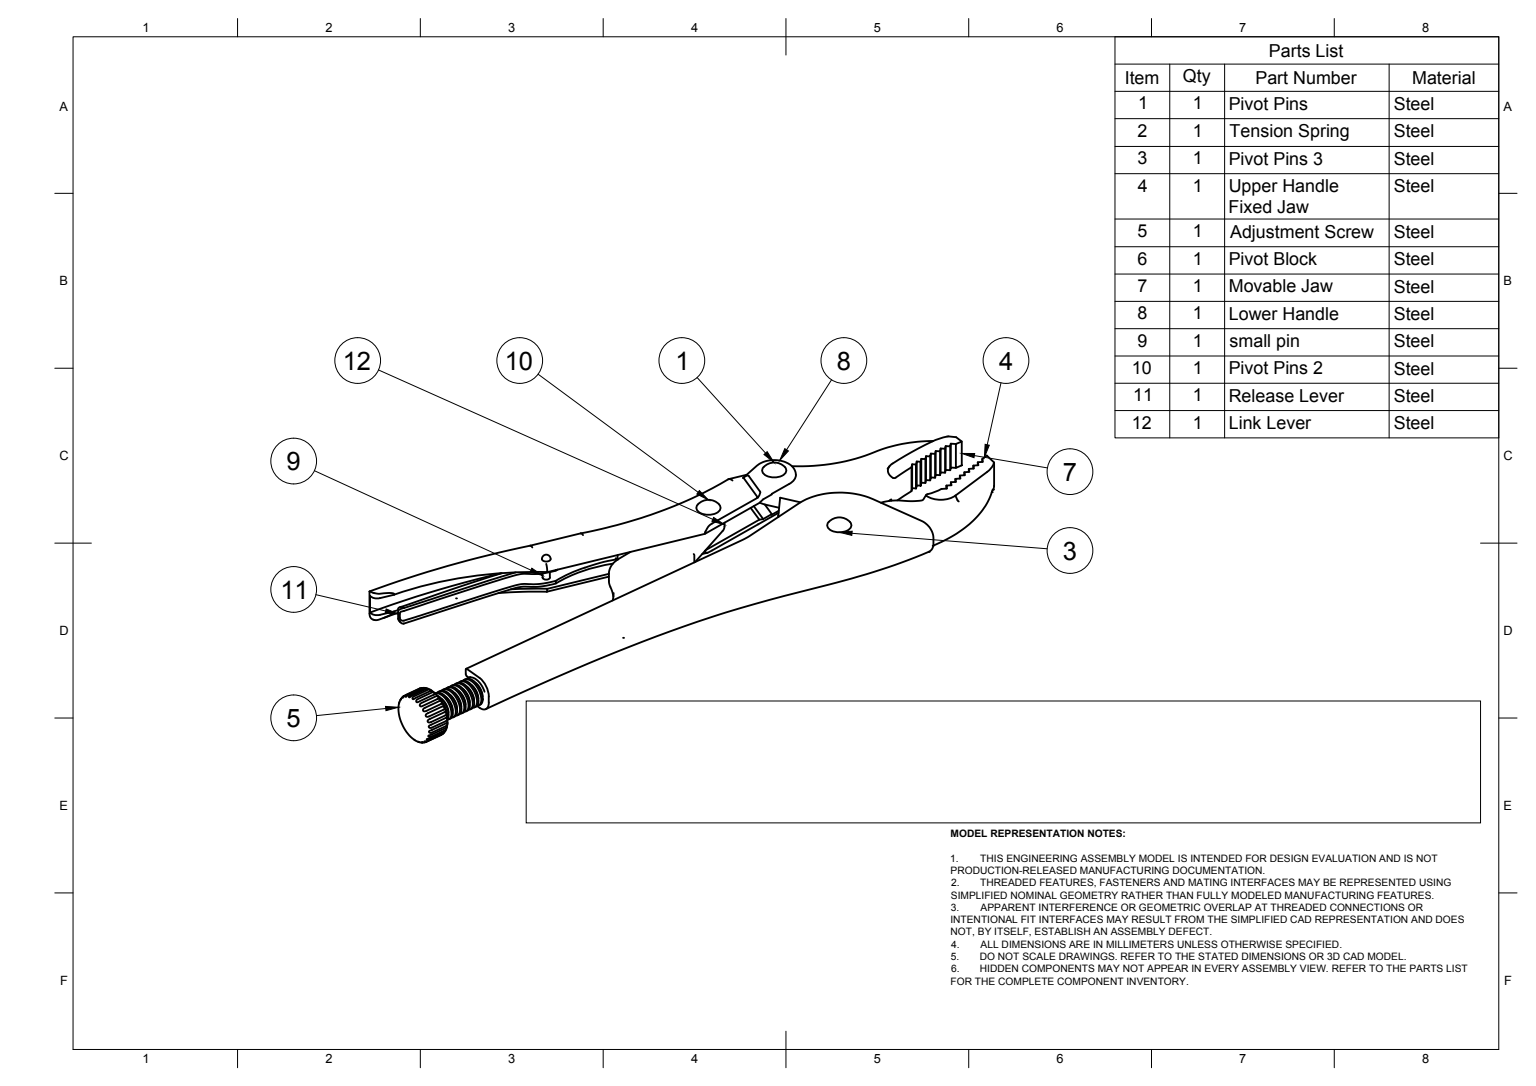
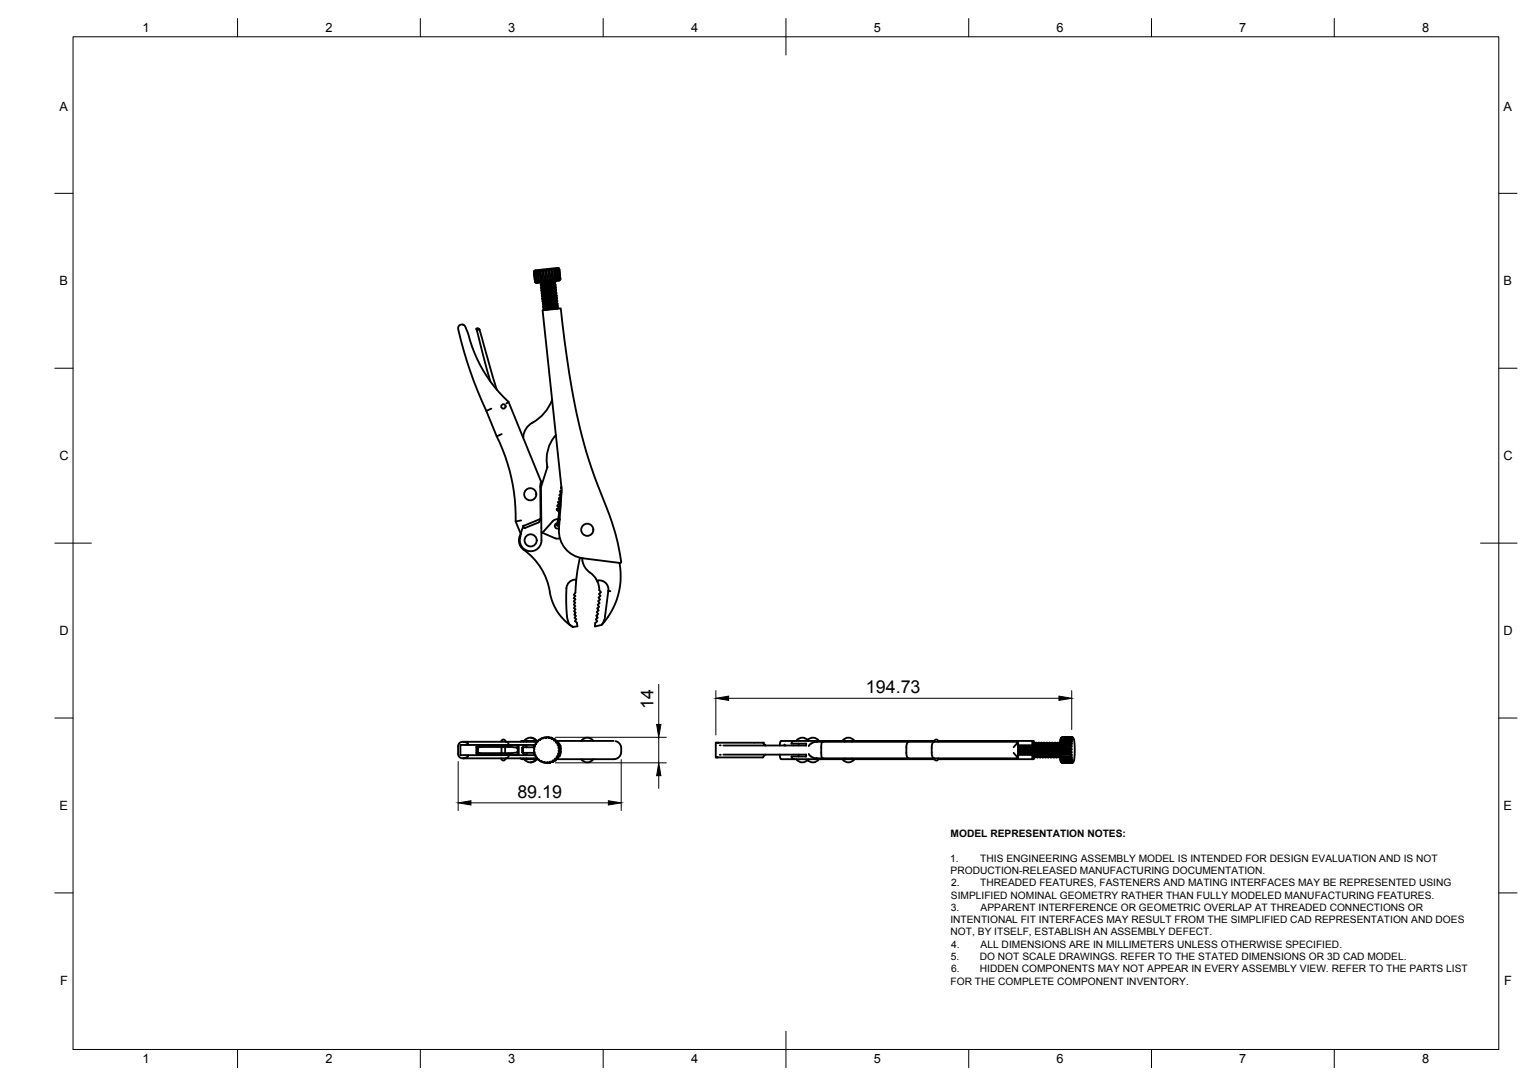
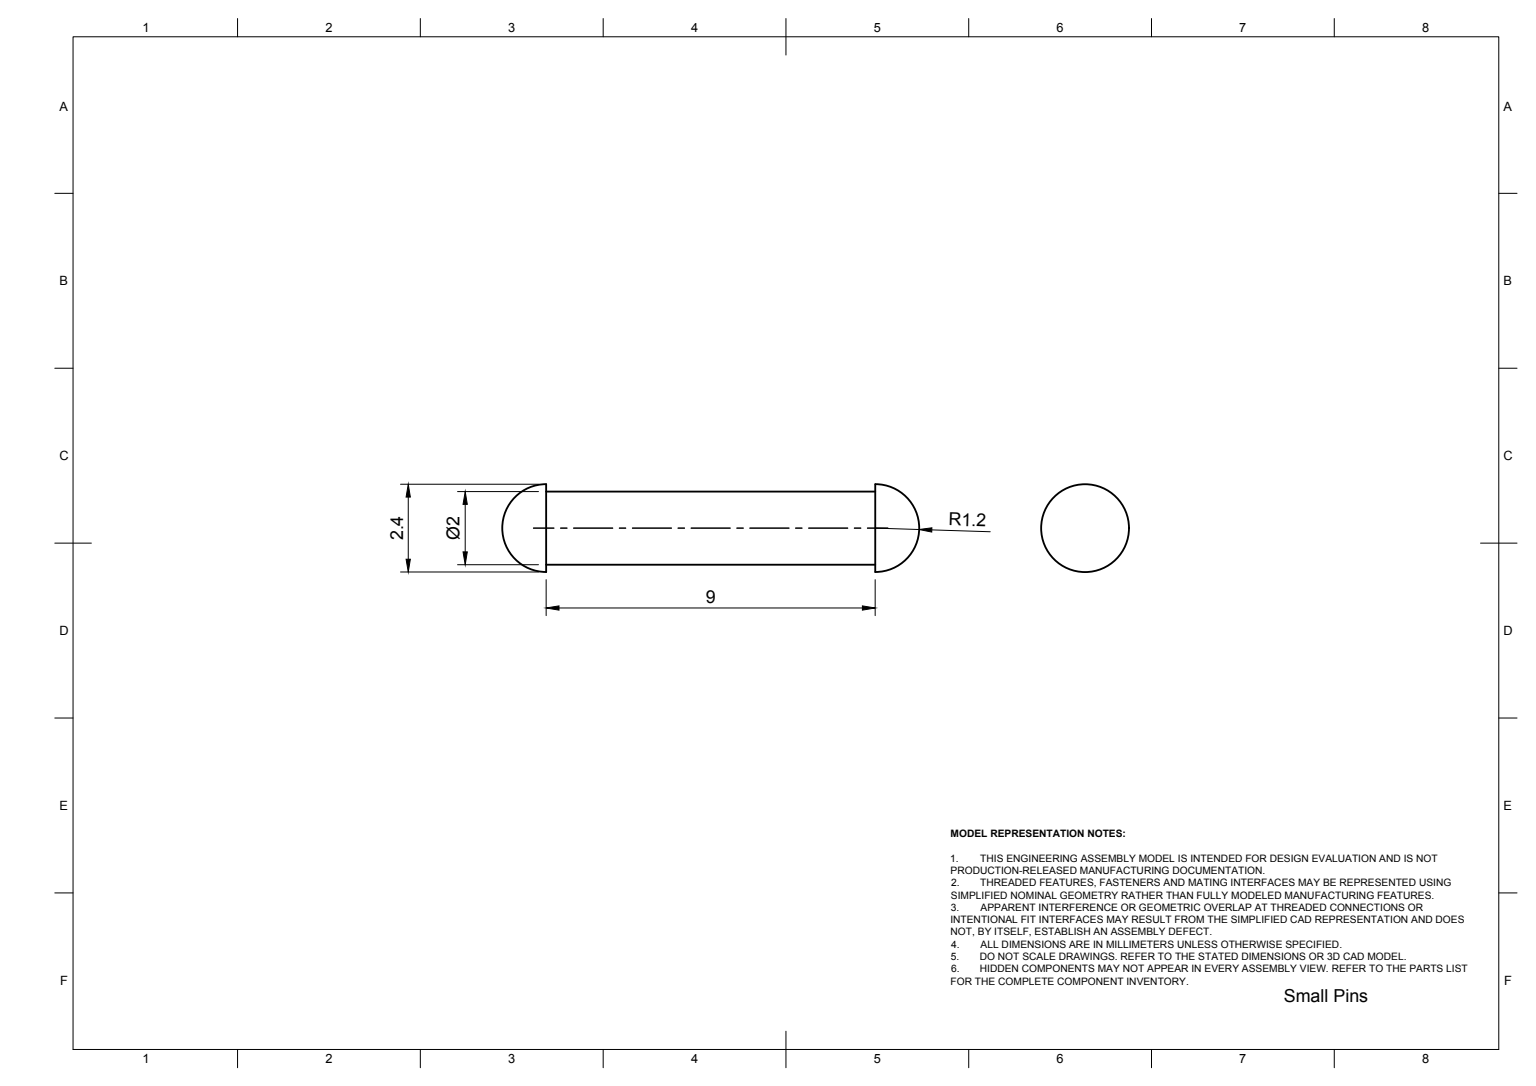
ISO-10303-21;
HEADER;
/* Generated by software containing ST-Developer
 * from STEP Tools, Inc. (www.steptools.com) 
 */

FILE_DESCRIPTION(
/* description */ ('STEP AP214'),
/* implementation_level */ '2;1');

FILE_NAME(
/* name */ 'MAS-610',
/* time_stamp */ '2026-10-06T11:11:25-07:00',
/* author */ (''),
/* organization */ (''),
/* preprocessor_version */ 'ST-DEVELOPER v20.2',
/* originating_system */ 'Autodesk Translation Framework v15.15.0.0',
/* authorisation */ '');

FILE_SCHEMA (('AUTOMOTIVE_DESIGN { 1 0 10303 214 3 1 1 }'));
ENDSEC;

DATA;
#10=MECHANICAL_DESIGN_GEOMETRIC_PRESENTATION_REPRESENTATION('',(#698,#699,
#700,#701,#702,#703,#704,#705,#706,#707,#708,#709),#47717);
#11=ITEM_DEFINED_TRANSFORMATION($,$,#9071,#9944);
#12=ITEM_DEFINED_TRANSFORMATION($,$,#9081,#9945);
#13=ITEM_DEFINED_TRANSFORMATION($,$,#9112,#9946);
#14=ITEM_DEFINED_TRANSFORMATION($,$,#9122,#9947);
#15=ITEM_DEFINED_TRANSFORMATION($,$,#9345,#9948);
#16=ITEM_DEFINED_TRANSFORMATION($,$,#9511,#9949);
#17=ITEM_DEFINED_TRANSFORMATION($,$,#9515,#9950);
#18=ITEM_DEFINED_TRANSFORMATION($,$,#9703,#9951);
#19=ITEM_DEFINED_TRANSFORMATION($,$,#9812,#9952);
#20=ITEM_DEFINED_TRANSFORMATION($,$,#9824,#9953);
#21=ITEM_DEFINED_TRANSFORMATION($,$,#9834,#9954);
#22=ITEM_DEFINED_TRANSFORMATION($,$,#9871,#9955);
#23=(
REPRESENTATION_RELATIONSHIP($,$,#47761,#47760)
REPRESENTATION_RELATIONSHIP_WITH_TRANSFORMATION(#11)
SHAPE_REPRESENTATION_RELATIONSHIP()
);
#24=(
REPRESENTATION_RELATIONSHIP($,$,#47762,#47760)
REPRESENTATION_RELATIONSHIP_WITH_TRANSFORMATION(#12)
SHAPE_REPRESENTATION_RELATIONSHIP()
);
#25=(
REPRESENTATION_RELATIONSHIP($,$,#47763,#47760)
REPRESENTATION_RELATIONSHIP_WITH_TRANSFORMATION(#13)
SHAPE_REPRESENTATION_RELATIONSHIP()
);
#26=(
REPRESENTATION_RELATIONSHIP($,$,#47764,#47760)
REPRESENTATION_RELATIONSHIP_WITH_TRANSFORMATION(#14)
SHAPE_REPRESENTATION_RELATIONSHIP()
);
#27=(
REPRESENTATION_RELATIONSHIP($,$,#47765,#47760)
REPRESENTATION_RELATIONSHIP_WITH_TRANSFORMATION(#15)
SHAPE_REPRESENTATION_RELATIONSHIP()
);
#28=(
REPRESENTATION_RELATIONSHIP($,$,#47766,#47760)
REPRESENTATION_RELATIONSHIP_WITH_TRANSFORMATION(#16)
SHAPE_REPRESENTATION_RELATIONSHIP()
);
#29=(
REPRESENTATION_RELATIONSHIP($,$,#47767,#47760)
REPRESENTATION_RELATIONSHIP_WITH_TRANSFORMATION(#17)
SHAPE_REPRESENTATION_RELATIONSHIP()
);
#30=(
REPRESENTATION_RELATIONSHIP($,$,#47768,#47760)
REPRESENTATION_RELATIONSHIP_WITH_TRANSFORMATION(#18)
SHAPE_REPRESENTATION_RELATIONSHIP()
);
#31=(
REPRESENTATION_RELATIONSHIP($,$,#47769,#47760)
REPRESENTATION_RELATIONSHIP_WITH_TRANSFORMATION(#19)
SHAPE_REPRESENTATION_RELATIONSHIP()
);
#32=(
REPRESENTATION_RELATIONSHIP($,$,#47770,#47760)
REPRESENTATION_RELATIONSHIP_WITH_TRANSFORMATION(#20)
SHAPE_REPRESENTATION_RELATIONSHIP()
);
#33=(
REPRESENTATION_RELATIONSHIP($,$,#47771,#47760)
REPRESENTATION_RELATIONSHIP_WITH_TRANSFORMATION(#21)
SHAPE_REPRESENTATION_RELATIONSHIP()
);
#34=(
REPRESENTATION_RELATIONSHIP($,$,#47772,#47760)
REPRESENTATION_RELATIONSHIP_WITH_TRANSFORMATION(#22)
SHAPE_REPRESENTATION_RELATIONSHIP()
);
#35=CONTEXT_DEPENDENT_SHAPE_REPRESENTATION(#23,#47748);
#36=CONTEXT_DEPENDENT_SHAPE_REPRESENTATION(#24,#47749);
#37=CONTEXT_DEPENDENT_SHAPE_REPRESENTATION(#25,#47750);
#38=CONTEXT_DEPENDENT_SHAPE_REPRESENTATION(#26,#47751);
#39=CONTEXT_DEPENDENT_SHAPE_REPRESENTATION(#27,#47752);
#40=CONTEXT_DEPENDENT_SHAPE_REPRESENTATION(#28,#47753);
#41=CONTEXT_DEPENDENT_SHAPE_REPRESENTATION(#29,#47754);
#42=CONTEXT_DEPENDENT_SHAPE_REPRESENTATION(#30,#47755);
#43=CONTEXT_DEPENDENT_SHAPE_REPRESENTATION(#31,#47756);
#44=CONTEXT_DEPENDENT_SHAPE_REPRESENTATION(#32,#47757);
#45=CONTEXT_DEPENDENT_SHAPE_REPRESENTATION(#33,#47758);
#46=CONTEXT_DEPENDENT_SHAPE_REPRESENTATION(#34,#47759);
#47=NEXT_ASSEMBLY_USAGE_OCCURRENCE('Pivot Pins:1','Pivot Pins:1',
'Pivot Pins:1',#47774,#47775,'Pivot Pins:1');
#48=NEXT_ASSEMBLY_USAGE_OCCURRENCE('Tension Spring:1',
'Tension Spring:1','Tension Spring:1',#47774,#47776,'Tension Spring:1');
#49=NEXT_ASSEMBLY_USAGE_OCCURRENCE('Pivot Pins 3:1','Pivot Pins 3:1',
'Pivot Pins 3:1',#47774,#47777,'Pivot Pins 3:1');
#50=NEXT_ASSEMBLY_USAGE_OCCURRENCE('Upper Handle Fixed Jaw:1',
'Upper Handle Fixed Jaw:1','Upper Handle Fixed Jaw:1',#47774,#47778,
'Upper Handle Fixed Jaw:1');
#51=NEXT_ASSEMBLY_USAGE_OCCURRENCE('Adjustment Screw:1',
'Adjustment Screw:1','Adjustment Screw:1',#47774,#47779,
'Adjustment Screw:1');
#52=NEXT_ASSEMBLY_USAGE_OCCURRENCE('Pivot Block:1','Pivot Block:1',
'Pivot Block:1',#47774,#47780,'Pivot Block:1');
#53=NEXT_ASSEMBLY_USAGE_OCCURRENCE('Movable Jaw:1','Movable Jaw:1',
'Movable Jaw:1',#47774,#47781,'Movable Jaw:1');
#54=NEXT_ASSEMBLY_USAGE_OCCURRENCE('Lower Handle:1','Lower Handle:1',
'Lower Handle:1',#47774,#47782,'Lower Handle:1');
#55=NEXT_ASSEMBLY_USAGE_OCCURRENCE('Small Pin:1','Small Pin:1',
'Small Pin:1',#47774,#47783,'Small Pin:1');
#56=NEXT_ASSEMBLY_USAGE_OCCURRENCE('Pivot Pins 2:1','Pivot Pins 2:1',
'Pivot Pins 2:1',#47774,#47784,'Pivot Pins 2:1');
#57=NEXT_ASSEMBLY_USAGE_OCCURRENCE('Release Lever:1','Release Lever:1',
'Release Lever:1',#47774,#47785,'Release Lever:1');
#58=NEXT_ASSEMBLY_USAGE_OCCURRENCE('Link Lever:1','Link Lever:1',
'Link Lever:1',#47774,#47786,'Link Lever:1');
#59=(
BOUNDED_CURVE()
B_SPLINE_CURVE(2,(#17840,#17841,#17842,#17843,#17844),.UNSPECIFIED.,.F.,
 .F.)
B_SPLINE_CURVE_WITH_KNOTS((3,2,3),(0.0782086527637745,0.0875,0.0968862157575747),
 .UNSPECIFIED.)
CURVE()
GEOMETRIC_REPRESENTATION_ITEM()
RATIONAL_B_SPLINE_CURVE((0.970952227928523,0.943419064382284,1.,0.942841349486679,
0.971523247154132))
REPRESENTATION_ITEM('')
);
#60=(
BOUNDED_CURVE()
B_SPLINE_CURVE(2,(#17845,#17846,#17847,#17848,#17849),.UNSPECIFIED.,.F.,
 .F.)
B_SPLINE_CURVE_WITH_KNOTS((3,2,3),(0.803114463635883,0.8125,0.821791347236166),
 .UNSPECIFIED.)
CURVE()
GEOMETRIC_REPRESENTATION_ITEM()
RATIONAL_B_SPLINE_CURVE((0.971519095495255,0.942845486746487,1.,0.943419064382644,
0.970952227928172))
REPRESENTATION_ITEM('')
);
#61=(
BOUNDED_CURVE()
B_SPLINE_CURVE(2,(#17851,#17852,#17853,#17854,#17855),.UNSPECIFIED.,.F.,
 .F.)
B_SPLINE_CURVE_WITH_KNOTS((3,2,3),(0.178208652763774,0.1875,0.196882250682148),
 .UNSPECIFIED.)
CURVE()
GEOMETRIC_REPRESENTATION_ITEM()
RATIONAL_B_SPLINE_CURVE((0.970952227928523,0.943419064382284,1.,0.942865495358289,
0.971499029940397))
REPRESENTATION_ITEM('')
);
#62=(
BOUNDED_CURVE()
B_SPLINE_CURVE(2,(#17856,#17857,#17858,#17859,#17860),.UNSPECIFIED.,.F.,
 .F.)
B_SPLINE_CURVE_WITH_KNOTS((3,2,3),(0.703119206263016,0.7125,0.721791347236166),
 .UNSPECIFIED.)
CURVE()
GEOMETRIC_REPRESENTATION_ITEM()
RATIONAL_B_SPLINE_CURVE((0.971490139155267,0.942874367626047,1.,0.943419064382644,
0.970952227928173))
REPRESENTATION_ITEM('')
);
#63=(
BOUNDED_CURVE()
B_SPLINE_CURVE(2,(#17862,#17863,#17864,#17865,#17866),.UNSPECIFIED.,.F.,
 .F.)
B_SPLINE_CURVE_WITH_KNOTS((3,2,3),(0.278208652763774,0.2875,0.296875230169318),
 .UNSPECIFIED.)
CURVE()
GEOMETRIC_REPRESENTATION_ITEM()
RATIONAL_B_SPLINE_CURVE((0.970952227928523,0.943419064382284,1.,0.94290824773578,
0.971456226391036))
REPRESENTATION_ITEM('')
);
#64=(
BOUNDED_CURVE()
B_SPLINE_CURVE(2,(#17867,#17868,#17869,#17870,#17871),.UNSPECIFIED.,.F.,
 .F.)
B_SPLINE_CURVE_WITH_KNOTS((3,2,3),(0.603126927215252,0.6125,0.621791347236166),
 .UNSPECIFIED.)
CURVE()
GEOMETRIC_REPRESENTATION_ITEM()
RATIONAL_B_SPLINE_CURVE((0.971443092268521,0.942921385425537,1.,0.943419064382644,
0.970952227928173))
REPRESENTATION_ITEM('')
);
#65=(
BOUNDED_CURVE()
B_SPLINE_CURVE(2,(#17873,#17874,#17875,#17876,#17877),.UNSPECIFIED.,.F.,
 .F.)
B_SPLINE_CURVE_WITH_KNOTS((3,2,3),(0.378208652763774,0.3875,0.396865543999395),
 .UNSPECIFIED.)
CURVE()
GEOMETRIC_REPRESENTATION_ITEM()
RATIONAL_B_SPLINE_CURVE((0.970952227928524,0.943419064382284,1.,0.942967232998394,
0.971397328198516))
REPRESENTATION_ITEM('')
);
#66=(
BOUNDED_CURVE()
B_SPLINE_CURVE(2,(#17878,#17879,#17880,#17881,#17882),.UNSPECIFIED.,.F.,
 .F.)
B_SPLINE_CURVE_WITH_KNOTS((3,2,3),(0.50313718714112,0.5125,0.521791347236167),
 .UNSPECIFIED.)
CURVE()
GEOMETRIC_REPRESENTATION_ITEM()
RATIONAL_B_SPLINE_CURVE((0.971380754136894,0.94298386465382,1.,0.943419064382643,
0.970952227928174))
REPRESENTATION_ITEM('')
);
#67=(
BOUNDED_CURVE()
B_SPLINE_CURVE(2,(#17884,#17885,#17886,#17887,#17888),.UNSPECIFIED.,.F.,
 .F.)
B_SPLINE_CURVE_WITH_KNOTS((3,2,3),(0.478208652763774,0.4875,0.496853778396117),
 .UNSPECIFIED.)
CURVE()
GEOMETRIC_REPRESENTATION_ITEM()
RATIONAL_B_SPLINE_CURVE((0.970952227928524,0.943419064382283,1.,0.94303888125614,
0.971326031620276))
REPRESENTATION_ITEM('')
);
#68=(
BOUNDED_CURVE()
B_SPLINE_CURVE(2,(#17889,#17890,#17891,#17892,#17893),.UNSPECIFIED.,.F.,
 .F.)
B_SPLINE_CURVE_WITH_KNOTS((3,2,3),(0.403149353858237,0.4125,0.421791347236167),
 .UNSPECIFIED.)
CURVE()
GEOMETRIC_REPRESENTATION_ITEM()
RATIONAL_B_SPLINE_CURVE((0.971307096418175,0.943057955549397,1.,0.943419064382643,
0.970952227928173))
REPRESENTATION_ITEM('')
);
#69=(
BOUNDED_CURVE()
B_SPLINE_CURVE(2,(#17895,#17896,#17897,#17898,#17899),.UNSPECIFIED.,.F.,
 .F.)
B_SPLINE_CURVE_WITH_KNOTS((3,2,3),(0.578208652763774,0.5875,0.596840698287781),
 .UNSPECIFIED.)
CURVE()
GEOMETRIC_REPRESENTATION_ITEM()
RATIONAL_B_SPLINE_CURVE((0.970952227928523,0.943419064382284,1.,0.943118534373046,
0.971247086120199))
REPRESENTATION_ITEM('')
);
#70=(
BOUNDED_CURVE()
B_SPLINE_CURVE(2,(#17900,#17901,#17902,#17903,#17904),.UNSPECIFIED.,.F.,
 .F.)
B_SPLINE_CURVE_WITH_KNOTS((3,2,3),(0.303162621990297,0.3125,0.321791347236167),
 .UNSPECIFIED.)
CURVE()
GEOMETRIC_REPRESENTATION_ITEM()
RATIONAL_B_SPLINE_CURVE((0.971227099510026,0.943138753662606,1.,0.943419064382643,
0.970952227928174))
REPRESENTATION_ITEM('')
);
#71=(
BOUNDED_CURVE()
B_SPLINE_CURVE(2,(#17907,#17908,#17909,#17910,#17911),.UNSPECIFIED.,.F.,
 .F.)
B_SPLINE_CURVE_WITH_KNOTS((3,2,3),(0.678208652763775,0.6875,0.691555825853902),
 .UNSPECIFIED.)
CURVE()
GEOMETRIC_REPRESENTATION_ITEM()
RATIONAL_B_SPLINE_CURVE((0.970952227928523,0.943419064382284,1.,0.975301491195852,
0.966630638481416))
REPRESENTATION_ITEM('')
);
#72=(
BOUNDED_CURVE()
B_SPLINE_CURVE(2,(#19973,#19974,#19975,#19976,#19977),.UNSPECIFIED.,.F.,
 .F.)
B_SPLINE_CURVE_WITH_KNOTS((3,2,3),(0.745762259902575,0.75,0.751783130051315),
 .UNSPECIFIED.)
CURVE()
GEOMETRIC_REPRESENTATION_ITEM()
RATIONAL_B_SPLINE_CURVE((0.965885061990929,0.974193699415065,1.,0.989141384552057,
0.981380740867458))
REPRESENTATION_ITEM('')
);
#73=(
BOUNDED_CURVE()
B_SPLINE_CURVE(2,(#20440,#20441,#20442,#20443,#20444,#20445,#20446,#20447,
#20448,#20449,#20450,#20451,#20452,#20453,#20454),.UNSPECIFIED.,.F.,.F.)
B_SPLINE_CURVE_WITH_KNOTS((3,2,2,2,2,2,2,3),(0.673216868607369,0.675,0.6875,
0.7,0.7125,0.725,0.7375,0.745762259902575),.UNSPECIFIED.)
CURVE()
GEOMETRIC_REPRESENTATION_ITEM()
RATIONAL_B_SPLINE_CURVE((0.981380729191956,0.989141376383933,1.,0.923879532511287,
1.,0.923879532511287,1.,0.923879532511287,1.,0.923879532511287,1.,0.923879532511287,
1.,0.949685833096222,0.965885061990929))
REPRESENTATION_ITEM('')
);
#74=(
BOUNDED_CURVE()
B_SPLINE_CURVE(2,(#20777,#20778,#20779,#20780,#20781,#20782,#20783,#20784,
#20785),.UNSPECIFIED.,.F.,.F.)
B_SPLINE_CURVE_WITH_KNOTS((3,2,2,2,3),(0.673216868607369,0.675,0.6875,0.7,
0.712499999279178),.UNSPECIFIED.)
CURVE()
GEOMETRIC_REPRESENTATION_ITEM()
RATIONAL_B_SPLINE_CURVE((0.981380729191956,0.989141376383933,1.,0.923879532511287,
1.,0.923879532511287,1.,0.923879536900831,0.999999991220912))
REPRESENTATION_ITEM('')
);
#75=(
BOUNDED_CURVE()
B_SPLINE_CURVE(2,(#23686,#23687,#23688,#23689,#23690,#23691,#23692,#23693,
#23694,#23695,#23696,#23697,#23698,#23699,#23700,#23701,#23702),
 .UNSPECIFIED.,.F.,.F.)
B_SPLINE_CURVE_WITH_KNOTS((3,2,2,2,2,2,2,2,3),(0.0732168686073693,0.075,
0.0875,0.1,0.1125,0.125,0.1375,0.15,0.151783130051315),.UNSPECIFIED.)
CURVE()
GEOMETRIC_REPRESENTATION_ITEM()
RATIONAL_B_SPLINE_CURVE((0.981380729191956,0.989141376383932,1.,0.923879532511287,
1.,0.923879532511287,1.,0.923879532511287,1.,0.923879532511287,1.,0.923879532511287,
1.,0.923879532511287,1.,0.989141384552058,0.981380740867459))
REPRESENTATION_ITEM('')
);
#76=(
BOUNDED_CURVE()
B_SPLINE_CURVE(2,(#24025,#24026,#24027,#24028,#24029,#24030,#24031,#24032,
#24033,#24034,#24035,#24036,#24037,#24038,#24039),.UNSPECIFIED.,.F.,.F.)
B_SPLINE_CURVE_WITH_KNOTS((3,2,2,2,2,2,2,3),(0.0792377388003687,0.0875,
0.1,0.1125,0.125,0.1375,0.15,0.151783130051315),.UNSPECIFIED.)
CURVE()
GEOMETRIC_REPRESENTATION_ITEM()
RATIONAL_B_SPLINE_CURVE((0.965885067077025,0.949685825197617,1.,0.923879532511287,
1.,0.923879532511287,1.,0.923879532511287,1.,0.923879532511287,1.,0.923879532511287,
1.,0.989141384552057,0.981380740867458))
REPRESENTATION_ITEM('')
);
#77=(
BOUNDED_CURVE()
B_SPLINE_CURVE(2,(#25006,#25007,#25008,#25009,#25010,#25011,#25012,#25013,
#25014,#25015,#25016,#25017,#25018,#25019,#25020,#25021,#25022),
 .UNSPECIFIED.,.F.,.F.)
B_SPLINE_CURVE_WITH_KNOTS((3,2,2,2,2,2,2,2,3),(0.173216868607369,0.175,
0.1875,0.2,0.2125,0.225,0.2375,0.25,0.251783130051315),.UNSPECIFIED.)
CURVE()
GEOMETRIC_REPRESENTATION_ITEM()
RATIONAL_B_SPLINE_CURVE((0.981380729191956,0.989141376383932,1.,0.923879532511287,
1.,0.923879532511287,1.,0.923879532511287,1.,0.923879532511287,1.,0.923879532511287,
1.,0.923879532511287,1.,0.989141384552057,0.981380740867459))
REPRESENTATION_ITEM('')
);
#78=(
BOUNDED_CURVE()
B_SPLINE_CURVE(2,(#25345,#25346,#25347,#25348,#25349,#25350,#25351,#25352,
#25353,#25354,#25355,#25356,#25357,#25358,#25359,#25360,#25361),
 .UNSPECIFIED.,.F.,.F.)
B_SPLINE_CURVE_WITH_KNOTS((3,2,2,2,2,2,2,2,3),(0.173216868607369,0.175,
0.1875,0.2,0.2125,0.225,0.2375,0.25,0.251783130051315),.UNSPECIFIED.)
CURVE()
GEOMETRIC_REPRESENTATION_ITEM()
RATIONAL_B_SPLINE_CURVE((0.981380729191957,0.989141376383933,1.,0.923879532511287,
1.,0.923879532511287,1.,0.923879532511287,1.,0.923879532511287,1.,0.923879532511287,
1.,0.923879532511287,1.,0.989141384552057,0.981380740867459))
REPRESENTATION_ITEM('')
);
#79=(
BOUNDED_CURVE()
B_SPLINE_CURVE(2,(#26328,#26329,#26330,#26331,#26332,#26333,#26334,#26335,
#26336,#26337,#26338,#26339,#26340,#26341,#26342,#26343,#26344),
 .UNSPECIFIED.,.F.,.F.)
B_SPLINE_CURVE_WITH_KNOTS((3,2,2,2,2,2,2,2,3),(0.273216868607369,0.275,
0.2875,0.3,0.3125,0.325,0.3375,0.35,0.351783130051315),.UNSPECIFIED.)
CURVE()
GEOMETRIC_REPRESENTATION_ITEM()
RATIONAL_B_SPLINE_CURVE((0.981380729191956,0.989141376383932,1.,0.923879532511287,
1.,0.923879532511287,1.,0.923879532511287,1.,0.923879532511287,1.,0.923879532511287,
1.,0.923879532511287,1.,0.989141384552056,0.981380740867458))
REPRESENTATION_ITEM('')
);
#80=(
BOUNDED_CURVE()
B_SPLINE_CURVE(2,(#26667,#26668,#26669,#26670,#26671,#26672,#26673,#26674,
#26675,#26676,#26677,#26678,#26679,#26680,#26681,#26682,#26683),
 .UNSPECIFIED.,.F.,.F.)
B_SPLINE_CURVE_WITH_KNOTS((3,2,2,2,2,2,2,2,3),(0.273216868607369,0.275,
0.2875,0.3,0.3125,0.325,0.3375,0.35,0.351783130051315),.UNSPECIFIED.)
CURVE()
GEOMETRIC_REPRESENTATION_ITEM()
RATIONAL_B_SPLINE_CURVE((0.981380729191955,0.989141376383932,1.,0.923879532511287,
1.,0.923879532511287,1.,0.923879532511287,1.,0.923879532511287,1.,0.923879532511287,
1.,0.923879532511287,1.,0.989141384552056,0.981380740867458))
REPRESENTATION_ITEM('')
);
#81=(
BOUNDED_CURVE()
B_SPLINE_CURVE(2,(#27650,#27651,#27652,#27653,#27654,#27655,#27656,#27657,
#27658,#27659,#27660,#27661,#27662,#27663,#27664,#27665,#27666),
 .UNSPECIFIED.,.F.,.F.)
B_SPLINE_CURVE_WITH_KNOTS((3,2,2,2,2,2,2,2,3),(0.373216868607369,0.375,
0.3875,0.4,0.4125,0.425,0.4375,0.45,0.451783130051315),.UNSPECIFIED.)
CURVE()
GEOMETRIC_REPRESENTATION_ITEM()
RATIONAL_B_SPLINE_CURVE((0.981380729191956,0.989141376383932,1.,0.923879532511287,
1.,0.923879532511287,1.,0.923879532511287,1.,0.923879532511287,1.,0.923879532511287,
1.,0.923879532511287,1.,0.989141384552057,0.981380740867459))
REPRESENTATION_ITEM('')
);
#82=(
BOUNDED_CURVE()
B_SPLINE_CURVE(2,(#27989,#27990,#27991,#27992,#27993,#27994,#27995,#27996,
#27997,#27998,#27999,#28000,#28001,#28002,#28003,#28004,#28005),
 .UNSPECIFIED.,.F.,.F.)
B_SPLINE_CURVE_WITH_KNOTS((3,2,2,2,2,2,2,2,3),(0.373216868607369,0.375,
0.3875,0.4,0.4125,0.425,0.4375,0.45,0.451783130051315),.UNSPECIFIED.)
CURVE()
GEOMETRIC_REPRESENTATION_ITEM()
RATIONAL_B_SPLINE_CURVE((0.981380729191956,0.989141376383932,1.,0.923879532511287,
1.,0.923879532511287,1.,0.923879532511287,1.,0.923879532511287,1.,0.923879532511287,
1.,0.923879532511287,1.,0.989141384552056,0.981380740867458))
REPRESENTATION_ITEM('')
);
#83=(
BOUNDED_CURVE()
B_SPLINE_CURVE(2,(#28972,#28973,#28974,#28975,#28976,#28977,#28978,#28979,
#28980,#28981,#28982,#28983,#28984,#28985,#28986,#28987,#28988),
 .UNSPECIFIED.,.F.,.F.)
B_SPLINE_CURVE_WITH_KNOTS((3,2,2,2,2,2,2,2,3),(0.473216868607369,0.475,
0.4875,0.5,0.5125,0.525,0.5375,0.55,0.551783130051315),.UNSPECIFIED.)
CURVE()
GEOMETRIC_REPRESENTATION_ITEM()
RATIONAL_B_SPLINE_CURVE((0.981380729191957,0.989141376383933,1.,0.923879532511287,
1.,0.923879532511287,1.,0.923879532511287,1.,0.923879532511287,1.,0.923879532511287,
1.,0.923879532511287,1.,0.989141384552057,0.981380740867459))
REPRESENTATION_ITEM('')
);
#84=(
BOUNDED_CURVE()
B_SPLINE_CURVE(2,(#29311,#29312,#29313,#29314,#29315,#29316,#29317,#29318,
#29319,#29320,#29321,#29322,#29323,#29324,#29325,#29326,#29327),
 .UNSPECIFIED.,.F.,.F.)
B_SPLINE_CURVE_WITH_KNOTS((3,2,2,2,2,2,2,2,3),(0.473216868607369,0.475,
0.4875,0.5,0.5125,0.525,0.5375,0.55,0.551783130051315),.UNSPECIFIED.)
CURVE()
GEOMETRIC_REPRESENTATION_ITEM()
RATIONAL_B_SPLINE_CURVE((0.981380729191956,0.989141376383932,1.,0.923879532511287,
1.,0.923879532511287,1.,0.923879532511287,1.,0.923879532511287,1.,0.923879532511287,
1.,0.923879532511287,1.,0.989141384552057,0.981380740867459))
REPRESENTATION_ITEM('')
);
#85=(
BOUNDED_CURVE()
B_SPLINE_CURVE(2,(#30294,#30295,#30296,#30297,#30298,#30299,#30300,#30301,
#30302,#30303,#30304,#30305,#30306,#30307,#30308,#30309,#30310),
 .UNSPECIFIED.,.F.,.F.)
B_SPLINE_CURVE_WITH_KNOTS((3,2,2,2,2,2,2,2,3),(0.573216868607369,0.575,
0.5875,0.6,0.6125,0.625,0.6375,0.65,0.651783130051315),.UNSPECIFIED.)
CURVE()
GEOMETRIC_REPRESENTATION_ITEM()
RATIONAL_B_SPLINE_CURVE((0.981380729191957,0.989141376383933,1.,0.923879532511287,
1.,0.923879532511287,1.,0.923879532511287,1.,0.923879532511287,1.,0.923879532511287,
1.,0.923879532511287,1.,0.989141384552057,0.981380740867459))
REPRESENTATION_ITEM('')
);
#86=(
BOUNDED_CURVE()
B_SPLINE_CURVE(2,(#30633,#30634,#30635,#30636,#30637,#30638,#30639,#30640,
#30641,#30642,#30643,#30644,#30645,#30646,#30647,#30648,#30649),
 .UNSPECIFIED.,.F.,.F.)
B_SPLINE_CURVE_WITH_KNOTS((3,2,2,2,2,2,2,2,3),(0.573216868607369,0.575,
0.5875,0.6,0.6125,0.625,0.6375,0.65,0.651783130051315),.UNSPECIFIED.)
CURVE()
GEOMETRIC_REPRESENTATION_ITEM()
RATIONAL_B_SPLINE_CURVE((0.981380729191956,0.989141376383932,1.,0.923879532511287,
1.,0.923879532511287,1.,0.923879532511287,1.,0.923879532511287,1.,0.923879532511287,
1.,0.923879532511287,1.,0.989141384552057,0.981380740867458))
REPRESENTATION_ITEM('')
);
#87=(
BOUNDED_CURVE()
B_SPLINE_CURVE(2,(#31616,#31617,#31618,#31619,#31620),.UNSPECIFIED.,.F.,
 .F.)
B_SPLINE_CURVE_WITH_KNOTS((3,2,3),(0.0457622599025745,0.05,0.0517831300513152),
 .UNSPECIFIED.)
CURVE()
GEOMETRIC_REPRESENTATION_ITEM()
RATIONAL_B_SPLINE_CURVE((0.965885061990928,0.974193699415064,1.,0.989141384552057,
0.981380740867459))
REPRESENTATION_ITEM('')
);
#88=(
BOUNDED_CURVE()
B_SPLINE_CURVE(2,(#38802,#38803,#38804,#38805,#38806,#38807,#38808,#38809,
#38810,#38811,#38812,#38813,#38814,#38815,#38816,#38817,#38818,#38819,#38820,
#38821,#38822,#38823,#38824,#38825,#38826,#38827,#38828,#38829,#38830,#38831,
#38832,#38833,#38834,#38835,#38836,#38837,#38838,#38839,#38840,#38841,#38842,
#38843,#38844,#38845,#38846,#38847,#38848,#38849,#38850,#38851,#38852,#38853,
#38854,#38855,#38856,#38857,#38858,#38859,#38860,#38861,#38862,#38863,#38864,
#38865,#38866,#38867,#38868,#38869,#38870,#38871,#38872,#38873,#38874,#38875,
#38876,#38877,#38878,#38879,#38880,#38881,#38882,#38883,#38884,#38885,#38886,
#38887,#38888,#38889,#38890,#38891,#38892,#38893,#38894,#38895,#38896,#38897,
#38898,#38899,#38900,#38901,#38902,#38903,#38904,#38905,#38906,#38907,#38908,
#38909,#38910,#38911,#38912,#38913,#38914,#38915,#38916,#38917,#38918,#38919,
#38920,#38921,#38922,#38923,#38924,#38925,#38926,#38927,#38928,#38929,#38930,
#38931,#38932,#38933,#38934,#38935,#38936,#38937,#38938,#38939,#38940,#38941,
#38942,#38943,#38944,#38945,#38946,#38947,#38948,#38949,#38950,#38951,#38952,
#38953,#38954,#38955,#38956,#38957,#38958,#38959,#38960,#38961,#38962,#38963,
#38964,#38965,#38966,#38967,#38968,#38969,#38970,#38971,#38972,#38973,#38974,
#38975,#38976,#38977,#38978,#38979,#38980,#38981,#38982,#38983,#38984,#38985,
#38986,#38987,#38988,#38989,#38990,#38991,#38992,#38993,#38994,#38995,#38996,
#38997,#38998,#38999,#39000,#39001,#39002,#39003,#39004,#39005,#39006,#39007,
#39008,#39009,#39010,#39011,#39012,#39013,#39014,#39015,#39016,#39017,#39018,
#39019,#39020,#39021,#39022,#39023,#39024,#39025,#39026,#39027,#39028,#39029,
#39030,#39031,#39032,#39033,#39034,#39035,#39036,#39037,#39038,#39039,#39040,
#39041,#39042,#39043,#39044,#39045,#39046,#39047,#39048,#39049,#39050,#39051,
#39052,#39053,#39054,#39055,#39056,#39057,#39058,#39059,#39060,#39061,#39062,
#39063,#39064,#39065,#39066,#39067,#39068,#39069,#39070,#39071,#39072,#39073,
#39074,#39075,#39076,#39077,#39078,#39079,#39080,#39081,#39082,#39083,#39084,
#39085,#39086,#39087,#39088,#39089,#39090,#39091,#39092,#39093,#39094,#39095,
#39096,#39097,#39098,#39099,#39100,#39101,#39102,#39103,#39104,#39105,#39106,
#39107,#39108,#39109,#39110,#39111,#39112,#39113,#39114,#39115,#39116,#39117,
#39118,#39119,#39120,#39121,#39122,#39123,#39124,#39125,#39126,#39127,#39128,
#39129,#39130,#39131,#39132,#39133,#39134,#39135,#39136,#39137,#39138,#39139,
#39140,#39141,#39142,#39143,#39144,#39145,#39146,#39147,#39148,#39149,#39150,
#39151,#39152,#39153,#39154,#39155,#39156,#39157,#39158,#39159,#39160,#39161,
#39162,#39163,#39164,#39165,#39166,#39167,#39168,#39169,#39170,#39171,#39172,
#39173,#39174,#39175,#39176,#39177,#39178,#39179,#39180,#39181,#39182,#39183,
#39184,#39185,#39186,#39187,#39188,#39189,#39190,#39191,#39192,#39193,#39194,
#39195,#39196,#39197,#39198,#39199,#39200,#39201,#39202,#39203,#39204,#39205,
#39206,#39207,#39208,#39209,#39210,#39211,#39212,#39213,#39214,#39215,#39216,
#39217,#39218,#39219,#39220,#39221,#39222,#39223,#39224,#39225,#39226,#39227,
#39228,#39229,#39230,#39231,#39232,#39233,#39234,#39235,#39236,#39237,#39238,
#39239,#39240,#39241,#39242,#39243,#39244,#39245,#39246,#39247,#39248,#39249,
#39250,#39251,#39252,#39253,#39254,#39255,#39256,#39257,#39258,#39259,#39260,
#39261,#39262,#39263,#39264,#39265,#39266,#39267,#39268,#39269,#39270,#39271,
#39272,#39273,#39274,#39275,#39276,#39277,#39278,#39279,#39280,#39281,#39282,
#39283,#39284,#39285,#39286,#39287,#39288,#39289,#39290,#39291,#39292,#39293,
#39294,#39295,#39296,#39297,#39298,#39299,#39300,#39301,#39302,#39303,#39304,
#39305,#39306,#39307,#39308,#39309,#39310,#39311,#39312,#39313,#39314,#39315,
#39316,#39317,#39318,#39319,#39320,#39321,#39322,#39323,#39324,#39325,#39326,
#39327,#39328,#39329,#39330,#39331,#39332,#39333,#39334,#39335,#39336,#39337,
#39338,#39339,#39340,#39341,#39342,#39343,#39344,#39345,#39346,#39347,#39348,
#39349,#39350,#39351,#39352,#39353,#39354,#39355,#39356,#39357,#39358,#39359,
#39360,#39361,#39362,#39363,#39364,#39365,#39366,#39367,#39368,#39369,#39370,
#39371,#39372,#39373,#39374,#39375,#39376,#39377,#39378,#39379,#39380,#39381,
#39382,#39383,#39384,#39385,#39386,#39387,#39388,#39389,#39390,#39391,#39392,
#39393,#39394,#39395,#39396,#39397,#39398,#39399,#39400,#39401,#39402,#39403,
#39404,#39405,#39406,#39407,#39408,#39409,#39410,#39411,#39412,#39413,#39414,
#39415,#39416,#39417,#39418,#39419,#39420,#39421,#39422,#39423,#39424,#39425,
#39426,#39427,#39428,#39429,#39430,#39431,#39432,#39433,#39434,#39435,#39436,
#39437,#39438,#39439,#39440,#39441,#39442,#39443,#39444),.UNSPECIFIED.,
 .F.,.F.)
B_SPLINE_CURVE_WITH_KNOTS((3,2,2,2,2,2,2,2,2,2,2,2,2,2,2,2,2,2,2,2,2,2,
2,2,2,2,2,2,2,2,2,2,2,2,2,2,2,2,2,2,2,2,2,2,2,2,2,2,2,2,2,2,2,2,2,2,2,2,
2,2,2,2,2,2,2,2,2,2,2,2,2,2,2,2,2,2,2,2,2,2,2,2,2,2,2,2,2,2,2,2,2,2,2,2,
2,2,2,2,2,2,2,2,2,2,2,2,2,2,2,2,2,2,2,2,2,2,2,2,2,2,2,2,2,2,2,2,2,2,2,2,
2,2,2,2,2,2,2,2,2,2,2,2,2,2,2,2,2,2,2,2,2,2,2,2,2,2,2,2,2,2,2,2,2,2,2,2,
2,2,2,2,2,2,2,2,2,2,2,2,2,2,2,2,2,2,2,2,2,2,2,2,2,2,2,2,2,2,2,2,2,2,2,2,
2,2,2,2,2,2,2,2,2,2,2,2,2,2,2,2,2,2,2,2,2,2,2,2,2,2,2,2,2,2,2,2,2,2,2,2,
2,2,2,2,2,2,2,2,2,2,2,2,2,2,2,2,2,2,2,2,2,2,2,2,2,2,2,2,2,2,2,2,2,2,2,2,
2,2,2,2,2,2,2,2,2,2,2,2,2,2,2,2,2,2,2,2,2,2,2,2,2,2,2,2,2,2,2,2,2,2,2,2,
2,2,2,2,2,2,2,2,2,2,2,3),(0.0125164708018431,0.0144231574970549,0.0173077889964661,
0.0201924204958774,0.0230770519952887,0.0259616834947,0.0288463149941112,
0.0317309464935225,0.0346155779929338,0.037500209492345,0.0403848409917563,
0.0432694724911676,0.0461541039905789,0.0490387354899901,0.0519233669894014,
0.0548079984888127,0.057692629988224,0.0605772614876352,0.0634618929870465,
0.0663465244864578,0.069231155985869,0.0721157874852803,0.0750004189846916,
0.0778850504841029,0.0807696819835141,0.0836543134829254,0.0865389449823367,
0.089423576481748,0.0923082079811592,0.0951928394805705,0.0980774709799818,
0.100962102479393,0.103846733978804,0.106731365478216,0.109615996977627,
0.112500628477038,0.115385259976449,0.118269891475861,0.121154522975272,
0.124039154474683,0.126923785974095,0.129808417473506,0.132693048972917,
0.135577680472328,0.13846231197174,0.141346943471151,0.144231574970562,
0.147116206469973,0.150000837969385,0.152885469468796,0.155770100968207,
0.158654732467619,0.16153936396703,0.164423995466441,0.167308626965852,
0.170193258465264,0.173077889964675,0.175962521464086,0.178847152963497,
0.181731784462909,0.18461641596232,0.187501047461731,0.190385678961143,
0.193270310460554,0.196154941959965,0.199039573459376,0.201924204958788,
0.204808836458199,0.20769346795761,0.210578099457021,0.213462730956433,
0.216347362455844,0.219231993955255,0.222116625454667,0.225001256954078,
0.227885888453489,0.2307705199529,0.233655151452312,0.236539782951723,0.239424414451134,
0.242309045950545,0.245193677449957,0.248078308949368,0.250962940448779,
0.253847571948191,0.256732203447602,0.259616834947013,0.262501466446424,
0.265386097945836,0.268270729445247,0.271155360944658,0.274039992444069,
0.276924623943481,0.279809255442892,0.282693886942303,0.285578518441715,
0.288463149941126,0.291347781440537,0.294232412939948,0.29711704443936,
0.300001675938771,0.302886307438182,0.305770938937593,0.308655570437005,
0.311540201936416,0.314424833435827,0.317309464935239,0.32019409643465,
0.323078727934061,0.325963359433472,0.328847990932884,0.331732622432295,
0.334617253931706,0.337501885431117,0.340386516930529,0.34327114842994,
0.346155779929351,0.349040411428763,0.351925042928174,0.354809674427585,
0.357694305926996,0.360578937426408,0.363463568925819,0.36634820042523,
0.369232831924641,0.372117463424053,0.375002094923464,0.377886726422875,
0.380771357922287,0.383655989421698,0.386540620921109,0.38942525242052,
0.392309883919932,0.395194515419343,0.398079146918754,0.400963778418165,
0.403848409917577,0.406733041416988,0.409617672916399,0.412502304415811,
0.415386935915222,0.418271567414633,0.421156198914044,0.424040830413456,
0.426925461912867,0.429810093412278,0.432694724911689,0.435579356411101,
0.438463987910512,0.441348619409923,0.444233250909335,0.447117882408746,
0.450002513908157,0.452887145407568,0.45577177690698,0.458656408406391,
0.461541039905802,0.464425671405213,0.467310302904625,0.470194934404036,
0.473079565903447,0.475964197402859,0.47884882890227,0.481733460401681,
0.484618091901092,0.487502723400504,0.490387354899915,0.493271986399326,
0.496156617898737,0.499041249398149,0.50192588089756,0.504810512396971,
0.507695143896382,0.510579775395794,0.513464406895205,0.516349038394616,
0.519233669894028,0.522118301393439,0.52500293289285,0.527887564392261,
0.530772195891673,0.533656827391084,0.536541458890495,0.539426090389907,
0.542310721889318,0.545195353388729,0.54807998488814,0.550964616387552,
0.553849247886963,0.556733879386374,0.559618510885786,0.562503142385197,
0.565387773884608,0.568272405384019,0.571157036883431,0.574041668382842,
0.576926299882253,0.579810931381664,0.582695562881076,0.585580194380487,
0.588464825879898,0.591349457379309,0.594234088878721,0.597118720378132,
0.600003351877543,0.602887983376955,0.605772614876366,0.608657246375777,
0.611541877875188,0.6144265093746,0.617311140874011,0.620195772373422,0.623080403872833,
0.625965035372245,0.628849666871656,0.631734298371067,0.634618929870479,
0.63750356136989,0.640388192869301,0.643272824368712,0.646157455868124,
0.649042087367535,0.651926718866946,0.654811350366358,0.657695981865769,
0.66058061336518,0.663465244864591,0.666349876364003,0.669234507863414,
0.672119139362825,0.675003770862236,0.677888402361648,0.680773033861059,
0.68365766536047,0.686542296859882,0.689426928359293,0.692311559858704,
0.695196191358115,0.698080822857527,0.700965454356938,0.703850085856349,
0.70673471735576,0.709619348855172,0.712503980354583,0.715388611853994,
0.718273243353405,0.721157874852817,0.724042506352228,0.726927137851639,
0.729811769351051,0.732696400850462,0.735581032349873,0.738465663849284,
0.741350295348696,0.744234926848107,0.747119558347518,0.75000418984693,
0.752888821346341,0.755773452845752,0.758658084345163,0.761542715844575,
0.764427347343986,0.767311978843397,0.770196610342808,0.77308124184222,
0.775965873341631,0.778850504841042,0.781735136340453,0.784619767839865,
0.787504399339276,0.790389030838687,0.793273662338098,0.79615829383751,
0.799042925336921,0.801927556836332,0.804812188335744,0.807696819835155,
0.810581451334566,0.813466082833978,0.816350714333389,0.8192353458328,0.822119977332211,
0.825004608831623,0.827889240331034,0.830773871830445,0.833658503329856,
0.836543134829268,0.839427766328679,0.84231239782809,0.845197029327502,
0.848081660826913,0.850966292326324,0.853850923825735,0.856735555325147,
0.859620186824558,0.862504818323969,0.86538944982338,0.868274081322792,
0.871158712822203,0.874043344321614,0.876927975821026,0.879812607320437,
0.882697238819848,0.885581870319259,0.888466501818671,0.891351133318082,
0.894235764817493,0.897120396316904,0.900005027816316,0.902889659315727,
0.905774290815138,0.908658922314549,0.911543553813961,0.914428185313372,
0.917312816812783,0.920197448312195,0.923082079811606,0.925966711311017,
0.928851342810428,0.93173597430984,0.934620605809251,0.935598550613399),
 .UNSPECIFIED.)
CURVE()
GEOMETRIC_REPRESENTATION_ITEM()
RATIONAL_B_SPLINE_CURVE((0.965885073571149,0.949685815112381,1.,0.923879532511287,
1.,0.923879532511287,1.,0.923879532511287,1.,0.923879532511287,1.,0.923879532511287,
1.,0.923879532511287,1.,0.923879532511287,1.,0.923879532511287,1.,0.923879532511287,
1.,0.923879532511287,1.,0.923879532511287,1.,0.923879532511287,1.,0.923879532511287,
1.,0.923879532511287,1.,0.923879532511287,1.,0.923879532511287,1.,0.923879532511287,
1.,0.923879532511287,1.,0.923879532511287,1.,0.923879532511287,1.,0.923879532511287,
1.,0.923879532511287,1.,0.923879532511287,1.,0.923879532511287,1.,0.923879532511287,
1.,0.923879532511287,1.,0.923879532511287,1.,0.923879532511287,1.,0.923879532511287,
1.,0.923879532511287,1.,0.923879532511287,1.,0.923879532511287,1.,0.923879532511287,
1.,0.923879532511287,1.,0.923879532511287,1.,0.923879532511287,1.,0.923879532511287,
1.,0.923879532511287,1.,0.923879532511287,1.,0.923879532511287,1.,0.923879532511287,
1.,0.923879532511287,1.,0.923879532511287,1.,0.923879532511287,1.,0.923879532511287,
1.,0.923879532511287,1.,0.923879532511287,1.,0.923879532511287,1.,0.923879532511287,
1.,0.923879532511287,1.,0.923879532511287,1.,0.923879532511287,1.,0.923879532511287,
1.,0.923879532511287,1.,0.923879532511287,1.,0.923879532511287,1.,0.923879532511287,
1.,0.923879532511287,1.,0.923879532511287,1.,0.923879532511287,1.,0.923879532511287,
1.,0.923879532511287,1.,0.923879532511287,1.,0.923879532511287,1.,0.923879532511287,
1.,0.923879532511287,1.,0.923879532511287,1.,0.923879532511287,1.,0.923879532511287,
1.,0.923879532511287,1.,0.923879532511287,1.,0.923879532511287,1.,0.923879532511287,
1.,0.923879532511287,1.,0.923879532511287,1.,0.923879532511287,1.,0.923879532511287,
1.,0.923879532511287,1.,0.923879532511287,1.,0.923879532511287,1.,0.923879532511287,
1.,0.923879532511287,1.,0.923879532511287,1.,0.923879532511287,1.,0.923879532511287,
1.,0.923879532511287,1.,0.923879532511287,1.,0.923879532511287,1.,0.923879532511287,
1.,0.923879532511287,1.,0.923879532511287,1.,0.923879532511287,1.,0.923879532511287,
1.,0.923879532511287,1.,0.923879532511287,1.,0.923879532511287,1.,0.923879532511287,
1.,0.923879532511287,1.,0.923879532511287,1.,0.923879532511287,1.,0.923879532511287,
1.,0.923879532511287,1.,0.923879532511287,1.,0.923879532511287,1.,0.923879532511287,
1.,0.923879532511287,1.,0.923879532511287,1.,0.923879532511287,1.,0.923879532511287,
1.,0.923879532511287,1.,0.923879532511287,1.,0.923879532511287,1.,0.923879532511287,
1.,0.923879532511287,1.,0.923879532511287,1.,0.923879532511287,1.,0.923879532511287,
1.,0.923879532511287,1.,0.923879532511287,1.,0.923879532511287,1.,0.923879532511287,
1.,0.923879532511287,1.,0.923879532511287,1.,0.923879532511287,1.,0.923879532511287,
1.,0.923879532511287,1.,0.923879532511287,1.,0.923879532511287,1.,0.923879532511287,
1.,0.923879532511287,1.,0.923879532511287,1.,0.923879532511287,1.,0.923879532511287,
1.,0.923879532511287,1.,0.923879532511287,1.,0.923879532511287,1.,0.923879532511287,
1.,0.923879532511287,1.,0.923879532511287,1.,0.923879532511287,1.,0.923879532511287,
1.,0.923879532511287,1.,0.923879532511287,1.,0.923879532511287,1.,0.923879532511287,
1.,0.923879532511287,1.,0.923879532511287,1.,0.923879532511287,1.,0.923879532511287,
1.,0.923879532511287,1.,0.923879532511287,1.,0.923879532511287,1.,0.923879532511287,
1.,0.923879532511287,1.,0.923879532511287,1.,0.923879532511287,1.,0.923879532511287,
1.,0.923879532511287,1.,0.923879532511287,1.,0.923879532511287,1.,0.923879532511287,
1.,0.923879532511287,1.,0.923879532511287,1.,0.923879532511287,1.,0.923879532511287,
1.,0.923879532511287,1.,0.923879532511287,1.,0.923879532511287,1.,0.923879532511287,
1.,0.923879532511287,1.,0.923879532511287,1.,0.923879532511287,1.,0.923879532511287,
1.,0.923879532511287,1.,0.923879532511287,1.,0.923879532511287,1.,0.923879532511287,
1.,0.923879532511287,1.,0.923879532511287,1.,0.923879532511287,1.,0.923879532511287,
1.,0.923879532511287,1.,0.923879532511287,1.,0.923879532511287,1.,0.923879532511287,
1.,0.923879532511287,1.,0.923879532511287,1.,0.923879532511287,1.,0.923879532511287,
1.,0.923879532511287,1.,0.923879532511287,1.,0.923879532511287,1.,0.923879532511287,
1.,0.923879532511287,1.,0.923879532511287,1.,0.923879532511287,1.,0.923879532511287,
1.,0.923879532511287,1.,0.923879532511287,1.,0.923879532511287,1.,0.923879532511287,
1.,0.923879532511287,1.,0.923879532511287,1.,0.923879532511287,1.,0.923879532511287,
1.,0.923879532511287,1.,0.923879532511287,1.,0.923879532511287,1.,0.923879532511287,
1.,0.923879532511287,1.,0.923879532511287,1.,0.923879532511287,1.,0.923879532511287,
1.,0.923879532511287,1.,0.923879532511287,1.,0.923879532511287,1.,0.923879532511287,
1.,0.923879532511287,1.,0.923879532511287,1.,0.923879532511287,1.,0.923879532511287,
1.,0.923879532511287,1.,0.923879532511287,1.,0.923879532511287,1.,0.923879532511287,
1.,0.923879532511287,1.,0.923879532511287,1.,0.923879532511287,1.,0.923879532511287,
1.,0.923879532511287,1.,0.923879532511287,1.,0.923879532511287,1.,0.923879532511287,
1.,0.923879532511287,1.,0.923879532511287,1.,0.923879532511287,1.,0.923879532511287,
1.,0.923879532511287,1.,0.923879532511287,1.,0.923879532511287,1.,0.923879532511287,
1.,0.923879532511287,1.,0.923879532511287,1.,0.923879532511287,1.,0.923879532511287,
1.,0.923879532511287,1.,0.923879532511287,1.,0.923879532511287,1.,0.923879532511287,
1.,0.923879532511287,1.,0.923879532511287,1.,0.923879532511287,1.,0.923879532511287,
1.,0.923879532511287,1.,0.923879532511287,1.,0.923879532511287,1.,0.923879532511287,
1.,0.923879532511287,1.,0.923879532511287,1.,0.923879532511287,1.,0.923879532511287,
1.,0.923879532511287,1.,0.923879532511287,1.,0.923879532511287,1.,0.923879532511287,
1.,0.923879532511287,1.,0.923879532511287,1.,0.923879532511287,1.,0.923879532511287,
1.,0.923879532511287,1.,0.923879532511287,1.,0.923879532511287,1.,0.923879532511287,
1.,0.923879532511287,1.,0.923879532511287,1.,0.923879532511287,1.,0.923879532511287,
1.,0.923879532511287,1.,0.923879532511287,1.,0.923879532511287,1.,0.923879532511287,
1.,0.923879532511287,1.,0.923879532511287,1.,0.923879532511287,1.,0.923879532511287,
1.,0.923879532511287,1.,0.923879532511287,1.,0.923879532511287,1.,0.923879532511287,
1.,0.923879532511287,1.,0.923879532511287,1.,0.923879532511287,1.,0.923879532511287,
1.,0.923879532511287,1.,0.923879532511287,1.,0.923879532511287,1.,0.923879532511287,
1.,0.923879532511287,1.,0.923879532511287,1.,0.923879532511287,1.,0.923879532511287,
1.,0.923879532511287,1.,0.923879532511287,1.,0.923879532511287,1.,0.923879532511287,
1.,0.923879532511287,1.,0.923879532511287,1.,0.923879532511287,1.,0.923879532511287,
1.,0.923879532511287,1.,0.923879532511287,1.,0.923879532511287,1.,0.923879532511287,
1.,0.923879532511287,1.,0.923879532511287,1.,0.923879532511287,1.,0.923879532511287,
1.,0.923879532511287,1.,0.923879532511287,1.,0.974193717400275,0.965885073572031))
REPRESENTATION_ITEM('')
);
#89=(
BOUNDED_CURVE()
B_SPLINE_CURVE(2,(#40835,#40836,#40837,#40838,#40839,#40840,#40841,#40842,
#40843,#40844,#40845,#40846,#40847,#40848,#40849,#40850,#40851,#40852,#40853,
#40854,#40855,#40856,#40857,#40858,#40859,#40860,#40861,#40862,#40863,#40864,
#40865,#40866,#40867,#40868,#40869,#40870,#40871,#40872,#40873,#40874,#40875,
#40876,#40877,#40878,#40879,#40880,#40881,#40882,#40883,#40884,#40885,#40886,
#40887,#40888,#40889,#40890,#40891,#40892,#40893,#40894,#40895,#40896,#40897,
#40898,#40899,#40900,#40901,#40902,#40903,#40904,#40905,#40906,#40907,#40908,
#40909,#40910,#40911,#40912,#40913,#40914,#40915,#40916,#40917,#40918,#40919,
#40920,#40921,#40922,#40923,#40924,#40925,#40926,#40927,#40928,#40929,#40930,
#40931,#40932,#40933,#40934,#40935,#40936,#40937,#40938,#40939,#40940,#40941,
#40942,#40943,#40944,#40945,#40946,#40947,#40948,#40949,#40950,#40951,#40952,
#40953,#40954,#40955,#40956,#40957,#40958,#40959,#40960,#40961,#40962,#40963,
#40964,#40965,#40966,#40967,#40968,#40969,#40970,#40971,#40972,#40973,#40974,
#40975,#40976,#40977,#40978,#40979,#40980,#40981,#40982,#40983,#40984,#40985,
#40986,#40987,#40988,#40989,#40990,#40991,#40992,#40993,#40994,#40995,#40996,
#40997,#40998,#40999,#41000,#41001,#41002,#41003,#41004,#41005,#41006,#41007,
#41008,#41009,#41010,#41011,#41012,#41013,#41014,#41015,#41016,#41017,#41018,
#41019,#41020,#41021,#41022,#41023,#41024,#41025,#41026,#41027,#41028,#41029,
#41030,#41031,#41032,#41033,#41034,#41035,#41036,#41037,#41038,#41039,#41040,
#41041,#41042,#41043,#41044,#41045,#41046,#41047,#41048,#41049,#41050,#41051,
#41052,#41053,#41054,#41055,#41056,#41057,#41058,#41059,#41060,#41061,#41062,
#41063,#41064,#41065,#41066,#41067,#41068,#41069,#41070,#41071,#41072,#41073,
#41074,#41075,#41076,#41077,#41078,#41079,#41080,#41081,#41082,#41083,#41084,
#41085,#41086,#41087,#41088,#41089,#41090,#41091,#41092,#41093,#41094,#41095,
#41096,#41097,#41098,#41099,#41100,#41101,#41102,#41103,#41104,#41105,#41106,
#41107,#41108,#41109,#41110,#41111,#41112,#41113,#41114,#41115,#41116,#41117,
#41118,#41119,#41120,#41121,#41122,#41123,#41124,#41125,#41126,#41127,#41128,
#41129,#41130,#41131,#41132,#41133,#41134,#41135,#41136,#41137,#41138,#41139,
#41140,#41141,#41142,#41143,#41144,#41145,#41146,#41147,#41148,#41149,#41150,
#41151,#41152,#41153,#41154,#41155,#41156,#41157,#41158,#41159,#41160,#41161,
#41162,#41163,#41164,#41165,#41166,#41167,#41168,#41169,#41170,#41171,#41172,
#41173,#41174,#41175,#41176,#41177,#41178,#41179,#41180,#41181,#41182,#41183,
#41184,#41185,#41186,#41187,#41188,#41189,#41190,#41191,#41192,#41193,#41194,
#41195,#41196,#41197,#41198,#41199,#41200,#41201,#41202,#41203,#41204,#41205,
#41206,#41207,#41208,#41209,#41210,#41211,#41212,#41213,#41214,#41215,#41216,
#41217,#41218,#41219,#41220,#41221,#41222,#41223,#41224,#41225,#41226,#41227,
#41228,#41229,#41230,#41231,#41232,#41233,#41234,#41235,#41236,#41237,#41238,
#41239,#41240,#41241,#41242,#41243,#41244,#41245,#41246,#41247,#41248,#41249,
#41250,#41251,#41252,#41253,#41254,#41255,#41256,#41257,#41258,#41259,#41260,
#41261,#41262,#41263,#41264,#41265,#41266,#41267,#41268,#41269,#41270,#41271,
#41272,#41273,#41274,#41275,#41276,#41277,#41278,#41279,#41280,#41281,#41282,
#41283,#41284,#41285,#41286,#41287,#41288,#41289,#41290,#41291,#41292,#41293,
#41294,#41295,#41296,#41297,#41298,#41299,#41300,#41301,#41302,#41303,#41304,
#41305,#41306,#41307,#41308,#41309,#41310,#41311,#41312,#41313,#41314,#41315,
#41316,#41317,#41318,#41319,#41320,#41321,#41322,#41323,#41324,#41325,#41326,
#41327,#41328,#41329,#41330,#41331,#41332,#41333,#41334,#41335,#41336,#41337,
#41338,#41339,#41340,#41341,#41342,#41343,#41344,#41345,#41346,#41347,#41348,
#41349,#41350,#41351,#41352,#41353,#41354,#41355,#41356,#41357,#41358,#41359,
#41360,#41361,#41362,#41363,#41364,#41365,#41366,#41367,#41368,#41369,#41370,
#41371,#41372,#41373,#41374,#41375,#41376,#41377,#41378,#41379,#41380,#41381,
#41382,#41383,#41384,#41385,#41386,#41387,#41388,#41389,#41390,#41391,#41392,
#41393,#41394,#41395,#41396,#41397,#41398,#41399,#41400,#41401,#41402,#41403,
#41404,#41405,#41406,#41407,#41408,#41409,#41410,#41411,#41412,#41413,#41414,
#41415,#41416,#41417,#41418,#41419,#41420,#41421,#41422,#41423,#41424,#41425,
#41426,#41427,#41428,#41429,#41430,#41431,#41432,#41433,#41434,#41435,#41436,
#41437,#41438,#41439,#41440,#41441,#41442,#41443,#41444,#41445,#41446,#41447,
#41448,#41449,#41450,#41451,#41452,#41453,#41454,#41455,#41456,#41457,#41458,
#41459,#41460,#41461,#41462,#41463,#41464,#41465,#41466,#41467,#41468,#41469,
#41470,#41471,#41472,#41473,#41474,#41475,#41476,#41477),.UNSPECIFIED.,
 .F.,.F.)
B_SPLINE_CURVE_WITH_KNOTS((3,2,2,2,2,2,2,2,2,2,2,2,2,2,2,2,2,2,2,2,2,2,
2,2,2,2,2,2,2,2,2,2,2,2,2,2,2,2,2,2,2,2,2,2,2,2,2,2,2,2,2,2,2,2,2,2,2,2,
2,2,2,2,2,2,2,2,2,2,2,2,2,2,2,2,2,2,2,2,2,2,2,2,2,2,2,2,2,2,2,2,2,2,2,2,
2,2,2,2,2,2,2,2,2,2,2,2,2,2,2,2,2,2,2,2,2,2,2,2,2,2,2,2,2,2,2,2,2,2,2,2,
2,2,2,2,2,2,2,2,2,2,2,2,2,2,2,2,2,2,2,2,2,2,2,2,2,2,2,2,2,2,2,2,2,2,2,2,
2,2,2,2,2,2,2,2,2,2,2,2,2,2,2,2,2,2,2,2,2,2,2,2,2,2,2,2,2,2,2,2,2,2,2,2,
2,2,2,2,2,2,2,2,2,2,2,2,2,2,2,2,2,2,2,2,2,2,2,2,2,2,2,2,2,2,2,2,2,2,2,2,
2,2,2,2,2,2,2,2,2,2,2,2,2,2,2,2,2,2,2,2,2,2,2,2,2,2,2,2,2,2,2,2,2,2,2,2,
2,2,2,2,2,2,2,2,2,2,2,2,2,2,2,2,2,2,2,2,2,2,2,2,2,2,2,2,2,2,2,2,2,2,2,2,
2,2,2,2,2,2,2,2,2,2,2,3),(0.0047186950560118,0.00568181818181818,0.00852272727272727,
0.0113636363636364,0.0142045454545455,0.0170454545454545,0.0198863636363636,
0.0227272727272727,0.0255681818181818,0.0284090909090909,0.03125,0.0340909090909091,
0.0369318181818182,0.0397727272727273,0.0426136363636364,0.0454545454545455,
0.0482954545454545,0.0511363636363636,0.0539772727272727,0.0568181818181818,
0.0596590909090909,0.0625,0.0653409090909091,0.0681818181818182,0.0710227272727273,
0.0738636363636364,0.0767045454545455,0.0795454545454545,0.0823863636363636,
0.0852272727272727,0.0880681818181818,0.0909090909090909,0.09375,0.0965909090909091,
0.0994318181818182,0.102272727272727,0.105113636363636,0.107954545454545,
0.110795454545455,0.113636363636364,0.116477272727273,0.119318181818182,
0.122159090909091,0.125,0.127840909090909,0.130681818181818,0.133522727272727,
0.136363636363636,0.139204545454545,0.142045454545455,0.144886363636364,
0.147727272727273,0.150568181818182,0.153409090909091,0.15625,0.159090909090909,
0.161931818181818,0.164772727272727,0.167613636363636,0.170454545454545,
0.173295454545455,0.176136363636364,0.178977272727273,0.181818181818182,
0.184659090909091,0.1875,0.190340909090909,0.193181818181818,0.196022727272727,
0.198863636363636,0.201704545454545,0.204545454545455,0.207386363636364,
0.210227272727273,0.213068181818182,0.215909090909091,0.21875,0.221590909090909,
0.224431818181818,0.227272727272727,0.230113636363636,0.232954545454545,
0.235795454545455,0.238636363636364,0.241477272727273,0.244318181818182,
0.247159090909091,0.25,0.252840909090909,0.255681818181818,0.258522727272727,
0.261363636363636,0.264204545454545,0.267045454545455,0.269886363636364,
0.272727272727273,0.275568181818182,0.278409090909091,0.28125,0.284090909090909,
0.286931818181818,0.289772727272727,0.292613636363636,0.295454545454545,
0.298295454545455,0.301136363636364,0.303977272727273,0.306818181818182,
0.309659090909091,0.3125,0.315340909090909,0.318181818181818,0.321022727272727,
0.323863636363636,0.326704545454545,0.329545454545455,0.332386363636364,
0.335227272727273,0.338068181818182,0.340909090909091,0.34375,0.346590909090909,
0.349431818181818,0.352272727272727,0.355113636363636,0.357954545454545,
0.360795454545455,0.363636363636364,0.366477272727273,0.369318181818182,
0.372159090909091,0.375,0.377840909090909,0.380681818181818,0.383522727272727,
0.386363636363636,0.389204545454546,0.392045454545455,0.394886363636364,
0.397727272727273,0.400568181818182,0.403409090909091,0.40625,0.409090909090909,
0.411931818181818,0.414772727272727,0.417613636363636,0.420454545454545,
0.423295454545455,0.426136363636364,0.428977272727273,0.431818181818182,
0.434659090909091,0.4375,0.440340909090909,0.443181818181818,0.446022727272727,
0.448863636363636,0.451704545454545,0.454545454545455,0.457386363636364,
0.460227272727273,0.463068181818182,0.465909090909091,0.46875,0.471590909090909,
0.474431818181818,0.477272727272727,0.480113636363636,0.482954545454545,
0.485795454545455,0.488636363636364,0.491477272727273,0.494318181818182,
0.497159090909091,0.5,0.502840909090909,0.505681818181818,0.508522727272727,
0.511363636363636,0.514204545454545,0.517045454545455,0.519886363636364,
0.522727272727273,0.525568181818182,0.528409090909091,0.53125,0.534090909090909,
0.536931818181818,0.539772727272727,0.542613636363636,0.545454545454545,
0.548295454545455,0.551136363636364,0.553977272727273,0.556818181818182,
0.559659090909091,0.5625,0.565340909090909,0.568181818181818,0.571022727272727,
0.573863636363636,0.576704545454545,0.579545454545455,0.582386363636364,
0.585227272727273,0.588068181818182,0.590909090909091,0.59375,0.596590909090909,
0.599431818181818,0.602272727272727,0.605113636363636,0.607954545454545,
0.610795454545455,0.613636363636364,0.616477272727273,0.619318181818182,
0.622159090909091,0.625,0.627840909090909,0.630681818181818,0.633522727272727,
0.636363636363636,0.639204545454545,0.642045454545455,0.644886363636364,
0.647727272727273,0.650568181818182,0.653409090909091,0.65625,0.659090909090909,
0.661931818181818,0.664772727272727,0.667613636363636,0.670454545454546,
0.673295454545455,0.676136363636364,0.678977272727273,0.681818181818182,
0.684659090909091,0.6875,0.690340909090909,0.693181818181818,0.696022727272727,
0.698863636363636,0.701704545454545,0.704545454545455,0.707386363636364,
0.710227272727273,0.713068181818182,0.715909090909091,0.71875,0.721590909090909,
0.724431818181818,0.727272727272727,0.730113636363636,0.732954545454545,
0.735795454545455,0.738636363636364,0.741477272727273,0.744318181818182,
0.747159090909091,0.75,0.752840909090909,0.755681818181818,0.758522727272727,
0.761363636363636,0.764204545454545,0.767045454545455,0.769886363636364,
0.772727272727273,0.775568181818182,0.778409090909091,0.78125,0.784090909090909,
0.786931818181818,0.789772727272727,0.792613636363636,0.795454545454545,
0.798295454545455,0.801136363636364,0.803977272727273,0.806818181818182,
0.809659090909091,0.8125,0.815340909090909,0.818181818181818,0.821022727272727,
0.823863636363636,0.826704545454546,0.829545454545455,0.832386363636364,
0.835227272727273,0.838068181818182,0.840909090909091,0.84375,0.846590909090909,
0.849431818181818,0.852272727272727,0.855113636363636,0.857954545454545,
0.860795454545455,0.863636363636364,0.866477272727273,0.869318181818182,
0.872159090909091,0.875,0.877840909090909,0.880681818181818,0.883522727272727,
0.886363636363636,0.889204545454545,0.892045454545455,0.894886363636364,
0.897727272727273,0.900568181818182,0.903409090909091,0.90625,0.909090909090909,
0.911931818181818,0.913809604147033),.UNSPECIFIED.)
CURVE()
GEOMETRIC_REPRESENTATION_ITEM()
RATIONAL_B_SPLINE_CURVE((0.965885055496846,0.974193689329879,1.,0.923879532511287,
1.,0.923879532511287,1.,0.923879532511287,1.,0.923879532511287,1.,0.923879532511287,
1.,0.923879532511287,1.,0.923879532511287,1.,0.923879532511287,1.,0.923879532511287,
1.,0.923879532511287,1.,0.923879532511287,1.,0.923879532511287,1.,0.923879532511287,
1.,0.923879532511287,1.,0.923879532511287,1.,0.923879532511287,1.,0.923879532511287,
1.,0.923879532511287,1.,0.923879532511287,1.,0.923879532511287,1.,0.923879532511287,
1.,0.923879532511287,1.,0.923879532511287,1.,0.923879532511287,1.,0.923879532511287,
1.,0.923879532511287,1.,0.923879532511287,1.,0.923879532511287,1.,0.923879532511287,
1.,0.923879532511287,1.,0.923879532511287,1.,0.923879532511287,1.,0.923879532511287,
1.,0.923879532511287,1.,0.923879532511287,1.,0.923879532511287,1.,0.923879532511287,
1.,0.923879532511287,1.,0.923879532511287,1.,0.923879532511287,1.,0.923879532511287,
1.,0.923879532511287,1.,0.923879532511287,1.,0.923879532511287,1.,0.923879532511287,
1.,0.923879532511287,1.,0.923879532511287,1.,0.923879532511287,1.,0.923879532511287,
1.,0.923879532511287,1.,0.923879532511287,1.,0.923879532511287,1.,0.923879532511287,
1.,0.923879532511287,1.,0.923879532511287,1.,0.923879532511287,1.,0.923879532511287,
1.,0.923879532511287,1.,0.923879532511287,1.,0.923879532511287,1.,0.923879532511287,
1.,0.923879532511287,1.,0.923879532511287,1.,0.923879532511287,1.,0.923879532511287,
1.,0.923879532511287,1.,0.923879532511287,1.,0.923879532511287,1.,0.923879532511287,
1.,0.923879532511287,1.,0.923879532511287,1.,0.923879532511287,1.,0.923879532511287,
1.,0.923879532511287,1.,0.923879532511287,1.,0.923879532511287,1.,0.923879532511287,
1.,0.923879532511287,1.,0.923879532511287,1.,0.923879532511287,1.,0.923879532511287,
1.,0.923879532511287,1.,0.923879532511287,1.,0.923879532511287,1.,0.923879532511287,
1.,0.923879532511287,1.,0.923879532511287,1.,0.923879532511287,1.,0.923879532511287,
1.,0.923879532511287,1.,0.923879532511287,1.,0.923879532511287,1.,0.923879532511287,
1.,0.923879532511287,1.,0.923879532511287,1.,0.923879532511287,1.,0.923879532511287,
1.,0.923879532511287,1.,0.923879532511287,1.,0.923879532511287,1.,0.923879532511287,
1.,0.923879532511287,1.,0.923879532511287,1.,0.923879532511287,1.,0.923879532511287,
1.,0.923879532511287,1.,0.923879532511287,1.,0.923879532511287,1.,0.923879532511287,
1.,0.923879532511287,1.,0.923879532511287,1.,0.923879532511287,1.,0.923879532511287,
1.,0.923879532511287,1.,0.923879532511287,1.,0.923879532511287,1.,0.923879532511287,
1.,0.923879532511287,1.,0.923879532511287,1.,0.923879532511287,1.,0.923879532511287,
1.,0.923879532511287,1.,0.923879532511287,1.,0.923879532511287,1.,0.923879532511287,
1.,0.923879532511287,1.,0.923879532511287,1.,0.923879532511287,1.,0.923879532511287,
1.,0.923879532511287,1.,0.923879532511287,1.,0.923879532511287,1.,0.923879532511287,
1.,0.923879532511287,1.,0.923879532511287,1.,0.923879532511287,1.,0.923879532511287,
1.,0.923879532511287,1.,0.923879532511287,1.,0.923879532511287,1.,0.923879532511287,
1.,0.923879532511287,1.,0.923879532511287,1.,0.923879532511287,1.,0.923879532511287,
1.,0.923879532511287,1.,0.923879532511287,1.,0.923879532511287,1.,0.923879532511287,
1.,0.923879532511287,1.,0.923879532511287,1.,0.923879532511287,1.,0.923879532511287,
1.,0.923879532511287,1.,0.923879532511287,1.,0.923879532511287,1.,0.923879532511287,
1.,0.923879532511287,1.,0.923879532511287,1.,0.923879532511287,1.,0.923879532511287,
1.,0.923879532511287,1.,0.923879532511287,1.,0.923879532511287,1.,0.923879532511287,
1.,0.923879532511287,1.,0.923879532511287,1.,0.923879532511287,1.,0.923879532511287,
1.,0.923879532511287,1.,0.923879532511287,1.,0.923879532511287,1.,0.923879532511287,
1.,0.923879532511287,1.,0.923879532511287,1.,0.923879532511287,1.,0.923879532511287,
1.,0.923879532511287,1.,0.923879532511287,1.,0.923879532511287,1.,0.923879532511287,
1.,0.923879532511287,1.,0.923879532511287,1.,0.923879532511287,1.,0.923879532511287,
1.,0.923879532511287,1.,0.923879532511287,1.,0.923879532511287,1.,0.923879532511287,
1.,0.923879532511287,1.,0.923879532511287,1.,0.923879532511287,1.,0.923879532511287,
1.,0.923879532511287,1.,0.923879532511287,1.,0.923879532511287,1.,0.923879532511287,
1.,0.923879532511287,1.,0.923879532511287,1.,0.923879532511287,1.,0.923879532511287,
1.,0.923879532511287,1.,0.923879532511287,1.,0.923879532511287,1.,0.923879532511287,
1.,0.923879532511287,1.,0.923879532511287,1.,0.923879532511287,1.,0.923879532511287,
1.,0.923879532511287,1.,0.923879532511287,1.,0.923879532511287,1.,0.923879532511287,
1.,0.923879532511287,1.,0.923879532511287,1.,0.923879532511287,1.,0.923879532511287,
1.,0.923879532511287,1.,0.923879532511287,1.,0.923879532511287,1.,0.923879532511287,
1.,0.923879532511287,1.,0.923879532511287,1.,0.923879532511287,1.,0.923879532511287,
1.,0.923879532511287,1.,0.923879532511287,1.,0.923879532511287,1.,0.923879532511287,
1.,0.923879532511287,1.,0.923879532511287,1.,0.923879532511287,1.,0.923879532511287,
1.,0.923879532511287,1.,0.923879532511287,1.,0.923879532511287,1.,0.923879532511287,
1.,0.923879532511287,1.,0.923879532511287,1.,0.923879532511287,1.,0.923879532511287,
1.,0.923879532511287,1.,0.923879532511287,1.,0.923879532511287,1.,0.923879532511287,
1.,0.923879532511287,1.,0.923879532511287,1.,0.923879532511287,1.,0.923879532511287,
1.,0.923879532511287,1.,0.923879532511287,1.,0.923879532511287,1.,0.923879532511287,
1.,0.923879532511287,1.,0.923879532511287,1.,0.923879532511287,1.,0.923879532511287,
1.,0.923879532511287,1.,0.923879532511287,1.,0.923879532511287,1.,0.923879532511287,
1.,0.923879532511287,1.,0.923879532511287,1.,0.923879532511287,1.,0.923879532511287,
1.,0.923879532511287,1.,0.923879532511287,1.,0.923879532511287,1.,0.923879532511287,
1.,0.923879532511287,1.,0.923879532511287,1.,0.923879532511287,1.,0.923879532511287,
1.,0.923879532511287,1.,0.923879532511287,1.,0.923879532511287,1.,0.923879532511287,
1.,0.923879532511287,1.,0.923879532511287,1.,0.923879532511287,1.,0.923879532511287,
1.,0.923879532511287,1.,0.923879532511287,1.,0.923879532511287,1.,0.923879532511287,
1.,0.923879532511287,1.,0.923879532511287,1.,0.923879532511287,1.,0.923879532511287,
1.,0.923879532511287,1.,0.923879532511287,1.,0.923879532511287,1.,0.923879532511287,
1.,0.923879532511287,1.,0.923879532511287,1.,0.923879532511287,1.,0.923879532511287,
1.,0.923879532511287,1.,0.923879532511287,1.,0.923879532511287,1.,0.923879532511287,
1.,0.923879532511287,1.,0.923879532511287,1.,0.923879532511287,1.,0.923879532511287,
1.,0.923879532511287,1.,0.923879532511287,1.,0.923879532511287,1.,0.923879532511287,
1.,0.923879532511287,1.,0.923879532511287,1.,0.923879532511287,1.,0.923879532511287,
1.,0.923879532511287,1.,0.923879532511287,1.,0.923879532511287,1.,0.923879532511287,
1.,0.923879532511287,1.,0.923879532511287,1.,0.949685843178392,0.965885055498788))
REPRESENTATION_ITEM('')
);
#90=ELLIPSE('',#9174,3.18617762455186,3.07129968234925);
#91=ELLIPSE('',#9175,3.18617761845016,3.07129967669361);
#92=ELLIPSE('',#9176,3.18617759547738,3.07129965523857);
#93=ELLIPSE('',#9177,3.18617760733856,3.07129966633831);
#94=ELLIPSE('',#9178,3.18617760230713,3.07129966147478);
#95=ELLIPSE('',#9179,3.18617759636938,3.07129965601913);
#96=ELLIPSE('',#9180,3.18617760025713,3.07129965960386);
#97=ELLIPSE('',#9183,3.18617762276224,3.07129968128518);
#98=ELLIPSE('',#9184,3.18617761431604,3.07129967288479);
#99=ELLIPSE('',#9226,3.15483183585312,3.04022344912707);
#100=ELLIPSE('',#9227,3.15483182592464,3.04022343859094);
#101=ELLIPSE('',#9228,3.15483183621962,3.04022344977534);
#102=ELLIPSE('',#9229,3.53219078069322,3.28486872276377);
#103=ELLIPSE('',#9230,3.15483183030471,3.04022344355871);
#104=ELLIPSE('',#9231,3.15483182288516,3.04022343561688);
#105=ELLIPSE('',#9232,3.15483181972163,3.04022343210884);
#106=ELLIPSE('',#9233,3.1548318236625,3.04022343652648);
#107=ELLIPSE('',#9234,3.15483184138826,3.04022345552491);
#108=ELLIPSE('',#9235,3.15483182239517,3.04022343496998);
#109=ELLIPSE('',#9281,18.0380987508663,8.93352299302603);
#110=ELLIPSE('',#9284,18.0200745312909,8.92797473607996);
#111=ELLIPSE('',#9597,55.9999994580806,27.9999998645779);
#112=ELLIPSE('',#9600,56.0000011433114,28.0000002857322);
#113=ELLIPSE('',#9746,4.06396121899487,1.49999999996976);
#114=ELLIPSE('',#9760,4.06396121989312,1.50000000014194);
#115=ELLIPSE('',#9762,4.71890632484228,1.50000000000588);
#116=ELLIPSE('',#9763,5.29011801808111,1.49999999999909);
#117=ELLIPSE('',#9769,4.71890632482846,1.5000000000021);
#118=ELLIPSE('',#9770,5.29011801808671,1.49999999999996);
#119=ELLIPSE('',#9772,5.36487494985319,2.99999999998019);
#120=ELLIPSE('',#9773,5.36487494986476,2.99999999998425);
#121=ELLIPSE('',#9861,992.32273705942,143.940737429079);
#122=ELLIPSE('',#9863,1.41421356237156,0.999999999998736);
#123=ELLIPSE('',#9865,1.41421356237466,1.00000000000111);
#124=B_SPLINE_SURFACE_WITH_KNOTS('',3,1,((#16524,#16525),(#16526,#16527),
(#16528,#16529),(#16530,#16531)),.UNSPECIFIED.,.F.,.F.,.F.,(4,4),(2,2),
(0.,1.),(0.,0.239999999999999),.UNSPECIFIED.);
#125=B_SPLINE_SURFACE_WITH_KNOTS('',3,1,((#16618,#16619),(#16620,#16621),
(#16622,#16623),(#16624,#16625)),.UNSPECIFIED.,.F.,.F.,.F.,(4,4),(2,2),
(0.,1.),(0.,0.239999999999999),.UNSPECIFIED.);
#126=B_SPLINE_SURFACE_WITH_KNOTS('',3,1,((#16715,#16716),(#16717,#16718),
(#16719,#16720),(#16721,#16722)),.UNSPECIFIED.,.F.,.F.,.F.,(4,4),(2,2),
(0.,1.),(0.,0.239999999999999),.UNSPECIFIED.);
#127=B_SPLINE_SURFACE_WITH_KNOTS('',3,1,((#16803,#16804),(#16805,#16806),
(#16807,#16808),(#16809,#16810)),.UNSPECIFIED.,.F.,.F.,.F.,(4,4),(2,2),
(0.,1.),(0.,0.239999999999999),.UNSPECIFIED.);
#128=B_SPLINE_SURFACE_WITH_KNOTS('',3,1,((#16894,#16895),(#16896,#16897),
(#16898,#16899),(#16900,#16901)),.UNSPECIFIED.,.F.,.F.,.F.,(4,4),(2,2),
(0.,1.),(0.,0.240000000000008),.UNSPECIFIED.);
#129=B_SPLINE_SURFACE_WITH_KNOTS('',3,1,((#16985,#16986),(#16987,#16988),
(#16989,#16990),(#16991,#16992)),.UNSPECIFIED.,.F.,.F.,.F.,(4,4),(2,2),
(0.,1.),(0.,0.239999999999999),.UNSPECIFIED.);
#130=B_SPLINE_SURFACE_WITH_KNOTS('',3,1,((#17924,#17925),(#17926,#17927),
(#17928,#17929),(#17930,#17931),(#17932,#17933),(#17934,#17935),(#17936,
#17937),(#17938,#17939),(#17940,#17941),(#17942,#17943),(#17944,#17945),
(#17946,#17947)),.UNSPECIFIED.,.F.,.F.,.F.,(4,2,2,2,2,4),(2,2),(0.,0.25,
0.5,0.625,0.75,1.),(0.,0.240000000000451),.UNSPECIFIED.);
#131=B_SPLINE_SURFACE_WITH_KNOTS('',3,1,((#18513,#18514),(#18515,#18516),
(#18517,#18518),(#18519,#18520)),.UNSPECIFIED.,.F.,.F.,.F.,(4,4),(2,2),
(0.,0.994738905317126),(0.,0.239999999999999),.UNSPECIFIED.);
#132=B_SPLINE_SURFACE_WITH_KNOTS('',3,1,((#19117,#19118),(#19119,#19120),
(#19121,#19122),(#19123,#19124)),.UNSPECIFIED.,.F.,.F.,.F.,(4,4),(2,2),
(0.,1.),(0.,1.),.UNSPECIFIED.);
#133=B_SPLINE_SURFACE_WITH_KNOTS('',3,1,((#46101,#46102),(#46103,#46104),
(#46105,#46106),(#46107,#46108),(#46109,#46110),(#46111,#46112)),
 .UNSPECIFIED.,.F.,.F.,.F.,(4,1,1,4),(2,2),(0.0598879849550618,0.738151675687099,
0.838151675687099,1.),(0.,0.118332698778717),.UNSPECIFIED.);
#134=B_SPLINE_SURFACE_WITH_KNOTS('',3,1,((#46331,#46332),(#46333,#46334),
(#46335,#46336),(#46337,#46338)),.UNSPECIFIED.,.F.,.F.,.F.,(4,4),(2,2),
(0.,0.99999999993505),(0.,0.384000000000005),.UNSPECIFIED.);
#135=B_SPLINE_SURFACE_WITH_KNOTS('',3,1,((#46385,#46386),(#46387,#46388),
(#46389,#46390),(#46391,#46392),(#46393,#46394),(#46395,#46396)),
 .UNSPECIFIED.,.F.,.F.,.F.,(4,1,1,4),(2,2),(0.0598879849550605,0.738151675687099,
0.838151675687099,1.),(0.,0.118332698778627),.UNSPECIFIED.);
#136=B_SPLINE_SURFACE_WITH_KNOTS('',3,1,((#46513,#46514),(#46515,#46516),
(#46517,#46518),(#46519,#46520),(#46521,#46522),(#46523,#46524),(#46525,
#46526),(#46527,#46528),(#46529,#46530),(#46531,#46532),(#46533,#46534),
(#46535,#46536),(#46537,#46538),(#46539,#46540),(#46541,#46542),(#46543,
#46544),(#46545,#46546),(#46547,#46548),(#46549,#46550),(#46551,#46552),
(#46553,#46554),(#46555,#46556)),.UNSPECIFIED.,.F.,.F.,.F.,(4,2,1,1,2,2,
2,2,2,2,2,4),(2,2),(0.,0.00781250000000001,0.015625,0.03125,0.0624999999999999,
0.125,0.25,0.5,0.749999999999999,0.874999999999999,0.9375,1.),(0.,0.412896000000006),
 .UNSPECIFIED.);
#137=CONICAL_SURFACE('',#9144,5.,0.5235987755983);
#138=CONICAL_SURFACE('',#9146,5.,0.5235987755983);
#139=CONICAL_SURFACE('',#9256,10.,0.5235987755983);
#140=CONICAL_SURFACE('',#9258,10.,0.5235987755983);
#141=CONICAL_SURFACE('',#9390,2.99999999999999,0.78539816339745);
#142=CONICAL_SURFACE('',#9608,105.,0.5235987755983);
#143=CONICAL_SURFACE('',#9610,13.5459216391339,0.5235987755983);
#144=CONICAL_SURFACE('',#9612,5.,0.5235987755983);
#145=CONICAL_SURFACE('',#9615,5.,0.5235987755983);
#146=CONICAL_SURFACE('',#9620,13.5459216391339,0.5235987755983);
#147=CONICAL_SURFACE('',#9622,105.,0.5235987755983);
#148=B_SPLINE_CURVE_WITH_KNOTS('',3,(#12437,#12438,#12439,#12440,#12441,
#12442,#12443,#12444,#12445,#12446,#12447,#12448,#12449,#12450,#12451,#12452,
#12453,#12454,#12455,#12456,#12457,#12458,#12459,#12460),.UNSPECIFIED.,
 .F.,.F.,(4,2,2,2,2,2,2,2,2,2,2,4),(0.916063809045508,0.917441355582055,
0.918818902118601,0.921573995191693,0.924329088264786,0.925706634801332,
0.927084181337879,0.932594367484064,0.935349460557156,0.936727007093702,
0.937415780361976,0.938104553630249),.UNSPECIFIED.);
#149=B_SPLINE_CURVE_WITH_KNOTS('',3,(#12461,#12462,#12463,#12464,#12465,
#12466,#12467,#12468,#12469,#12470,#12471,#12472,#12473,#12474,#12475,#12476,
#12477,#12478,#12479,#12480,#12481,#12482,#12483,#12484),.UNSPECIFIED.,
 .F.,.F.,(4,2,2,2,2,2,2,2,2,2,2,4),(0.916063809045508,0.917441355582055,
0.918818902118601,0.921573995191693,0.924329088264786,0.925706634801332,
0.927084181337879,0.932594367484064,0.935349460557156,0.936727007093702,
0.937415780361976,0.938104553630249),.UNSPECIFIED.);
#150=B_SPLINE_CURVE_WITH_KNOTS('',3,(#13664,#13665,#13666,#13667,#13668,
#13669,#13670,#13671,#13672,#13673,#13674,#13675,#13676,#13677,#13678,#13679,
#13680,#13681,#13682,#13683,#13684,#13685,#13686,#13687,#13688,#13689,#13690,
#13691,#13692,#13693,#13694,#13695,#13696,#13697,#13698,#13699,#13700,#13701,
#13702,#13703,#13704,#13705,#13706,#13707,#13708,#13709,#13710,#13711,#13712,
#13713,#13714,#13715,#13716,#13717,#13718,#13719,#13720,#13721,#13722,#13723,
#13724,#13725,#13726,#13727,#13728,#13729,#13730,#13731,#13732,#13733,#13734,
#13735,#13736,#13737,#13738,#13739,#13740,#13741,#13742,#13743,#13744,#13745,
#13746,#13747,#13748,#13749,#13750,#13751,#13752,#13753,#13754,#13755,#13756,
#13757,#13758,#13759,#13760,#13761,#13762,#13763,#13764,#13765,#13766,#13767,
#13768,#13769,#13770,#13771,#13772,#13773,#13774,#13775,#13776,#13777,#13778,
#13779,#13780,#13781,#13782,#13783,#13784,#13785,#13786,#13787,#13788,#13789,
#13790,#13791,#13792,#13793,#13794,#13795,#13796,#13797,#13798,#13799,#13800,
#13801,#13802,#13803,#13804,#13805,#13806,#13807,#13808,#13809,#13810,#13811,
#13812,#13813,#13814,#13815,#13816,#13817,#13818,#13819,#13820,#13821,#13822,
#13823,#13824,#13825,#13826,#13827,#13828,#13829,#13830,#13831),
 .UNSPECIFIED.,.F.,.F.,(4,2,2,2,2,2,2,2,2,2,2,2,2,2,2,2,2,2,2,2,2,2,2,2,
2,2,2,2,2,2,2,2,2,2,2,2,2,2,2,2,2,2,2,2,2,2,2,2,2,2,2,2,2,2,2,2,2,2,2,2,
2,2,2,2,2,2,2,2,2,2,2,2,2,2,2,2,2,2,2,2,2,2,2,4),(0.0896131586159842,0.0909349273058256,
0.092256695995667,0.09490023337535,0.100187308134716,0.110761457653447,
0.121335607172179,0.131909756690911,0.142406945548381,0.152904134405852,
0.163401323263323,0.173898512120793,0.184326267064866,0.194754022008939,
0.205181776953011,0.215609531897084,0.225968774255778,0.236328016614473,
0.246687258973167,0.257046501331861,0.268365392558388,0.279684283784914,
0.29100317501144,0.302322066237966,0.313563979866736,0.324805893495506,
0.336047807124276,0.347289720753047,0.358457560536344,0.369625400319641,
0.380793240102939,0.391961079886236,0.403057648451734,0.414154217017233,
0.425250785582731,0.43634735414823,0.447375242283774,0.458403130419317,
0.469431018554861,0.480458906690405,0.491420626849432,0.50238234700846,
0.513344067167488,0.524305787326516,0.535203741266554,0.546101695206592,
0.55699964914663,0.567897603086667,0.578734005374906,0.589570407663145,
0.600406809951383,0.611243212239622,0.62202044333232,0.632797674425018,
0.643574905517716,0.654352136610414,0.665072195325672,0.675792254040929,
0.686512312756186,0.697232371471444,0.707897173370898,0.718561975270352,
0.729226777169807,0.739891579069261,0.750503305564763,0.761115032060264,
0.771726758555766,0.782338485051268,0.79289871583597,0.803458946620673,
0.814019177405375,0.824579408190078,0.835090233536042,0.845601058882007,
0.856111884227971,0.866622709573936,0.877085607262584,0.887548504951232,
0.89801140263988,0.908474300328528,0.912269054687018,0.914166431866263,
0.915115120455886,0.916063809045508),.UNSPECIFIED.);
#151=B_SPLINE_CURVE_WITH_KNOTS('',3,(#13832,#13833,#13834,#13835,#13836,
#13837,#13838,#13839,#13840,#13841,#13842,#13843,#13844,#13845,#13846,#13847,
#13848,#13849,#13850,#13851,#13852,#13853,#13854,#13855,#13856,#13857,#13858,
#13859,#13860,#13861,#13862,#13863,#13864,#13865,#13866,#13867,#13868,#13869,
#13870,#13871,#13872,#13873,#13874,#13875,#13876,#13877,#13878,#13879,#13880,
#13881,#13882,#13883,#13884,#13885,#13886,#13887,#13888,#13889,#13890,#13891,
#13892,#13893,#13894,#13895,#13896,#13897,#13898,#13899,#13900,#13901,#13902,
#13903,#13904,#13905,#13906,#13907,#13908,#13909,#13910,#13911,#13912,#13913,
#13914,#13915,#13916,#13917,#13918,#13919,#13920,#13921,#13922,#13923,#13924,
#13925,#13926,#13927,#13928,#13929,#13930,#13931,#13932,#13933,#13934,#13935,
#13936,#13937,#13938,#13939,#13940,#13941,#13942,#13943,#13944,#13945,#13946,
#13947,#13948,#13949,#13950,#13951,#13952,#13953,#13954,#13955,#13956,#13957,
#13958,#13959,#13960,#13961,#13962,#13963,#13964,#13965,#13966,#13967,#13968,
#13969,#13970,#13971,#13972,#13973,#13974,#13975,#13976,#13977,#13978,#13979,
#13980,#13981,#13982,#13983,#13984,#13985,#13986,#13987,#13988,#13989,#13990,
#13991,#13992,#13993,#13994,#13995,#13996,#13997,#13998,#13999),
 .UNSPECIFIED.,.F.,.F.,(4,2,2,2,2,2,2,2,2,2,2,2,2,2,2,2,2,2,2,2,2,2,2,2,
2,2,2,2,2,2,2,2,2,2,2,2,2,2,2,2,2,2,2,2,2,2,2,2,2,2,2,2,2,2,2,2,2,2,2,2,
2,2,2,2,2,2,2,2,2,2,2,2,2,2,2,2,2,2,2,2,2,2,2,4),(0.0896131586159842,0.0909349273058256,
0.092256695995667,0.09490023337535,0.100187308134716,0.110761457653447,
0.121335607172179,0.131909756690911,0.142406945548381,0.152904134405852,
0.163401323263323,0.173898512120793,0.184326267064866,0.194754022008939,
0.205181776953011,0.215609531897084,0.225968774255778,0.236328016614473,
0.246687258973167,0.257046501331861,0.268365392558388,0.279684283784914,
0.29100317501144,0.302322066237966,0.313563979866736,0.324805893495506,
0.336047807124276,0.347289720753047,0.358457560536344,0.369625400319641,
0.380793240102939,0.391961079886236,0.403057648451734,0.414154217017233,
0.425250785582731,0.43634735414823,0.447375242283774,0.458403130419317,
0.469431018554861,0.480458906690405,0.491420626849432,0.50238234700846,
0.513344067167488,0.524305787326516,0.535203741266554,0.546101695206592,
0.55699964914663,0.567897603086667,0.578734005374906,0.589570407663145,
0.600406809951383,0.611243212239622,0.62202044333232,0.632797674425018,
0.643574905517716,0.654352136610414,0.665072195325672,0.675792254040929,
0.686512312756186,0.697232371471444,0.707897173370898,0.718561975270352,
0.729226777169807,0.739891579069261,0.750503305564763,0.761115032060264,
0.771726758555766,0.782338485051268,0.79289871583597,0.803458946620673,
0.814019177405375,0.824579408190078,0.835090233536042,0.845601058882007,
0.856111884227971,0.866622709573936,0.877085607262584,0.887548504951232,
0.89801140263988,0.908474300328528,0.912269054687018,0.914166431866263,
0.915115120455886,0.916063809045508),.UNSPECIFIED.);
#152=B_SPLINE_CURVE_WITH_KNOTS('',3,(#14143,#14144,#14145,#14146,#14147,
#14148,#14149,#14150,#14151,#14152,#14153,#14154,#14155,#14156,#14157,#14158,
#14159,#14160,#14161,#14162),.UNSPECIFIED.,.F.,.F.,(4,2,2,2,2,2,2,2,2,4),
(0.0618954463697512,0.0653601604005303,0.0688248744313094,0.0757543024928677,
0.0792190165236468,0.0809513735390363,0.0826837305544259,0.086148444585205,
0.0878808016005946,0.0896131586159842),.UNSPECIFIED.);
#153=B_SPLINE_CURVE_WITH_KNOTS('',3,(#14163,#14164,#14165,#14166,#14167,
#14168,#14169,#14170,#14171,#14172,#14173,#14174,#14175,#14176,#14177,#14178,
#14179,#14180,#14181,#14182),.UNSPECIFIED.,.F.,.F.,(4,2,2,2,2,2,2,2,2,4),
(0.0618954463697512,0.0653601604005303,0.0688248744313094,0.0757543024928677,
0.0792190165236468,0.0809513735390363,0.0826837305544259,0.086148444585205,
0.0878808016005946,0.0896131586159842),.UNSPECIFIED.);
#154=B_SPLINE_CURVE_WITH_KNOTS('',3,(#15707,#15708,#15709,#15710,#15711,
#15712,#15713,#15714,#15715,#15716,#15717,#15718),.UNSPECIFIED.,.F.,.F.,
(4,2,2,2,2,4),(-0.315861705869912,-0.304504739480588,-0.293147577229122,
-0.273654264741298,-0.254199478143445,-0.237067099008455),.UNSPECIFIED.);
#155=B_SPLINE_CURVE_WITH_KNOTS('',3,(#15728,#15729,#15730,#15731,#15732,
#15733,#15734,#15735,#15736,#15737),.UNSPECIFIED.,.F.,.F.,(4,2,2,2,4),(-0.075918388998373,
-0.0561637881777793,-0.0369076925566084,-0.0182249521533977,0.),
 .UNSPECIFIED.);
#156=B_SPLINE_CURVE_WITH_KNOTS('',3,(#15746,#15747,#15748,#15749,#15750,
#15751,#15752,#15753,#15754,#15755),.UNSPECIFIED.,.F.,.F.,(4,2,2,2,4),(-0.303763540065855,
-0.285538587912457,-0.266855847509246,-0.247599751888075,-0.227845151067482),
 .UNSPECIFIED.);
#157=B_SPLINE_CURVE_WITH_KNOTS('',3,(#15761,#15762,#15763,#15764,#15765,
#15766,#15767,#15768,#15769,#15770,#15771,#15772,#15773,#15774,#15775,#15776,
#15777,#15778,#15779,#15780,#15781,#15782,#15783,#15784,#15785,#15786,#15787,
#15788,#15789,#15790,#15791),.UNSPECIFIED.,.F.,.F.,(4,3,3,3,3,3,3,3,3,3,
4),(0.,6.43812390587994E-5,0.000133462758091886,0.000205560683863588,0.000281692284478665,
0.000294258926984526,0.00030196027953542,0.000382573776850771,0.000466187556446014,
0.000551165178275843,0.000603920559070841),.UNSPECIFIED.);
#158=B_SPLINE_CURVE_WITH_KNOTS('',3,(#15800,#15801,#15802,#15803,#15804,
#15805,#15806,#15807,#15808,#15809,#15810,#15811,#15812,#15813,#15814,#15815,
#15816,#15817,#15818,#15819,#15820,#15821,#15822,#15823,#15824,#15825,#15826,
#15827,#15828,#15829,#15830),.UNSPECIFIED.,.F.,.F.,(4,3,3,3,3,3,3,3,3,3,
4),(0.,8.03828939616283E-5,0.00016094681871393,0.000237477837746124,0.000302706001391965,
0.000310398285264662,0.000384832659816502,0.000456089108430895,0.000524203185115278,
0.000588293662717843,0.00060541200278393),.UNSPECIFIED.);
#159=B_SPLINE_CURVE_WITH_KNOTS('',3,(#15838,#15839,#15840,#15841),
 .UNSPECIFIED.,.F.,.F.,(4,4),(0.000288679049704741,0.00173207592567418),
 .UNSPECIFIED.);
#160=B_SPLINE_CURVE_WITH_KNOTS('',3,(#15842,#15843,#15844,#15845),
 .UNSPECIFIED.,.F.,.F.,(4,4),(0.,0.00146452330146534),.UNSPECIFIED.);
#161=B_SPLINE_CURVE_WITH_KNOTS('',3,(#15850,#15851,#15852,#15853),
 .UNSPECIFIED.,.F.,.F.,(4,4),(3.99819120664141E-10,0.0014645237012841),
 .UNSPECIFIED.);
#162=B_SPLINE_CURVE_WITH_KNOTS('',3,(#15854,#15855,#15856,#15857),
 .UNSPECIFIED.,.F.,.F.,(4,4),(0.,0.00144339687596949),.UNSPECIFIED.);
#163=B_SPLINE_CURVE_WITH_KNOTS('',3,(#15874,#15875,#15876,#15877,#15878,
#15879,#15880,#15881),.UNSPECIFIED.,.F.,.F.,(4,2,2,4),(0.,0.0195287994608885,
0.039060798714645,0.058407685727557),.UNSPECIFIED.);
#164=B_SPLINE_CURVE_WITH_KNOTS('',3,(#15893,#15894,#15895,#15896,#15897,
#15898,#15899,#15900,#15901,#15902),.UNSPECIFIED.,.F.,.F.,(4,2,2,2,4),(0.25677760841793,
0.273427822422786,0.292959602080408,0.30405126303756,0.315142780478787),
 .UNSPECIFIED.);
#165=B_SPLINE_CURVE_WITH_KNOTS('',3,(#15909,#15910,#15911,#15912,#15913,
#15914,#15915,#15916,#15917,#15918,#15919,#15920),.UNSPECIFIED.,.F.,.F.,
(4,2,2,2,2,4),(-0.675172633386201,-0.576849455741665,-0.476321267640776,
-0.315506903735809,-0.160746606147669,-9.99999996698087E-7),
 .UNSPECIFIED.);
#166=B_SPLINE_CURVE_WITH_KNOTS('',3,(#15924,#15925,#15926,#15927,#15928,
#15929,#15930,#15931,#15932,#15933,#15934,#15935),.UNSPECIFIED.,.F.,.F.,
(4,2,2,2,2,4),(-0.675693768666456,-0.514824382991667,-0.359943941875025,
-0.199004734580793,-0.0983990080529495,0.),.UNSPECIFIED.);
#167=B_SPLINE_CURVE_WITH_KNOTS('',3,(#15943,#15944,#15945,#15946,#15947,
#15948,#15949,#15950,#15951,#15952,#15953,#15954,#15955,#15956,#15957,#15958,
#15959,#15960,#15961,#15962,#15963,#15964,#15965,#15966,#15967,#15968,#15969,
#15970,#15971,#15972,#15973,#15974,#15975,#15976,#15977,#15978,#15979,#15980,
#15981,#15982,#15983,#15984,#15985,#15986,#15987,#15988,#15989,#15990,#15991,
#15992,#15993,#15994,#15995,#15996,#15997,#15998,#15999,#16000,#16001,#16002,
#16003,#16004,#16005,#16006,#16007,#16008,#16009,#16010,#16011,#16012,#16013,
#16014,#16015,#16016,#16017,#16018,#16019,#16020,#16021,#16022,#16023,#16024,
#16025,#16026,#16027,#16028,#16029,#16030,#16031,#16032,#16033,#16034,#16035,
#16036,#16037,#16038,#16039,#16040,#16041,#16042,#16043,#16044,#16045,#16046,
#16047,#16048,#16049,#16050,#16051,#16052,#16053,#16054,#16055,#16056,#16057,
#16058,#16059,#16060,#16061,#16062,#16063,#16064,#16065,#16066,#16067,#16068,
#16069,#16070,#16071,#16072,#16073,#16074,#16075,#16076,#16077,#16078,#16079,
#16080,#16081),.UNSPECIFIED.,.F.,.F.,(4,3,3,3,3,3,3,3,3,3,3,3,3,3,3,3,3,
3,3,3,3,3,3,3,3,3,3,3,3,3,3,3,3,3,3,3,3,3,3,3,3,3,3,3,3,3,4),(0.,0.000256348549033948,
0.000502816100424785,0.000732686647454628,0.000929586010325689,0.00106762170514576,
0.00119927302827119,0.00132084179949912,0.00139437901548853,0.00146772785131755,
0.00153687262127654,0.00160013903578677,0.00162677551806997,0.00169883608742252,
0.00174297376936069,0.0017904732714029,0.00184301110341694,0.00185917202065141,
0.00192000576784545,0.00198442832044501,0.00205463066127626,0.00209156852323289,
0.00219804885243176,0.00231204074056505,0.00232396502581438,0.00249108586559547,
0.00266994389318095,0.00278875803097735,0.00305416840235674,0.00333025398384524,
0.00362172008319921,0.00371834404130334,0.00415146712302494,0.00461037575263192,
0.00509524559958469,0.00557751606195529,0.00625060925148138,0.00695696807124114,
0.00743668808260725,0.00838353573023607,0.0093594221448559,0.0103800307872189,
0.0111550321239112,0.0124465160053231,0.013791250312021,0.0141155747496086,
0.0148733761652151),.UNSPECIFIED.);
#168=B_SPLINE_CURVE_WITH_KNOTS('',3,(#16083,#16084,#16085,#16086,#16087,
#16088,#16089,#16090,#16091,#16092,#16093,#16094,#16095,#16096,#16097,#16098,
#16099,#16100,#16101,#16102,#16103,#16104,#16105,#16106,#16107,#16108,#16109,
#16110,#16111,#16112,#16113,#16114,#16115,#16116,#16117,#16118,#16119,#16120,
#16121,#16122,#16123,#16124,#16125,#16126,#16127,#16128,#16129,#16130,#16131,
#16132,#16133,#16134,#16135,#16136,#16137,#16138,#16139,#16140,#16141,#16142,
#16143,#16144,#16145,#16146,#16147,#16148,#16149),.UNSPECIFIED.,.F.,.F.,
(4,3,3,3,3,3,3,3,3,3,3,3,3,3,3,3,3,3,3,3,3,3,4),(9.27910111233108E-7,0.0388272496183639,
0.0772841574679648,0.116619782957044,0.132707521806239,0.162001548301887,
0.193238852575001,0.208023910010697,0.229368195915971,0.235345838936746,
0.249459717687539,0.259976239169003,0.270396540144426,0.283622627082234,
0.304570284853286,0.307925338554378,0.339393568656544,0.367134413731198,
0.37086179875871,0.40826291529972,0.444819006483458,0.481815249493331,0.517800460191241),
 .UNSPECIFIED.);
#169=B_SPLINE_CURVE_WITH_KNOTS('',3,(#16151,#16152,#16153,#16154,#16155,
#16156,#16157,#16158,#16159,#16160,#16161,#16162,#16163,#16164,#16165,#16166,
#16167,#16168,#16169,#16170,#16171,#16172),.UNSPECIFIED.,.F.,.F.,(4,2,2,
2,2,2,2,2,2,2,4),(9.99999880946701E-7,0.740968356548999,1.10803447596115,
1.13297439899924,1.143721929787,1.15062153269268,1.15675184018037,1.16426475270422,
1.17757025555378,1.20996329596376,1.34291541565289),.UNSPECIFIED.);
#170=B_SPLINE_CURVE_WITH_KNOTS('',3,(#16180,#16181,#16182,#16183,#16184,
#16185,#16186,#16187,#16188,#16189,#16190,#16191,#16192,#16193,#16194,#16195,
#16196,#16197,#16198,#16199,#16200,#16201,#16202,#16203,#16204,#16205,#16206,
#16207,#16208,#16209),.UNSPECIFIED.,.F.,.F.,(4,2,2,2,2,2,2,2,2,2,2,2,2,
2,4),(-1.98444564130913,-1.89114422425201,-1.7958177380882,-1.6349790573507,
-1.48026754058274,-1.31955477667618,-1.16495234940928,-1.00932603631617,
-0.850222812514903,-0.69461661564959,-0.535710588189596,-0.380118368783108,
-0.221411746164279,-0.109438295410394,0.),.UNSPECIFIED.);
#171=B_SPLINE_CURVE_WITH_KNOTS('',3,(#16214,#16215,#16216,#16217,#16218,
#16219,#16220,#16221,#16222,#16223,#16224,#16225,#16226,#16227,#16228,#16229,
#16230,#16231,#16232,#16233,#16234,#16235,#16236,#16237,#16238,#16239,#16240,
#16241,#16242,#16243),.UNSPECIFIED.,.F.,.F.,(4,2,2,2,2,2,2,2,2,2,2,2,2,
2,4),(-1.984820426919,-1.88639492736602,-1.78576272266909,-1.6246808184501,
-1.46967790916084,-1.30845849556702,-1.15333170836285,-0.992039524704425,
-0.83081389910288,-0.675813195226356,-0.514724822116692,-0.359847895242116,
-0.198896919906624,-0.0983465039006042,-9.9999998770528E-7),
 .UNSPECIFIED.);
#172=B_SPLINE_CURVE_WITH_KNOTS('',3,(#16247,#16248,#16249,#16250,#16251,
#16252,#16253,#16254,#16255,#16256,#16257,#16258,#16259,#16260,#16261,#16262,
#16263,#16264,#16265,#16266,#16267,#16268,#16269,#16270,#16271,#16272,#16273,
#16274,#16275,#16276),.UNSPECIFIED.,.F.,.F.,(4,2,2,2,2,2,2,2,2,2,2,2,2,
2,4),(-1.98444666250816,-1.89114483728254,-1.79581794294083,-1.63497942337504,
-1.48026806163894,-1.31955545877792,-1.16495318643358,-1.00932702928904,
-0.850223964920479,-0.694617923983521,-0.535712055758561,-0.380119992266497,
-0.221413528682937,-0.109439684369395,-1.00000005098799E-6),
 .UNSPECIFIED.);
#173=B_SPLINE_CURVE_WITH_KNOTS('',3,(#16281,#16282,#16283,#16284,#16285,
#16286,#16287,#16288,#16289,#16290,#16291,#16292,#16293,#16294,#16295,#16296,
#16297,#16298,#16299,#16300,#16301,#16302,#16303,#16304,#16305,#16306,#16307,
#16308,#16309,#16310),.UNSPECIFIED.,.F.,.F.,(4,2,2,2,2,2,2,2,2,2,2,2,2,
2,4),(-1.98481940872555,-1.88639386031479,-1.78576160566468,-1.62467962148561,
-1.46967663525383,-1.30845714163163,-1.15333027742346,-0.99203801370059,
-0.830812308067643,-0.675811527249796,-0.514723074176976,-0.359846070422441,
-0.198895015191813,-0.0983450528749099,0.),.UNSPECIFIED.);
#174=B_SPLINE_CURVE_WITH_KNOTS('',3,(#16314,#16315,#16316,#16317,#16318,
#16319,#16320,#16321,#16322,#16323,#16324,#16325,#16326,#16327,#16328,#16329,
#16330,#16331),.UNSPECIFIED.,.F.,.F.,(4,2,2,2,2,2,2,2,4),(-0.99035866670182,
-0.901126137518957,-0.810017339813086,-0.64988238649248,-0.495708568742823,
-0.340066262368237,-0.18191477126192,-0.0901037457175406,-1.00000003533385E-6),
 .UNSPECIFIED.);
#175=B_SPLINE_CURVE_WITH_KNOTS('',3,(#16338,#16339,#16340,#16341,#16342,
#16343,#16344,#16345,#16346,#16347),.UNSPECIFIED.,.F.,.F.,(4,2,2,2,4),(-0.354263984936231,
-0.264994680361422,-0.177037652566582,-0.0891610114015905,-1.00000006514334E-6),
 .UNSPECIFIED.);
#176=B_SPLINE_CURVE_WITH_KNOTS('',3,(#16351,#16352,#16353,#16354,#16355,
#16356,#16357,#16358,#16359,#16360),.UNSPECIFIED.,.F.,.F.,(4,2,2,2,4),(-0.353824542748299,
-0.264774556195651,-0.177007347690013,-0.0891585628061826,-9.99999994089062E-7),
 .UNSPECIFIED.);
#177=B_SPLINE_CURVE_WITH_KNOTS('',3,(#16365,#16366,#16367,#16368,#16369,
#16370,#16371,#16372,#16373,#16374),.UNSPECIFIED.,.F.,.F.,(4,2,2,2,4),(-0.354518502107395,
-0.265189138567669,-0.177165433052852,-0.0892273778761162,-1.00000006419965E-6),
 .UNSPECIFIED.);
#178=B_SPLINE_CURVE_WITH_KNOTS('',3,(#16378,#16379,#16380,#16381,#16382,
#16383,#16384,#16385,#16386,#16387),.UNSPECIFIED.,.F.,.F.,(4,2,2,2,4),(-0.354079537268672,
-0.264963089010901,-0.177134329509822,-0.0892187800375224,-1.00000006381107E-6),
 .UNSPECIFIED.);
#179=B_SPLINE_CURVE_WITH_KNOTS('',3,(#16392,#16393,#16394,#16395,#16396,
#16397,#16398,#16399,#16400,#16401),.UNSPECIFIED.,.F.,.F.,(4,2,2,2,4),(-0.354757463555714,
-0.265371721316049,-0.17728540199176,-0.0892896807913005,-1.00000006364453E-6),
 .UNSPECIFIED.);
#180=B_SPLINE_CURVE_WITH_KNOTS('',3,(#16405,#16406,#16407,#16408,#16409,
#16410,#16411,#16412,#16413,#16414),.UNSPECIFIED.,.F.,.F.,(4,2,2,2,4),(-0.354314501807183,
-0.265136819335046,-0.177251338508511,-0.0892742578316736,-1.00000006514334E-6),
 .UNSPECIFIED.);
#181=B_SPLINE_CURVE_WITH_KNOTS('',3,(#16419,#16420,#16421,#16422,#16423,
#16424,#16425,#16426,#16427,#16428),.UNSPECIFIED.,.F.,.F.,(4,2,2,2,4),(-0.354964666048056,
-0.26553004556308,-0.177389425165517,-0.0893436976482566,-9.99999990924927E-7),
 .UNSPECIFIED.);
#182=B_SPLINE_CURVE_WITH_KNOTS('',3,(#16432,#16433,#16434,#16435,#16436,
#16437,#16438,#16439,#16440,#16441),.UNSPECIFIED.,.F.,.F.,(4,2,2,2,4),(-0.354513805707218,
-0.265284187720151,-0.177350590270964,-0.0893213087125481,-1.0000000654764E-6),
 .UNSPECIFIED.);
#183=B_SPLINE_CURVE_WITH_KNOTS('',3,(#16446,#16447,#16448,#16449,#16450,
#16451,#16452,#16453,#16454,#16455),.UNSPECIFIED.,.F.,.F.,(4,2,2,2,4),(-0.355127057597616,
-0.265654134459916,-0.17747095070662,-0.0893860287446967,-9.99999999196088E-7),
 .UNSPECIFIED.);
#184=B_SPLINE_CURVE_WITH_KNOTS('',3,(#16459,#16460,#16461,#16462,#16463,
#16464,#16465,#16466,#16467,#16468),.UNSPECIFIED.,.F.,.F.,(4,2,2,2,4),(-0.354665118474449,
-0.265396073885442,-0.177425943603115,-0.0893570257229319,-9.99999998974044E-7),
 .UNSPECIFIED.);
#185=B_SPLINE_CURVE_WITH_KNOTS('',3,(#16473,#16474,#16475,#16476,#16477,
#16478,#16479,#16480,#16481,#16482),.UNSPECIFIED.,.F.,.F.,(4,2,2,2,4),(-0.355235150205187,
-0.265736734067912,-0.177525216072434,-0.0894142037588925,-1.00000006714174E-6),
 .UNSPECIFIED.);
#186=B_SPLINE_CURVE_WITH_KNOTS('',3,(#16486,#16487,#16488,#16489,#16490,
#16491,#16492,#16493,#16494,#16495),.UNSPECIFIED.,.F.,.F.,(4,2,2,2,4),(-0.354759791686021,
-0.265466080089346,-0.177473090931424,-0.0893793712074604,-9.99999999695689E-7),
 .UNSPECIFIED.);
#187=B_SPLINE_CURVE_WITH_KNOTS('',3,(#16500,#16501,#16502,#16503,#16504,
#16505,#16506,#16507,#16508,#16509),.UNSPECIFIED.,.F.,.F.,(4,2,2,2,4),(-0.355283282513423,
-0.26577351527105,-0.177549379663897,-0.0894267492827573,-1.00000006569845E-6),
 .UNSPECIFIED.);
#188=B_SPLINE_CURVE_WITH_KNOTS('',3,(#16513,#16514,#16515,#16516,#16517,
#16518,#16519,#16520,#16521,#16522),.UNSPECIFIED.,.F.,.F.,(4,2,2,2,4),(-0.354793080478592,
-0.265490695774362,-0.177489668834524,-0.0893872279312292,-9.99999999584666E-7),
 .UNSPECIFIED.);
#189=B_SPLINE_CURVE_WITH_KNOTS('',3,(#16534,#16535,#16536,#16537,#16538,
#16539,#16540,#16541,#16542,#16543,#16544,#16545,#16546,#16547,#16548,#16549,
#16550,#16551,#16552,#16553,#16554,#16555,#16556,#16557,#16558,#16559,#16560,
#16561,#16562,#16563,#16564,#16565,#16566,#16567,#16568,#16569,#16570),
 .UNSPECIFIED.,.F.,.F.,(4,3,3,3,3,3,3,3,3,3,3,3,4),(-0.195598306843679,
-0.123264481538882,-0.110045864193155,-0.103002447810529,-0.10157695259272,
-0.100794703875248,-0.100424012566965,-0.100190257704989,-0.0993931570989621,
-0.0980296806446515,-0.0926181161151234,-0.0743843579378517,-1.00000019162542E-6),
 .UNSPECIFIED.);
#190=B_SPLINE_CURVE_WITH_KNOTS('',3,(#16572,#16573,#16574,#16575),
 .UNSPECIFIED.,.F.,.F.,(4,4),(0.141911553477537,0.142385482367034),
 .UNSPECIFIED.);
#191=B_SPLINE_CURVE_WITH_KNOTS('',3,(#16577,#16578,#16579,#16580,#16581,
#16582,#16583,#16584,#16585,#16586,#16587,#16588,#16589,#16590,#16591,#16592,
#16593,#16594,#16595,#16596,#16597,#16598,#16599,#16600,#16601,#16602,#16603,
#16604,#16605,#16606,#16607,#16608,#16609,#16610,#16611,#16612,#16613),
 .UNSPECIFIED.,.F.,.F.,(4,3,3,3,3,3,3,3,3,3,3,3,4),(-0.194458103761094,
-0.134684129317144,-0.113068646531483,-0.103143192107291,-0.101588268397981,
-0.100784238137842,-0.100418705769013,-0.100119304646258,-0.0993246176591243,
-0.0979697747936403,-0.0926478893950155,-0.074330571228443,0.),
 .UNSPECIFIED.);
#192=B_SPLINE_CURVE_WITH_KNOTS('',3,(#16614,#16615,#16616,#16617),
 .UNSPECIFIED.,.F.,.F.,(4,4),(0.00134009499830981,0.00181261238932178),
 .UNSPECIFIED.);
#193=B_SPLINE_CURVE_WITH_KNOTS('',3,(#16628,#16629,#16630,#16631,#16632,
#16633,#16634,#16635,#16636,#16637,#16638,#16639,#16640,#16641,#16642,#16643,
#16644,#16645,#16646,#16647,#16648,#16649,#16650,#16651,#16652,#16653,#16654,
#16655,#16656,#16657,#16658,#16659,#16660,#16661,#16662,#16663,#16664,#16665,
#16666,#16667),.UNSPECIFIED.,.F.,.F.,(4,3,3,3,3,3,3,3,3,3,3,3,3,4),(-0.194494028891387,
-0.162125908018411,-0.119536045329343,-0.108846565940067,-0.102885128703993,
-0.101541265474887,-0.100781691030153,-0.100417518665575,-0.10012302828061,
-0.0992855890259592,-0.0977398411588879,-0.0897084819313687,-0.0744225582376583,
-1.00000019873092E-6),.UNSPECIFIED.);
#194=B_SPLINE_CURVE_WITH_KNOTS('',3,(#16669,#16670,#16671,#16672),
 .UNSPECIFIED.,.F.,.F.,(4,4),(0.140405475149255,0.140881603915338),
 .UNSPECIFIED.);
#195=B_SPLINE_CURVE_WITH_KNOTS('',3,(#16674,#16675,#16676,#16677,#16678,
#16679,#16680,#16681,#16682,#16683,#16684,#16685,#16686,#16687,#16688,#16689,
#16690,#16691,#16692,#16693,#16694,#16695,#16696,#16697,#16698,#16699,#16700,
#16701,#16702,#16703,#16704,#16705,#16706,#16707,#16708,#16709,#16710),
 .UNSPECIFIED.,.F.,.F.,(4,3,3,3,3,3,3,3,3,3,3,3,4),(-0.194436193946118,
-0.144932886173553,-0.115563305609625,-0.103254995613247,-0.101617470978299,
-0.100796695496138,-0.100431864202833,-0.10013062822708,-0.099348493432612,
-0.098048610059559,-0.0933182996091218,-0.0753172897329091,0.),
 .UNSPECIFIED.);
#196=B_SPLINE_CURVE_WITH_KNOTS('',3,(#16711,#16712,#16713,#16714),
 .UNSPECIFIED.,.F.,.F.,(4,4),(0.002838891359255,0.0033137097483393),
 .UNSPECIFIED.);
#197=B_SPLINE_CURVE_WITH_KNOTS('',3,(#16725,#16726,#16727,#16728,#16729,
#16730,#16731,#16732,#16733,#16734,#16735,#16736,#16737,#16738,#16739,#16740,
#16741,#16742,#16743,#16744,#16745,#16746,#16747,#16748,#16749,#16750,#16751,
#16752,#16753,#16754,#16755,#16756,#16757,#16758),.UNSPECIFIED.,.F.,.F.,
(4,3,3,3,3,3,3,3,3,3,3,4),(-0.19435323528279,-0.124535619715197,-0.106070197067798,
-0.102599335626109,-0.101487874003443,-0.100780098417182,-0.100427674373929,
-0.10010644945315,-0.0991724103632078,-0.0971568831920127,-0.0759588650073846,
-1.00000018861696E-6),.UNSPECIFIED.);
#198=B_SPLINE_CURVE_WITH_KNOTS('',3,(#16760,#16761,#16762,#16763),
 .UNSPECIFIED.,.F.,.F.,(4,4),(0.134372093107689,0.134872686417409),
 .UNSPECIFIED.);
#199=B_SPLINE_CURVE_WITH_KNOTS('',3,(#16765,#16766,#16767,#16768,#16769,
#16770,#16771,#16772,#16773,#16774,#16775,#16776,#16777,#16778,#16779,#16780,
#16781,#16782,#16783,#16784,#16785,#16786,#16787,#16788,#16789,#16790,#16791,
#16792,#16793,#16794,#16795,#16796,#16797,#16798),.UNSPECIFIED.,.F.,.F.,
(4,3,3,3,3,3,3,3,3,3,3,4),(-0.194392555335661,-0.123344459486231,-0.103739879120015,
-0.101678198852006,-0.100778062576977,-0.100422358916701,-0.10010239570925,
-0.0993609150724121,-0.0982389457672826,-0.0950358831823619,-0.075424087699,
0.),.UNSPECIFIED.);
#200=B_SPLINE_CURVE_WITH_KNOTS('',3,(#16799,#16800,#16801,#16802),
 .UNSPECIFIED.,.F.,.F.,(4,4),(0.00882605152059419,0.00932569413867771),
 .UNSPECIFIED.);
#201=B_SPLINE_CURVE_WITH_KNOTS('',3,(#16813,#16814,#16815,#16816,#16817,
#16818,#16819,#16820,#16821,#16822,#16823,#16824,#16825,#16826,#16827,#16828,
#16829,#16830,#16831,#16832,#16833,#16834,#16835,#16836,#16837,#16838,#16839,
#16840,#16841,#16842,#16843,#16844,#16845,#16846,#16847,#16848,#16849),
 .UNSPECIFIED.,.F.,.F.,(4,3,3,3,3,3,3,3,3,3,3,3,4),(-0.194157876185446,
-0.124533044815514,-0.106352198581866,-0.102421387170606,-0.101257165736826,
-0.100537645142505,-0.100181415933288,-0.0998675692180962,-0.0989614751107034,
-0.0970886950782979,-0.0795114673901098,-0.0324255403862385,-1.00000007903258E-6),
 .UNSPECIFIED.);
#202=B_SPLINE_CURVE_WITH_KNOTS('',3,(#16851,#16852,#16853,#16854),
 .UNSPECIFIED.,.F.,.F.,(4,4),(0.13588184021166,0.136373897134007),
 .UNSPECIFIED.);
#203=B_SPLINE_CURVE_WITH_KNOTS('',3,(#16856,#16857,#16858,#16859,#16860,
#16861,#16862,#16863,#16864,#16865,#16866,#16867,#16868,#16869,#16870,#16871,
#16872,#16873,#16874,#16875,#16876,#16877,#16878,#16879,#16880,#16881,#16882,
#16883,#16884,#16885,#16886,#16887,#16888,#16889),.UNSPECIFIED.,.F.,.F.,
(4,3,3,3,3,3,3,3,3,3,3,4),(-0.194441151898413,-0.123303248261605,-0.103612149587876,
-0.101673331691855,-0.100795113504573,-0.100436213890763,-0.100122644799755,
-0.0993723218297423,-0.0982113052533252,-0.0947158338413571,-0.076129474606578,
0.),.UNSPECIFIED.);
#204=B_SPLINE_CURVE_WITH_KNOTS('',3,(#16890,#16891,#16892,#16893),
 .UNSPECIFIED.,.F.,.F.,(4,4),(0.00733049598192872,0.0078215204041217),
 .UNSPECIFIED.);
#205=B_SPLINE_CURVE_WITH_KNOTS('',3,(#16904,#16905,#16906,#16907,#16908,
#16909,#16910,#16911,#16912,#16913,#16914,#16915,#16916,#16917,#16918,#16919,
#16920,#16921,#16922,#16923,#16924,#16925,#16926,#16927,#16928,#16929,#16930,
#16931,#16932,#16933,#16934,#16935,#16936,#16937,#16938,#16939,#16940),
 .UNSPECIFIED.,.F.,.F.,(4,3,3,3,3,3,3,3,3,3,3,3,4),(-0.195323898017394,
-0.124294804269522,-0.107255118396146,-0.102731117250133,-0.101499027233354,
-0.100759964465065,-0.100395632571243,-0.100153343276803,-0.0993052369896065,
-0.0977122022557945,-0.0888118939699463,-0.0729373309057275,-1.00000018948831E-6),
 .UNSPECIFIED.);
#206=B_SPLINE_CURVE_WITH_KNOTS('',3,(#16942,#16943,#16944,#16945),
 .UNSPECIFIED.,.F.,.F.,(4,4),(0.137390638838294,0.137875797145181),
 .UNSPECIFIED.);
#207=B_SPLINE_CURVE_WITH_KNOTS('',3,(#16947,#16948,#16949,#16950,#16951,
#16952,#16953,#16954,#16955,#16956,#16957,#16958,#16959,#16960,#16961,#16962,
#16963,#16964,#16965,#16966,#16967,#16968,#16969,#16970,#16971,#16972,#16973,
#16974,#16975,#16976,#16977,#16978,#16979,#16980),.UNSPECIFIED.,.F.,.F.,
(4,3,3,3,3,3,3,3,3,3,3,4),(-0.194460770152194,-0.123138826518747,-0.103467518298517,
-0.101639305168327,-0.100781542294932,-0.100420043418356,-0.100111728380133,
-0.0993517235744529,-0.0981483078455959,-0.0943102495859858,-0.0747206712961253,
0.),.UNSPECIFIED.);
#208=B_SPLINE_CURVE_WITH_KNOTS('',3,(#16981,#16982,#16983,#16984),
 .UNSPECIFIED.,.F.,.F.,(4,4),(0.00583410702683465,0.00631814513922487),
 .UNSPECIFIED.);
#209=B_SPLINE_CURVE_WITH_KNOTS('',3,(#16995,#16996,#16997,#16998,#16999,
#17000,#17001,#17002,#17003,#17004,#17005,#17006,#17007,#17008,#17009,#17010,
#17011,#17012,#17013,#17014,#17015,#17016,#17017,#17018,#17019,#17020,#17021,
#17022,#17023,#17024,#17025,#17026,#17027,#17028,#17029,#17030,#17031),
 .UNSPECIFIED.,.F.,.F.,(4,3,3,3,3,3,3,3,3,3,3,3,4),(-0.194354595634486,
-0.124820448572211,-0.107845859548302,-0.102700952796982,-0.101421142037528,
-0.100675980132718,-0.100314095496492,-0.100010428444396,-0.0991509263640827,
-0.0975029450999708,-0.0874063402276625,-0.0661239178086379,-1.00000017532684E-6),
 .UNSPECIFIED.);
#210=B_SPLINE_CURVE_WITH_KNOTS('',3,(#17033,#17034,#17035,#17036),
 .UNSPECIFIED.,.F.,.F.,(4,4),(0.138898510273107,0.139378370938015),
 .UNSPECIFIED.);
#211=B_SPLINE_CURVE_WITH_KNOTS('',3,(#17038,#17039,#17040,#17041,#17042,
#17043,#17044,#17045,#17046,#17047,#17048,#17049,#17050,#17051,#17052,#17053,
#17054,#17055,#17056,#17057,#17058,#17059,#17060,#17061,#17062,#17063,#17064,
#17065,#17066,#17067,#17068,#17069,#17070,#17071,#17072,#17073,#17074),
 .UNSPECIFIED.,.F.,.F.,(4,3,3,3,3,3,3,3,3,3,3,3,4),(-0.19441619914366,-0.161480406225361,
-0.119240121158241,-0.103349474438416,-0.101621236163409,-0.100782583552426,
-0.100419101429683,-0.100114896575942,-0.099344306124858,-0.0980947432494325,
-0.093850925665231,-0.0744872008833497,0.),.UNSPECIFIED.);
#212=B_SPLINE_CURVE_WITH_KNOTS('',3,(#17075,#17076,#17077,#17078),
 .UNSPECIFIED.,.F.,.F.,(4,4),(0.00433690036911171,0.00481554798135458),
 .UNSPECIFIED.);
#213=B_SPLINE_CURVE_WITH_KNOTS('',3,(#17086,#17087,#17088,#17089,#17090,
#17091),.UNSPECIFIED.,.F.,.F.,(4,2,4),(-0.14333107944773,-0.0736159262229404,
0.),.UNSPECIFIED.);
#214=B_SPLINE_CURVE_WITH_KNOTS('',3,(#17095,#17096,#17097,#17098,#17099,
#17100),.UNSPECIFIED.,.F.,.F.,(4,2,4),(-0.147015175052716,-0.0741905379943431,
-9.99999944489849E-7),.UNSPECIFIED.);
#215=B_SPLINE_CURVE_WITH_KNOTS('',3,(#17104,#17105,#17106,#17107,#17108,
#17109),.UNSPECIFIED.,.F.,.F.,(4,2,4),(-0.143331079447973,-0.0736164030416013,
0.),.UNSPECIFIED.);
#216=B_SPLINE_CURVE_WITH_KNOTS('',3,(#17113,#17114,#17115,#17116,#17117,
#17118),.UNSPECIFIED.,.F.,.F.,(4,2,4),(-0.147015175052249,-0.0741900426363321,
-9.99999949590951E-7),.UNSPECIFIED.);
#217=B_SPLINE_CURVE_WITH_KNOTS('',3,(#17122,#17123,#17124,#17125,#17126,
#17127),.UNSPECIFIED.,.F.,.F.,(4,2,4),(-0.143331079446318,-0.07361640304082,
0.),.UNSPECIFIED.);
#218=B_SPLINE_CURVE_WITH_KNOTS('',3,(#17131,#17132,#17133,#17134,#17135,
#17136),.UNSPECIFIED.,.F.,.F.,(4,2,4),(-0.147015175052338,-0.0741905379942694,
-9.99999947848274E-7),.UNSPECIFIED.);
#219=B_SPLINE_CURVE_WITH_KNOTS('',3,(#17140,#17141,#17142,#17143,#17144,
#17145),.UNSPECIFIED.,.F.,.F.,(4,2,4),(-0.143331079445893,-0.0736164030406679,
0.),.UNSPECIFIED.);
#220=B_SPLINE_CURVE_WITH_KNOTS('',3,(#17149,#17150,#17151,#17152,#17153,
#17154),.UNSPECIFIED.,.F.,.F.,(4,2,4),(-0.147015175052675,-0.074190537994313,
-9.99999944878427E-7),.UNSPECIFIED.);
#221=B_SPLINE_CURVE_WITH_KNOTS('',3,(#17158,#17159,#17160,#17161,#17162,
#17163),.UNSPECIFIED.,.F.,.F.,(4,2,4),(-0.143331079449217,-0.0736164030425967,
0.),.UNSPECIFIED.);
#222=B_SPLINE_CURVE_WITH_KNOTS('',3,(#17167,#17168,#17169,#17170,#17171,
#17172),.UNSPECIFIED.,.F.,.F.,(4,2,4),(-0.147015175052563,-0.0741905379943041,
-9.99999946987851E-7),.UNSPECIFIED.);
#223=B_SPLINE_CURVE_WITH_KNOTS('',3,(#17176,#17177,#17178,#17179,#17180,
#17181),.UNSPECIFIED.,.F.,.F.,(4,2,4),(-0.143331079448333,-0.0736159262229434,
0.),.UNSPECIFIED.);
#224=B_SPLINE_CURVE_WITH_KNOTS('',3,(#17185,#17186,#17187,#17188,#17189,
#17190),.UNSPECIFIED.,.F.,.F.,(4,2,4),(-0.147015175052789,-0.0741900426364876,
-9.99999946378767E-7),.UNSPECIFIED.);
#225=B_SPLINE_CURVE_WITH_KNOTS('',3,(#17194,#17195,#17196,#17197,#17198,
#17199),.UNSPECIFIED.,.F.,.F.,(4,2,4),(-0.143331079447819,-0.0736164030417104,
0.),.UNSPECIFIED.);
#226=B_SPLINE_CURVE_WITH_KNOTS('',3,(#17201,#17202,#17203,#17204,#17205,
#17206),.UNSPECIFIED.,.F.,.F.,(4,2,4),(-0.0412408216537853,-0.0206214941513466,
-1.00000001180406E-6),.UNSPECIFIED.);
#227=B_SPLINE_CURVE_WITH_KNOTS('',3,(#17218,#17219,#17220,#17221,#17222,
#17223,#17224,#17225,#17226,#17227,#17228,#17229,#17230,#17231,#17232,#17233,
#17234,#17235,#17236,#17237,#17238,#17239,#17240,#17241,#17242,#17243,#17244,
#17245,#17246,#17247,#17248,#17249,#17250,#17251,#17252,#17253,#17254,#17255,
#17256,#17257,#17258,#17259,#17260,#17261,#17262,#17263,#17264,#17265,#17266,
#17267,#17268,#17269,#17270,#17271,#17272,#17273,#17274,#17275,#17276,#17277,
#17278,#17279,#17280,#17281,#17282,#17283,#17284,#17285,#17286,#17287),
 .UNSPECIFIED.,.F.,.F.,(4,3,3,3,3,3,3,3,3,3,3,3,3,3,3,3,3,3,3,3,3,3,3,4),
(0.0481874539974375,0.0604511794446379,0.070528500825075,0.0734860385296239,
0.0816990242388937,0.0865209011059417,0.0928695476527125,0.0930383208706332,
0.0984548093596218,0.0995557664417368,0.104040071066531,0.106073179694452,
0.112590606795416,0.11521059448035,0.119108035899913,0.120795856187259,
0.124177092586103,0.125625561625231,0.126381117894169,0.128882895010381,
0.131966379601078,0.132137852941708,0.136965611308967,0.137551641307987),
 .UNSPECIFIED.);
#228=B_SPLINE_CURVE_WITH_KNOTS('',3,(#17303,#17304,#17305,#17306,#17307,
#17308,#17309,#17310,#17311,#17312,#17313,#17314,#17315,#17316,#17317,#17318),
 .UNSPECIFIED.,.F.,.F.,(4,2,2,2,2,2,2,4),(1.00000015767795E-6,0.0566419671564676,
0.112784425720308,0.12743749066151,0.133720994177815,0.139633617857089,
0.183920433299157,0.225783248401836),.UNSPECIFIED.);
#229=B_SPLINE_CURVE_WITH_KNOTS('',3,(#17319,#17320,#17321,#17322,#17323,
#17324,#17325,#17326,#17327,#17328,#17329,#17330,#17331,#17332,#17333,#17334,
#17335,#17336),.UNSPECIFIED.,.F.,.F.,(4,2,2,2,2,2,2,2,4),(0.,0.0401671331759944,
0.0854041510983084,0.088451528257622,0.0916096770996849,0.0983906908764339,
0.112644364639411,0.170245279340444,0.225566054832859),.UNSPECIFIED.);
#230=B_SPLINE_CURVE_WITH_KNOTS('',3,(#17349,#17350,#17351,#17352,#17353,
#17354,#17355,#17356,#17357,#17358,#17359,#17360,#17361,#17362,#17363,#17364,
#17365,#17366),.UNSPECIFIED.,.F.,.F.,(4,2,2,2,2,2,2,2,4),(1.00000015378182E-6,
0.0558033364890031,0.111947159620381,0.126596830926891,0.132828265004497,
0.135756028209409,0.138596448354699,0.182551382377112,0.224108739412938),
 .UNSPECIFIED.);
#231=B_SPLINE_CURVE_WITH_KNOTS('',3,(#17367,#17368,#17369,#17370,#17371,
#17372,#17373,#17374,#17375,#17376,#17377,#17378,#17379,#17380,#17381,#17382),
 .UNSPECIFIED.,.F.,.F.,(4,2,2,2,2,2,2,4),(0.,0.0397861978551001,0.084544977734077,
0.0907978235304521,0.0975212072539927,0.111776839943134,0.169529074612989,
0.223835312885583),.UNSPECIFIED.);
#232=B_SPLINE_CURVE_WITH_KNOTS('',3,(#17395,#17396,#17397,#17398,#17399,
#17400,#17401,#17402,#17403,#17404,#17405,#17406,#17407,#17408,#17409,#17410),
 .UNSPECIFIED.,.F.,.F.,(4,2,2,2,2,2,2,4),(1.00000015458341E-6,0.0551170619821043,
0.111258895694281,0.125906053027141,0.132093950533861,0.137915824051536,
0.181508333049727,0.22273106176126),.UNSPECIFIED.);
#233=B_SPLINE_CURVE_WITH_KNOTS('',3,(#17411,#17412,#17413,#17414,#17415,
#17416,#17417,#17418,#17419,#17420,#17421,#17422,#17423,#17424,#17425,#17426),
 .UNSPECIFIED.,.F.,.F.,(4,2,2,2,2,2,2,4),(0.,0.0409142927088161,0.0870329656864442,
0.090140402195948,0.0968150072471416,0.11107376451763,0.168959944123858,
0.222415697934881),.UNSPECIFIED.);
#234=B_SPLINE_CURVE_WITH_KNOTS('',3,(#17439,#17440,#17441,#17442,#17443,
#17444,#17445,#17446,#17447,#17448,#17449,#17450,#17451,#17452,#17453,#17454),
 .UNSPECIFIED.,.F.,.F.,(4,2,2,2,2,2,2,4),(1.00000015245565E-6,0.0545871826959916,
0.110723454503288,0.125369052976213,0.131522194169781,0.137311275351113,
0.18065802848448,0.221659371342439),.UNSPECIFIED.);
#235=B_SPLINE_CURVE_WITH_KNOTS('',3,(#17455,#17456,#17457,#17458,#17459,
#17460,#17461,#17462,#17463,#17464,#17465,#17466,#17467,#17468,#17469,#17470),
 .UNSPECIFIED.,.F.,.F.,(4,2,2,2,2,2,2,4),(0.,0.0406903828664926,0.0865151821863462,
0.0896037483126215,0.0962386252435175,0.110500789147319,0.168500019068009,
0.221271398664186),.UNSPECIFIED.);
#236=B_SPLINE_CURVE_WITH_KNOTS('',3,(#17483,#17484,#17485,#17486,#17487,
#17488,#17489,#17490,#17491,#17492,#17493,#17494,#17495,#17496,#17497,#17498),
 .UNSPECIFIED.,.F.,.F.,(4,2,2,2,2,2,2,4),(1.00000015268294E-6,0.0542163947487819,
0.110343410733279,0.124212476892867,0.130385053869933,0.136193595788229,
0.179714725892929,0.220902014754228),.UNSPECIFIED.);
#237=B_SPLINE_CURVE_WITH_KNOTS('',3,(#17499,#17500,#17501,#17502,#17503,
#17504,#17505,#17506,#17507,#17508,#17509,#17510,#17511,#17512,#17513,#17514),
 .UNSPECIFIED.,.F.,.F.,(4,2,2,2,2,2,2,4),(0.,0.039140602667914,0.0830524217192137,
0.0891911669334346,0.095795784554504,0.110061497078605,0.168152629570437,
0.220408984280307),.UNSPECIFIED.);
#238=B_SPLINE_CURVE_WITH_KNOTS('',3,(#17527,#17528,#17529,#17530,#17531,
#17532,#17533,#17534,#17535,#17536,#17537,#17538,#17539,#17540,#17541,#17542),
 .UNSPECIFIED.,.F.,.F.,(4,2,2,2,2,2,2,4),(9.9999962800122E-7,0.0540058272398856,
0.110119887130061,0.123968789679388,0.130125700954026,0.135919865126588,
0.179343774956579,0.220454906422694),.UNSPECIFIED.);
#239=B_SPLINE_CURVE_WITH_KNOTS('',3,(#17543,#17544,#17545,#17546,#17547,
#17548,#17549,#17550,#17551,#17552,#17553,#17554,#17555,#17556),
 .UNSPECIFIED.,.F.,.F.,(4,2,2,2,2,2,4),(0.,0.0388549911094784,0.0823949291517112,
0.0955223331063072,0.109792272136123,0.167956881450626,0.21987139248006),
 .UNSPECIFIED.);
#240=B_SPLINE_CURVE_WITH_KNOTS('',3,(#17570,#17571,#17572,#17573,#17574,
#17575,#17576,#17577,#17578,#17579,#17580,#17581,#17582,#17583),
 .UNSPECIFIED.,.F.,.F.,(4,2,2,2,2,2,4),(0.,0.038846670414078,0.0823248638019488,
0.0954305814969146,0.109709621306899,0.167964127673705,0.219706780889003),
 .UNSPECIFIED.);
#241=B_SPLINE_CURVE_WITH_KNOTS('',3,(#17586,#17587,#17588,#17589,#17590,
#17591,#17592,#17593,#17594,#17595,#17596,#17597,#17598,#17599,#17600,#17601),
 .UNSPECIFIED.,.F.,.F.,(4,2,2,2,2,2,2,4),(1.00000015172994E-6,0.0540638821572014,
0.11014021259305,0.124011364716217,0.130159885420681,0.135947500297997,
0.179358237230156,0.220496798577425),.UNSPECIFIED.);
#242=B_SPLINE_CURVE_WITH_KNOTS('',3,(#17615,#17616,#17617,#17618,#17619,
#17620,#17621,#17622,#17623,#17624,#17625,#17626,#17627,#17628),
 .UNSPECIFIED.,.F.,.F.,(4,2,2,2,2,2,4),(0.,0.0389316508749848,0.0824851666861475,
0.0956106643644333,0.109894565357363,0.168167665939653,0.220077044238227),
 .UNSPECIFIED.);
#243=B_SPLINE_CURVE_WITH_KNOTS('',3,(#17631,#17632,#17633,#17634,#17635,
#17636,#17637,#17638,#17639,#17640,#17641,#17642,#17643,#17644,#17645,#17646),
 .UNSPECIFIED.,.F.,.F.,(4,2,2,2,2,2,2,4),(9.99999733883172E-7,0.0543338500939956,
0.110384986534261,0.124299234975658,0.130454753460029,0.136249978201543,
0.179744351784844,0.220987670436901),.UNSPECIFIED.);
#244=B_SPLINE_CURVE_WITH_KNOTS('',3,(#17660,#17661,#17662,#17663,#17664,
#17665,#17666,#17667,#17668,#17669,#17670,#17671,#17672,#17673,#17674,#17675),
 .UNSPECIFIED.,.F.,.F.,(4,2,2,2,2,2,2,4),(0.,0.0392686346462967,0.0832009038398811,
0.0893387848744381,0.0959430114101636,0.110232011346826,0.168506578804678,
0.220751898189097),.UNSPECIFIED.);
#245=B_SPLINE_CURVE_WITH_KNOTS('',3,(#17678,#17679,#17680,#17681,#17682,
#17683,#17684,#17685,#17686,#17687,#17688,#17689,#17690,#17691,#17692,#17693),
 .UNSPECIFIED.,.F.,.F.,(4,2,2,2,2,2,2,4),(9.99999694798638E-7,0.054765186443432,
0.110787756000683,0.124766747937571,0.130936736325675,0.136746840437026,
0.180385329895753,0.221794905871534),.UNSPECIFIED.);
#246=B_SPLINE_CURVE_WITH_KNOTS('',3,(#17707,#17708,#17709,#17710,#17711,
#17712,#17713,#17714,#17715,#17716,#17717,#17718,#17719,#17720,#17721,#17722),
 .UNSPECIFIED.,.F.,.F.,(4,2,2,2,2,2,2,4),(0.,0.0408739056675736,0.0867208225315575,
0.0898091363774199,0.0964435146083802,0.110738149517396,0.168998361491458,
0.221749184254011),.UNSPECIFIED.);
#247=B_SPLINE_CURVE_WITH_KNOTS('',3,(#17725,#17726,#17727,#17728,#17729,
#17730,#17731,#17732,#17733,#17734,#17735,#17736,#17737,#17738,#17739,#17740,
#17741,#17742),.UNSPECIFIED.,.F.,.F.,(4,2,2,2,2,2,2,2,4),(1.0000001542254E-6,
0.0553562490243362,0.111347973454671,0.125413378119285,0.13160524711844,
0.134516642372091,0.140176624201263,0.182626732587682,0.222901923225939),
 .UNSPECIFIED.);
#248=B_SPLINE_CURVE_WITH_KNOTS('',3,(#17756,#17757,#17758,#17759,#17760,
#17761,#17762,#17763,#17764,#17765,#17766,#17767,#17768,#17769,#17770,#17771),
 .UNSPECIFIED.,.F.,.F.,(4,2,2,2,2,2,2,4),(0.,0.0397423041374614,0.0841800463334577,
0.0903840838386645,0.0970580150081825,0.111357802402403,0.169584115209849,
0.223003636179411),.UNSPECIFIED.);
#249=B_SPLINE_CURVE_WITH_KNOTS('',3,(#17774,#17775,#17776,#17777,#17778,
#17779,#17780,#17781,#17782,#17783,#17784,#17785,#17786,#17787,#17788,#17789,
#17790,#17791),.UNSPECIFIED.,.F.,.F.,(4,2,2,2,2,2,2,2,4),(1.00000015667271E-6,
0.05610406193974,0.112063656979094,0.1267391800453,0.132931491224511,0.135843444218188,
0.138670210782974,0.182598137801834,0.2243485614711),.UNSPECIFIED.);
#250=B_SPLINE_CURVE_WITH_KNOTS('',3,(#17805,#17806,#17807,#17808,#17809,
#17810,#17811,#17812,#17813,#17814,#17815,#17816,#17817,#17818,#17819,#17820,
#17821,#17822),.UNSPECIFIED.,.F.,.F.,(4,2,2,2,2,2,2,2,4),(0.,0.0401135485226958,
0.0849628399941787,0.0879826739139531,0.0911130528346559,0.0978362772912048,
0.112141694870289,0.170319870714651,0.224570333252864),.UNSPECIFIED.);
#251=B_SPLINE_CURVE_WITH_KNOTS('',3,(#17825,#17826,#17827,#17828,#17829,
#17830,#17831,#17832,#17833,#17834,#17835,#17836,#17837,#17838),
 .UNSPECIFIED.,.F.,.F.,(4,2,2,2,2,2,4),(1.00000015712895E-6,0.0570055155829236,
0.112931585188432,0.127617025456474,0.152457956486069,0.190231269095715,
0.226037592522236),.UNSPECIFIED.);
#252=B_SPLINE_CURVE_WITH_KNOTS('',3,(#17914,#17915,#17916,#17917,#17918,
#17919,#17920,#17921,#17922,#17923),.UNSPECIFIED.,.F.,.F.,(4,2,2,2,4),(-0.585264524702013,
-0.413512903650657,-0.255832772201376,-0.111462969969327,-1.00000008418366E-6),
 .UNSPECIFIED.);
#253=B_SPLINE_CURVE_WITH_KNOTS('',3,(#17949,#17950,#17951,#17952,#17953,
#17954,#17955,#17956,#17957,#17958,#17959,#17960,#17961,#17962,#17963,#17964,
#17965,#17966,#17967,#17968,#17969,#17970,#17971,#17972,#17973,#17974,#17975,
#17976,#17977,#17978,#17979,#17980,#17981,#17982,#17983,#17984,#17985,#17986,
#17987,#17988,#17989,#17990,#17991,#17992,#17993,#17994,#17995,#17996,#17997,
#17998,#17999,#18000,#18001,#18002,#18003,#18004,#18005,#18006,#18007,#18008,
#18009,#18010,#18011,#18012,#18013,#18014,#18015,#18016,#18017,#18018,#18019,
#18020,#18021,#18022,#18023,#18024,#18025,#18026,#18027,#18028,#18029,#18030,
#18031,#18032,#18033,#18034,#18035,#18036,#18037,#18038,#18039,#18040,#18041,
#18042,#18043,#18044,#18045),.UNSPECIFIED.,.F.,.F.,(4,3,3,3,3,3,3,3,3,3,
3,3,3,3,3,3,3,3,3,3,3,3,3,3,3,3,3,3,3,3,3,3,4),(0.00520390849053931,0.0111835548209164,
0.012118997686005,0.0144941590703358,0.0175378069916795,0.0178073866881133,
0.0184477217574606,0.0215855252002216,0.0237812844703456,0.0244250135230592,
0.0277183120730455,0.0302238583774399,0.0310116106230319,0.034285860301359,
0.0369003334813381,0.0375601099796862,0.0419321400689772,0.0440789397487643,
0.0473302468073634,0.0488344027844652,0.050350039614148,0.0505815538659626,
0.0545489282567866,0.056285549733304,0.0570785274976558,0.0635772982300868,
0.0675410633768119,0.0700760689625178,0.07874287737638,0.0830884508286058,
0.0925219281812085,0.0961152797092054,0.10693113025843),.UNSPECIFIED.);
#254=B_SPLINE_CURVE_WITH_KNOTS('',3,(#18048,#18049,#18050,#18051,#18052,
#18053,#18054,#18055,#18056,#18057,#18058,#18059,#18060,#18061,#18062,#18063,
#18064,#18065,#18066,#18067,#18068,#18069,#18070,#18071,#18072,#18073),
 .UNSPECIFIED.,.F.,.F.,(4,2,2,2,2,2,2,2,2,2,2,2,4),(0.0365380202373312,
0.04920852331164,0.0618790595466603,0.0745495957816805,0.0872201320167008,
0.093555400134211,0.0998906682517212,0.106225936369231,0.112561204486741,
0.118896472604252,0.125231740721762,0.131567008839272,0.137902275881919),
 .UNSPECIFIED.);
#255=B_SPLINE_CURVE_WITH_KNOTS('',3,(#18153,#18154,#18155,#18156,#18157,
#18158,#18159,#18160,#18161,#18162,#18163,#18164,#18165,#18166,#18167,#18168,
#18169,#18170,#18171,#18172,#18173,#18174,#18175,#18176,#18177,#18178,#18179,
#18180,#18181,#18182,#18183,#18184,#18185,#18186,#18187,#18188,#18189,#18190,
#18191,#18192,#18193,#18194,#18195,#18196,#18197,#18198,#18199,#18200,#18201,
#18202,#18203,#18204,#18205,#18206,#18207,#18208,#18209,#18210,#18211,#18212,
#18213,#18214,#18215,#18216,#18217,#18218,#18219,#18220,#18221,#18222,#18223,
#18224,#18225),.UNSPECIFIED.,.F.,.F.,(4,3,3,3,3,3,3,3,3,3,3,3,3,3,3,3,3,
3,3,3,3,3,3,3,4),(0.00520886345403039,0.00970120603013346,0.0106439945563895,
0.0108154787072623,0.0139735509194556,0.0164220939604942,0.0171820088000305,
0.0204031582895172,0.0220287092137261,0.0237260172021366,0.0276353244669579,
0.030270007008701,0.0368139948663752,0.0388485549734217,0.043357966798868,
0.0444551702266536,0.0495865075309555,0.0499019750475477,0.0500617854798855,
0.05644595420659,0.0612750159863493,0.06953393868509,0.0724882464928131,
0.0826219208929852,0.0949147075057406),.UNSPECIFIED.);
#256=B_SPLINE_CURVE_WITH_KNOTS('',3,(#18226,#18227,#18228,#18229,#18230,
#18231,#18232,#18233,#18234,#18235,#18236,#18237),.UNSPECIFIED.,.F.,.F.,
(4,2,2,2,2,4),(0.,0.0299527642720166,0.0619423015472164,0.120911888659585,
0.180698800964258,0.241792534958426),.UNSPECIFIED.);
#257=B_SPLINE_CURVE_WITH_KNOTS('',3,(#18322,#18323,#18324,#18325,#18326,
#18327,#18328,#18329,#18330,#18331,#18332,#18333),.UNSPECIFIED.,.F.,.F.,
(4,2,2,2,2,4),(1.00000010262874E-6,0.0610883129182119,0.120980470221561,
0.180061968201615,0.212160232587823,0.242212526403015),.UNSPECIFIED.);
#258=B_SPLINE_CURVE_WITH_KNOTS('',3,(#18346,#18347,#18348,#18349,#18350,
#18351,#18352,#18353,#18354,#18355,#18356,#18357,#18358,#18359,#18360,#18361,
#18362,#18363,#18364,#18365,#18366,#18367,#18368,#18369,#18370,#18371,#18372,
#18373,#18374,#18375,#18376),.UNSPECIFIED.,.F.,.F.,(4,3,3,3,3,3,3,3,3,3,
4),(0.,0.000294988744227459,0.000591621339744572,0.000703775434139677,0.00140755086827935,
0.00211132630241903,0.00281510173655871,0.00351887717069839,0.00422265260483806,
0.00492642803897774,0.00563020347311742),.UNSPECIFIED.);
#259=B_SPLINE_CURVE_WITH_KNOTS('',3,(#18386,#18387,#18388,#18389,#18390,
#18391,#18392,#18393,#18394,#18395,#18396,#18397,#18398,#18399,#18400,#18401,
#18402,#18403,#18404,#18405,#18406,#18407,#18408,#18409,#18410,#18411,#18412,
#18413,#18414,#18415,#18416,#18417,#18418,#18419,#18420,#18421,#18422),
 .UNSPECIFIED.,.F.,.F.,(4,3,3,3,3,3,3,3,3,3,3,3,4),(0.,0.000230876498533257,
0.000465662459581963,0.000700448420630669,0.000975047322199287,0.00124663139837462,
0.00140089684126134,0.00210134526189201,0.00280179368252268,0.00350224210315334,
0.00420269052378401,0.00490313894441468,0.00560358736504535),
 .UNSPECIFIED.);
#260=B_SPLINE_CURVE_WITH_KNOTS('',3,(#18442,#18443,#18444,#18445,#18446,
#18447,#18448,#18449,#18450,#18451,#18452,#18453),.UNSPECIFIED.,.F.,.F.,
(4,2,2,2,2,4),(-0.426179478037512,-0.32445407038533,-0.214075470571974,
-0.161545733302206,-0.0817578221150203,0.),.UNSPECIFIED.);
#261=B_SPLINE_CURVE_WITH_KNOTS('',3,(#18455,#18456,#18457,#18458,#18459,
#18460),.UNSPECIFIED.,.F.,.F.,(4,2,4),(-0.150501180006049,-0.0752447108658683,
-1.00000001429512E-6),.UNSPECIFIED.);
#262=B_SPLINE_CURVE_WITH_KNOTS('',3,(#18480,#18481,#18482,#18483,#18484,
#18485),.UNSPECIFIED.,.F.,.F.,(4,2,4),(-0.150600801674249,-0.0756430925380589,
0.),.UNSPECIFIED.);
#263=B_SPLINE_CURVE_WITH_KNOTS('',3,(#18487,#18488,#18489,#18490,#18491,
#18492,#18493,#18494,#18495,#18496,#18497,#18498),.UNSPECIFIED.,.F.,.F.,
(4,2,2,2,2,4),(-0.43181117785828,-0.349168381037158,-0.268518618936436,
-0.215365450898843,-0.103278388757051,-8.24157489365263E-7),
 .UNSPECIFIED.);
#264=B_SPLINE_CURVE_WITH_KNOTS('',3,(#18522,#18523,#18524,#18525,#18526,
#18527,#18528,#18529,#18530,#18531,#18532,#18533,#18534,#18535,#18536,#18537,
#18538,#18539,#18540,#18541,#18542,#18543,#18544,#18545,#18546,#18547),
 .UNSPECIFIED.,.F.,.F.,(4,2,2,2,2,2,2,2,2,2,2,2,4),(0.,0.0178777739260339,
0.0357555478520677,0.0536333217781016,0.0715110957041355,0.0804499826671525,
0.0893888696301694,0.0983277565931864,0.107266643556203,0.11620553051922,
0.125144417482237,0.134083304445254,0.143022191408271),.UNSPECIFIED.);
#265=B_SPLINE_CURVE_WITH_KNOTS('',3,(#18550,#18551,#18552,#18553,#18554,
#18555,#18556,#18557,#18558,#18559,#18560,#18561,#18562,#18563,#18564,#18565,
#18566,#18567,#18568,#18569,#18570,#18571,#18572,#18573,#18574,#18575,#18576,
#18577),.UNSPECIFIED.,.F.,.F.,(4,2,2,2,2,2,2,2,2,2,2,2,2,4),(0.00065268600767223,
0.0096207910894088,0.0141048436302771,0.0185888961711454,0.0275570012528819,
0.0365251063346185,0.0454932114163551,0.0544613164980917,0.0634294215798282,
0.0723975266615648,0.090333736825038,0.108269946988511,0.126206157151984,
0.144142367315457),.UNSPECIFIED.);
#266=B_SPLINE_CURVE_WITH_KNOTS('',3,(#18586,#18587,#18588,#18589,#18590,
#18591,#18592,#18593,#18594,#18595,#18596,#18597,#18598,#18599,#18600,#18601,
#18602,#18603,#18604,#18605,#18606,#18607,#18608,#18609,#18610,#18611,#18612,
#18613,#18614,#18615,#18616,#18617,#18618,#18619,#18620,#18621,#18622,#18623,
#18624,#18625,#18626,#18627,#18628,#18629,#18630,#18631,#18632,#18633,#18634,
#18635,#18636,#18637,#18638,#18639,#18640,#18641,#18642,#18643,#18644,#18645,
#18646,#18647,#18648,#18649,#18650,#18651,#18652,#18653,#18654,#18655,#18656,
#18657,#18658,#18659,#18660,#18661,#18662,#18663,#18664,#18665,#18666,#18667,
#18668,#18669,#18670),.UNSPECIFIED.,.F.,.F.,(4,3,3,3,3,3,3,3,3,3,3,3,3,
3,3,3,3,3,3,3,3,3,3,3,3,3,3,3,4),(0.,0.0177783686920926,0.0180029436513539,
0.0270066186424758,0.0355567373841852,0.0360116560450794,0.0533351060762777,
0.0540227029497941,0.0711134747683703,0.0720337497834665,0.0810392838872481,
0.0888918434604629,0.0900447880456831,0.0977810278065092,0.099050320587819,
0.106670212152555,0.108055841493459,0.115559396498602,0.117061369410219,
0.121433958055277,0.124448580844648,0.126066766093759,0.128893173017671,
0.130566980042054,0.133337765190694,0.135060883634036,0.139548881847676,
0.141790875480166,0.142226949536741),.UNSPECIFIED.);
#267=B_SPLINE_CURVE_WITH_KNOTS('',3,(#18691,#18692,#18693,#18694,#18695,
#18696,#18697,#18698,#18699,#18700,#18701,#18702,#18703,#18704,#18705,#18706,
#18707,#18708,#18709,#18710,#18711,#18712,#18713,#18714,#18715,#18716,#18717,
#18718,#18719,#18720,#18721,#18722,#18723,#18724,#18725,#18726,#18727,#18728,
#18729,#18730,#18731,#18732,#18733,#18734,#18735,#18736,#18737,#18738,#18739,
#18740,#18741,#18742,#18743,#18744,#18745,#18746,#18747,#18748,#18749,#18750,
#18751,#18752,#18753,#18754,#18755,#18756,#18757,#18758,#18759,#18760,#18761,
#18762,#18763,#18764,#18765,#18766,#18767,#18768,#18769,#18770,#18771,#18772),
 .UNSPECIFIED.,.F.,.F.,(4,3,3,3,3,3,3,3,3,3,3,3,3,3,3,3,3,3,3,3,3,3,3,3,
3,3,3,4),(0.000517800053919739,0.000956159507782921,0.00320697463254193,
0.00771269228342838,0.00944404423079018,0.0134429504552714,0.0139071663192254,
0.0167424870504005,0.0183702884076606,0.0227455403801691,0.0257851780432227,
0.0272965325845311,0.0348279221194363,0.0362227767614015,0.0438706503327037,
0.045149020938272,0.0529133874777611,0.0540752651151424,0.0619560947171763,
0.070998836612136,0.0719277534688833,0.0890842949457832,0.0897802418226242,
0.107169748483184,0.107632730176365,0.125255111030166,0.125485218530106,
0.143337706883847),.UNSPECIFIED.);
#268=B_SPLINE_CURVE_WITH_KNOTS('',3,(#18872,#18873,#18874,#18875,#18876,
#18877,#18878,#18879,#18880,#18881,#18882,#18883,#18884,#18885,#18886,#18887,
#18888,#18889,#18890,#18891,#18892,#18893,#18894,#18895,#18896,#18897,#18898,
#18899,#18900,#18901,#18902,#18903,#18904,#18905,#18906,#18907,#18908,#18909,
#18910,#18911,#18912,#18913,#18914,#18915,#18916,#18917,#18918,#18919,#18920,
#18921,#18922,#18923,#18924,#18925,#18926,#18927,#18928,#18929,#18930,#18931,
#18932,#18933,#18934,#18935,#18936,#18937,#18938),.UNSPECIFIED.,.F.,.F.,
(4,3,3,3,3,3,3,3,3,3,3,3,3,3,3,3,3,3,3,3,3,3,4),(3.24873139256393E-12,0.000789113203271446,
0.000792375749127745,0.00141612050710302,0.00157874172054858,0.00158475149825549,
0.00222253730489919,0.00236930376886044,0.00237712724738323,0.00294445569018658,
0.00316101198412218,0.00316950299651097,0.00395398652820353,0.00396187874563871,
0.00461756528354283,0.00474818189970434,0.00475425449476645,0.0054660318604933,
0.00554328490870971,0.00554663024389419,0.00586525399963526,0.00618286705330126,
0.00633900599302193),.UNSPECIFIED.);
#269=B_SPLINE_CURVE_WITH_KNOTS('',3,(#19047,#19048,#19049,#19050,#19051,
#19052,#19053,#19054,#19055,#19056,#19057,#19058,#19059,#19060,#19061,#19062,
#19063,#19064,#19065,#19066,#19067,#19068,#19069,#19070,#19071,#19072,#19073,
#19074,#19075,#19076,#19077,#19078,#19079,#19080,#19081,#19082,#19083,#19084,
#19085,#19086,#19087,#19088,#19089,#19090,#19091,#19092,#19093,#19094,#19095,
#19096,#19097,#19098,#19099,#19100,#19101,#19102,#19103,#19104,#19105,#19106,
#19107,#19108,#19109,#19110,#19111,#19112,#19113,#19114,#19115,#19116),
 .UNSPECIFIED.,.F.,.F.,(4,3,3,3,3,3,3,3,3,3,3,3,3,3,3,3,3,3,3,3,3,3,3,4),
(0.,0.000792526143918412,0.000795787604514349,0.00142673915028219,0.00158505228783682,
0.00159109328876066,0.00237757843175524,0.00238542369538965,0.00299442831057784,
0.00317010457567365,0.0031785911693371,0.00375515851311093,0.00396263071959206,
0.00397045983119314,0.00448222397781173,0.00475515686351047,0.00476119515944008,
0.00506130515504216,0.0053643750105131,0.00554768300742888,0.00580423226308875,
0.00607222070558002,0.00632304467713367,0.0063402091480713),
 .UNSPECIFIED.);
#270=B_SPLINE_CURVE_WITH_KNOTS('',3,(#19127,#19128,#19129,#19130,#19131,
#19132,#19133,#19134,#19135,#19136,#19137,#19138,#19139,#19140,#19141,#19142,
#19143,#19144,#19145,#19146,#19147,#19148,#19149,#19150),.UNSPECIFIED.,
 .F.,.F.,(4,2,2,2,2,2,2,2,2,2,2,4),(-0.19450411922911,-0.126334189862308,
-0.111286464135786,-0.103050819900779,-0.10157129690467,-0.100782940759509,
-0.100118651209767,-0.0993103301884034,-0.0978953228319982,-0.0918418092473422,
-0.074264450184147,-3.29579807889502E-10),.UNSPECIFIED.);
#271=B_SPLINE_CURVE_WITH_KNOTS('',3,(#19151,#19152,#19153,#19154),
 .UNSPECIFIED.,.F.,.F.,(4,4),(0.,0.000312238933267578),.UNSPECIFIED.);
#272=B_SPLINE_CURVE_WITH_KNOTS('',3,(#19165,#19166,#19167,#19168,#19169,
#19170),.UNSPECIFIED.,.F.,.F.,(4,2,4),(-0.149813019636341,-0.0742119267126466,
0.),.UNSPECIFIED.);
#273=B_SPLINE_CURVE_WITH_KNOTS('',3,(#19172,#19173,#19174,#19175,#19176,
#19177),.UNSPECIFIED.,.F.,.F.,(4,2,4),(-0.154390811946475,-0.0750953953452426,
-9.99999601875023E-7),.UNSPECIFIED.);
#274=B_SPLINE_CURVE_WITH_KNOTS('',3,(#19180,#19181,#19182,#19183,#19184,
#19185),.UNSPECIFIED.,.F.,.F.,(4,2,4),(-0.149813019635849,-0.0742119267123349,
0.),.UNSPECIFIED.);
#275=B_SPLINE_CURVE_WITH_KNOTS('',3,(#19187,#19188,#19189,#19190,#19191,
#19192),.UNSPECIFIED.,.F.,.F.,(4,2,4),(-0.154390811945437,-0.0750948817400542,
-9.99999603170351E-7),.UNSPECIFIED.);
#276=B_SPLINE_CURVE_WITH_KNOTS('',3,(#19195,#19196,#19197,#19198,#19199,
#19200),.UNSPECIFIED.,.F.,.F.,(4,2,4),(-0.149813019635709,-0.0742114219215882,
0.),.UNSPECIFIED.);
#277=B_SPLINE_CURVE_WITH_KNOTS('',3,(#19202,#19203,#19204,#19205,#19206,
#19207),.UNSPECIFIED.,.F.,.F.,(4,2,4),(-0.154390811947745,-0.0750953953455204,
-9.99999601236645E-7),.UNSPECIFIED.);
#278=B_SPLINE_CURVE_WITH_KNOTS('',3,(#19210,#19211,#19212,#19213,#19214,
#19215),.UNSPECIFIED.,.F.,.F.,(4,2,4),(-0.149813019636192,-0.0742119267126041,
0.),.UNSPECIFIED.);
#279=B_SPLINE_CURVE_WITH_KNOTS('',3,(#19217,#19218,#19219,#19220,#19221,
#19222),.UNSPECIFIED.,.F.,.F.,(4,2,4),(-0.154390811946182,-0.0750948817402176,
-9.99999601734471E-7),.UNSPECIFIED.);
#280=B_SPLINE_CURVE_WITH_KNOTS('',3,(#19225,#19226,#19227,#19228,#19229,
#19230),.UNSPECIFIED.,.F.,.F.,(4,2,4),(-0.149813019636222,-0.0742119267126633,
0.),.UNSPECIFIED.);
#281=B_SPLINE_CURVE_WITH_KNOTS('',3,(#19232,#19233,#19234,#19235,#19236,
#19237),.UNSPECIFIED.,.F.,.F.,(4,2,4),(-0.154390811946885,-0.0750948817403378,
-9.99999602331216E-7),.UNSPECIFIED.);
#282=B_SPLINE_CURVE_WITH_KNOTS('',3,(#19240,#19241,#19242,#19243,#19244,
#19245),.UNSPECIFIED.,.F.,.F.,(4,2,4),(-0.149813019636188,-0.0742114219217932,
0.),.UNSPECIFIED.);
#283=B_SPLINE_CURVE_WITH_KNOTS('',3,(#19247,#19248,#19249,#19250,#19251,
#19252),.UNSPECIFIED.,.F.,.F.,(4,2,4),(-0.154390811947138,-0.0750948817403358,
-9.99999601842204E-7),.UNSPECIFIED.);
#284=B_SPLINE_CURVE_WITH_KNOTS('',3,(#19255,#19256,#19257,#19258,#19259,
#19260),.UNSPECIFIED.,.F.,.F.,(4,2,4),(-0.1498130196363,-0.0742119267124509,
0.),.UNSPECIFIED.);
#285=B_SPLINE_CURVE_WITH_KNOTS('',3,(#19262,#19263,#19264,#19265,#19266,
#19267),.UNSPECIFIED.,.F.,.F.,(4,2,4),(-0.1167939430675,-0.0559485367490526,
-9.9999970383513E-7),.UNSPECIFIED.);
#286=B_SPLINE_CURVE_WITH_KNOTS('',3,(#19283,#19284,#19285,#19286,#19287,
#19288),.UNSPECIFIED.,.F.,.F.,(4,2,4),(9.99999616665374E-7,0.0121034221554694,
0.0242049584783662),.UNSPECIFIED.);
#287=B_SPLINE_CURVE_WITH_KNOTS('',3,(#19289,#19290,#19291,#19292,#19293,
#19294,#19295,#19296,#19297,#19298,#19299,#19300,#19301,#19302),
 .UNSPECIFIED.,.F.,.F.,(4,2,2,2,2,2,4),(0.,0.0409644441214631,0.0887268040598564,
0.0955303651869036,0.109712942382492,0.168590020103833,0.219688229784175),
 .UNSPECIFIED.);
#288=B_SPLINE_CURVE_WITH_KNOTS('',3,(#19304,#19305,#19306,#19307,#19308,
#19309,#19310,#19311,#19312,#19313,#19314,#19315,#19316,#19317,#19318,#19319,
#19320,#19321,#19322,#19323,#19324,#19325,#19326,#19327,#19328,#19329,#19330,
#19331),.UNSPECIFIED.,.F.,.F.,(4,2,2,2,2,2,2,2,2,2,2,2,2,4),(-0.195818704088962,
-0.143355144115657,-0.110356347530556,-0.0979570470431692,-0.090786108819357,
-0.0895445881165381,-0.0888007558059985,-0.0882295747566688,-0.087617885883006,
-0.0866600191131884,-0.0836895532525834,-0.0674705918142883,-0.0363980900813506,
-9.99670535101194E-7),.UNSPECIFIED.);
#289=B_SPLINE_CURVE_WITH_KNOTS('',3,(#19345,#19346,#19347,#19348,#19349,
#19350,#19351,#19352,#19353,#19354,#19355,#19356,#19357,#19358,#19359,#19360,
#19361,#19362,#19363),.UNSPECIFIED.,.F.,.F.,(4,3,3,3,3,3,4),(5.81811766227498E-12,
0.000713015175406057,0.00148279719273555,0.0017944978017605,0.00183065943066078,
0.00325218021980356,0.00366131886132156),.UNSPECIFIED.);
#290=B_SPLINE_CURVE_WITH_KNOTS('',3,(#19365,#19366,#19367,#19368,#19369,
#19370,#19371,#19372,#19373,#19374,#19375,#19376,#19377,#19378,#19379,#19380,
#19381,#19382,#19383,#19384,#19385,#19386,#19387,#19388,#19389),
 .UNSPECIFIED.,.F.,.F.,(4,3,3,3,3,3,3,3,4),(0.,0.000282845373659893,0.000537791840235127,
0.000538908034209594,0.000878730315925117,0.00107558368047025,0.00107834483611328,
0.00176407748649149,0.00215116736094051),.UNSPECIFIED.);
#291=B_SPLINE_CURVE_WITH_KNOTS('',3,(#19390,#19391,#19392,#19393),
 .UNSPECIFIED.,.F.,.F.,(4,4),(0.,6.29047409436179E-5),.UNSPECIFIED.);
#292=B_SPLINE_CURVE_WITH_KNOTS('',3,(#19395,#19396,#19397,#19398),
 .UNSPECIFIED.,.F.,.F.,(4,4),(0.,6.29047409436508E-5),.UNSPECIFIED.);
#293=B_SPLINE_CURVE_WITH_KNOTS('',3,(#19400,#19401,#19402,#19403,#19404,
#19405,#19406,#19407,#19408,#19409,#19410,#19411,#19412,#19413,#19414,#19415,
#19416,#19417,#19418,#19419,#19420,#19421,#19422,#19423,#19424),
 .UNSPECIFIED.,.F.,.F.,(4,3,3,3,3,3,3,3,4),(0.,0.000685296287045248,0.00107213984073947,
0.00107489923933792,0.00141450527734773,0.0016112333753157,0.0016123488590069,
0.00191262071533291,0.00214979847867587),.UNSPECIFIED.);
#294=B_SPLINE_CURVE_WITH_KNOTS('',3,(#19425,#19426,#19427,#19428,#19429,
#19430,#19431,#19432,#19433,#19434,#19435,#19436,#19437,#19438,#19439,#19440,
#19441,#19442,#19443),.UNSPECIFIED.,.F.,.F.,(4,3,3,3,3,3,4),(0.,0.000899413916680641,
0.00174431342931246,0.00179882783336128,0.00256218526438471,0.00331004957902007,
0.00359765561291069),.UNSPECIFIED.);
#295=B_SPLINE_CURVE_WITH_KNOTS('',3,(#19448,#19449,#19450,#19451,#19452,
#19453),.UNSPECIFIED.,.F.,.F.,(4,2,4),(-0.0144436412707524,-0.00699620646723456,
-6.60336511512649E-9),.UNSPECIFIED.);
#296=B_SPLINE_CURVE_WITH_KNOTS('',3,(#19455,#19456,#19457,#19458,#19459,
#19460),.UNSPECIFIED.,.F.,.F.,(4,2,4),(-0.0144503347921917,-0.00745133852662736,
-1.00730609309307E-6),.UNSPECIFIED.);
#297=B_SPLINE_CURVE_WITH_KNOTS('',3,(#19475,#19476,#19477,#19478),
 .UNSPECIFIED.,.F.,.F.,(4,4),(0.,0.00173428636340849),.UNSPECIFIED.);
#298=B_SPLINE_CURVE_WITH_KNOTS('',3,(#19480,#19481,#19482,#19483,#19484,
#19485,#19486,#19487,#19488,#19489,#19490,#19491,#19492,#19493,#19494,#19495,
#19496,#19497,#19498,#19499,#19500,#19501,#19502,#19503,#19504,#19505,#19506,
#19507,#19508,#19509,#19510,#19511,#19512,#19513,#19514,#19515,#19516,#19517,
#19518,#19519,#19520,#19521,#19522,#19523,#19524,#19525),.UNSPECIFIED.,
 .F.,.F.,(4,3,3,3,3,3,3,3,3,3,3,3,3,3,3,4),(0.,9.12787148238181E-5,0.000183921671662766,
0.000256351757877802,0.000311479035290493,0.000328781844092839,0.000439888590826784,
0.000526050950548542,0.000530451527395148,0.000625111740468468,0.000657563688185677,
0.000756198241413529,0.000800848465156635,0.000892918501575997,0.000983117535815826,
0.00105210190109708),.UNSPECIFIED.);
#299=B_SPLINE_CURVE_WITH_KNOTS('',3,(#19533,#19534,#19535,#19536,#19537,
#19538,#19539,#19540,#19541,#19542,#19543,#19544,#19545,#19546,#19547,#19548,
#19549,#19550,#19551,#19552,#19553,#19554,#19555,#19556,#19557,#19558,#19559,
#19560,#19561,#19562,#19563,#19564,#19565,#19566,#19567,#19568,#19569,#19570,
#19571,#19572,#19573,#19574,#19575,#19576,#19577,#19578,#19579,#19580,#19581),
 .UNSPECIFIED.,.F.,.F.,(4,3,3,3,3,3,3,3,3,3,3,3,3,3,3,3,4),(0.,0.000112411075416676,
0.00022668855713591,0.000256939338114826,0.000281905681799926,0.00038239262866012,
0.000399717078062952,0.000493967094647472,0.000528483381613059,0.000532956104083936,
0.000646963423007012,0.00066619513010492,0.000766124399620658,0.000822145470081397,
0.000917119711214598,0.00101032641648309,0.00106591220816787),
 .UNSPECIFIED.);
#300=B_SPLINE_CURVE_WITH_KNOTS('',3,(#19583,#19584,#19585,#19586),
 .UNSPECIFIED.,.F.,.F.,(4,4),(0.,0.00173428636340849),.UNSPECIFIED.);
#301=B_SPLINE_CURVE_WITH_KNOTS('',3,(#19591,#19592,#19593,#19594,#19595,
#19596,#19597,#19598,#19599,#19600,#19601,#19602,#19603,#19604),
 .UNSPECIFIED.,.F.,.F.,(4,2,2,2,2,2,4),(-0.0976421838858201,-0.084189955512187,
-0.0697581457509971,-0.0491108456698284,-0.0297735319812699,-0.0141869021647831,
0.),.UNSPECIFIED.);
#302=B_SPLINE_CURVE_WITH_KNOTS('',3,(#19609,#19610,#19611,#19612,#19613,
#19614),.UNSPECIFIED.,.F.,.F.,(4,2,4),(-0.0567997771842775,-0.0284184953580656,
-1.01442404849064E-6),.UNSPECIFIED.);
#303=B_SPLINE_CURVE_WITH_KNOTS('',3,(#19663,#19664,#19665,#19666,#19667,
#19668,#19669,#19670,#19671,#19672,#19673,#19674,#19675,#19676),
 .UNSPECIFIED.,.F.,.F.,(4,2,2,2,2,2,4),(0.,0.0141504479466231,0.0296944189662601,
0.0490192876277638,0.0696539086346055,0.0841403129979988,0.0976417165566767),
 .UNSPECIFIED.);
#304=B_SPLINE_CURVE_WITH_KNOTS('',3,(#19715,#19716,#19717,#19718,#19719,
#19720),.UNSPECIFIED.,.F.,.F.,(4,2,4),(1.01442403287893E-6,0.0284184953584133,
0.0567997771849387),.UNSPECIFIED.);
#305=B_SPLINE_CURVE_WITH_KNOTS('',3,(#19724,#19725,#19726,#19727,#19728,
#19729,#19730,#19731,#19732,#19733),.UNSPECIFIED.,.F.,.F.,(4,3,3,4),(4.30118003192922E-9,
0.00131474961221221,0.00268758862115831,0.0031904227463795),
 .UNSPECIFIED.);
#306=B_SPLINE_CURVE_WITH_KNOTS('',3,(#19738,#19739,#19740,#19741,#19742,
#19743,#19744,#19745,#19746,#19747),.UNSPECIFIED.,.F.,.F.,(4,3,3,4),(0.,
0.00137283900902173,0.00187567313416777,0.00319041844519952),
 .UNSPECIFIED.);
#307=B_SPLINE_CURVE_WITH_KNOTS('',3,(#19790,#19791,#19792,#19793,#19794,
#19795,#19796,#19797,#19798,#19799,#19800,#19801,#19802,#19803,#19804,#19805,
#19806,#19807,#19808,#19809,#19810,#19811,#19812,#19813,#19814,#19815,#19816,
#19817,#19818,#19819,#19820),.UNSPECIFIED.,.F.,.F.,(4,3,3,3,3,3,3,3,3,3,
4),(0.,0.000157386647060973,0.000332445535114511,0.000489094642209349,0.000494201771608867,
0.000710151345833458,0.000951984363272296,0.000988403543217735,0.000989925971234007,
0.00149956601242565,0.00197680708643547),.UNSPECIFIED.);
#308=B_SPLINE_CURVE_WITH_KNOTS('',3,(#19826,#19827,#19828,#19829,#19830,
#19831,#19832,#19833,#19834,#19835,#19836,#19837,#19838,#19839,#19840,#19841,
#19842,#19843,#19844,#19845,#19846,#19847,#19848,#19849,#19850,#19851,#19852,
#19853,#19854,#19855,#19856),.UNSPECIFIED.,.F.,.F.,(4,3,3,3,3,3,3,3,3,3,
4),(0.,0.000509513490104227,0.000986636057298634,0.000988158107272369,0.00123519763409046,
0.00145109358469587,0.00148223716090855,0.00148734302212855,0.00166747975270183,
0.00182718054780211,0.00197631621454474),.UNSPECIFIED.);
#309=B_SPLINE_CURVE_WITH_KNOTS('',3,(#19979,#19980,#19981,#19982,#19983,
#19984),.UNSPECIFIED.,.F.,.F.,(4,2,4),(-0.107519161292799,-0.0637323978923038,
0.),.UNSPECIFIED.);
#310=B_SPLINE_CURVE_WITH_KNOTS('',3,(#32348,#32349,#32350,#32351,#32352,
#32353,#32354,#32355,#32356,#32357),.UNSPECIFIED.,.F.,.F.,(4,2,2,2,4),(-0.317022884646079,
-0.305729538758937,-0.18510534189066,-0.0921237868962644,-1.00000008007584E-6),
 .UNSPECIFIED.);
#311=B_SPLINE_CURVE_WITH_KNOTS('',3,(#32363,#32364,#32365,#32366,#32367,
#32368,#32369,#32370,#32371,#32372,#32373,#32374,#32375,#32376,#32377,#32378,
#32379,#32380,#32381,#32382,#32383,#32384,#32385,#32386,#32387,#32388,#32389,
#32390,#32391,#32392,#32393,#32394,#32395,#32396,#32397,#32398),
 .UNSPECIFIED.,.F.,.F.,(4,2,2,2,2,2,2,2,2,2,2,2,2,2,2,2,2,4),(-2.20877752486386,
-2.1921017198068,-2.0724399317334,-1.95706912003883,-1.83729284877479,-1.72182784454118,
-1.60193535202522,-1.48637284172353,-1.36636241511554,-1.25069926792504,
-1.13056922486976,-1.01480248488051,-0.894551178068988,-0.778678056364855,
-0.658303877405628,-0.54232174411607,-0.421823126741146,-0.317022884646079),
 .UNSPECIFIED.);
#312=B_SPLINE_CURVE_WITH_KNOTS('',3,(#32401,#32402,#32403,#32404,#32405,
#32406,#32407,#32408,#32409,#32410,#32411,#32412,#32413,#32414,#32415,#32416,
#32417,#32418,#32419,#32420,#32421,#32422,#32423,#32424,#32425,#32426,#32427,
#32428,#32429,#32430,#32431,#32432),.UNSPECIFIED.,.F.,.F.,(4,2,2,2,2,2,
2,2,2,2,2,2,2,2,2,4),(-56.1018496897495,-56.020261169572,-55.9400137990114,
-55.8174844812794,-55.6902240350637,-55.5678472298567,-55.4407451859001,
-55.3185207025299,-55.1915768628461,-55.0695045107994,-54.9427186775888,
-54.8207982665224,-54.6941702421669,-54.5724015819026,-54.4459311689611,
-54.4423592036668),.UNSPECIFIED.);
#313=B_SPLINE_CURVE_WITH_KNOTS('',3,(#32437,#32438,#32439,#32440,#32441,
#32442,#32443,#32444,#32445,#32446,#32447,#32448,#32449,#32450,#32451,#32452,
#32453,#32454,#32455,#32456,#32457,#32458,#32459,#32460,#32461,#32462,#32463,
#32464,#32465,#32466,#32467,#32468,#32469,#32470,#32471,#32472),
 .UNSPECIFIED.,.F.,.F.,(4,2,2,2,2,2,2,2,2,2,2,2,2,2,2,2,2,4),(-4.09054085430461,
-4.06552527473558,-3.94671600483119,-3.83195524526434,-3.71304546474063,
-3.59822439924299,-3.4792124302724,-3.36432605817047,-3.24521018614115,
-3.13025373205913,-3.01103221426206,-2.89600112622998,-2.77667220060433,
-2.66156214681765,-2.54212404054857,-2.42693090497668,-2.30738184277471,
-2.20877752486386),.UNSPECIFIED.);
#314=B_SPLINE_CURVE_WITH_KNOTS('',3,(#32473,#32474,#32475,#32476,#32477,
#32478,#32479,#32480,#32481,#32482,#32483,#32484,#32485,#32486,#32487,#32488,
#32489,#32490,#32491,#32492,#32493,#32494,#32495,#32496,#32497,#32498,#32499,
#32500,#32501,#32502,#32503,#32504,#32505,#32506,#32507,#32508),
 .UNSPECIFIED.,.F.,.F.,(4,2,2,2,2,2,2,2,2,2,2,2,2,2,2,2,2,4),(-54.4423592036668,
-54.3243140694799,-54.198001070683,-54.0765353421194,-53.9503795603631,
-53.8290650129986,-53.7030662513386,-53.5819026955948,-53.4560607572401,
-53.3350480036717,-53.2093626919771,-53.0885005512639,-52.9629716697227,
-52.8422599526612,-52.7168873048974,-52.5963258223919,-52.4711092121511,
-52.4675692868415),.UNSPECIFIED.);
#315=B_SPLINE_CURVE_WITH_KNOTS('',3,(#32513,#32514,#32515,#32516,#32517,
#32518,#32519,#32520,#32521,#32522,#32523,#32524,#32525,#32526,#32527,#32528,
#32529,#32530,#32531,#32532,#32533,#32534,#32535,#32536,#32537,#32538,#32539,
#32540,#32541,#32542,#32543,#32544,#32545,#32546,#32547,#32548),
 .UNSPECIFIED.,.F.,.F.,(4,2,2,2,2,2,2,2,2,2,2,2,2,2,2,2,2,4),(-5.96600277725799,
-5.92915238724561,-5.81109356976484,-5.6966089801729,-5.57846094519294,
-5.46396379271469,-5.34572536991432,-5.23120900895501,-5.11287895829174,
-4.99833691252241,-4.87991392178187,-4.76533989948019,-4.64682258434647,
-4.53221049115057,-4.41359739749494,-4.29894134662589,-4.18023095468391,
-4.09054085430461),.UNSPECIFIED.);
#316=B_SPLINE_CURVE_WITH_KNOTS('',3,(#32549,#32550,#32551,#32552,#32553,
#32554,#32555,#32556,#32557,#32558,#32559,#32560,#32561,#32562,#32563,#32564,
#32565,#32566,#32567,#32568,#32569,#32570,#32571,#32572,#32573,#32574,#32575,
#32576,#32577,#32578,#32579,#32580,#32581,#32582,#32583,#32584),
 .UNSPECIFIED.,.F.,.F.,(4,2,2,2,2,2,2,2,2,2,2,2,2,2,2,2,2,4),(-52.4675692868415,
-52.350697775204,-52.2256370063445,-52.1053754260461,-51.980470302529,-51.8603583900464,
-51.7356087159248,-51.6156462824901,-51.4910518618977,-51.3712387187952,
-51.2467993559344,-51.1271353144871,-51.0028508136156,-50.8833356851705,
-50.7592058505875,-50.6398394464999,-50.5158640825307,-50.5123532699249),
 .UNSPECIFIED.);
#317=B_SPLINE_CURVE_WITH_KNOTS('',3,(#32589,#32590,#32591,#32592,#32593,
#32594,#32595,#32596,#32597,#32598,#32599,#32600,#32601,#32602,#32603,#32604,
#32605,#32606,#32607,#32608,#32609,#32610,#32611,#32612,#32613,#32614,#32615,
#32616,#32617,#32618,#32619,#32620,#32621,#32622,#32623,#32624),
 .UNSPECIFIED.,.F.,.F.,(4,2,2,2,2,2,2,2,2,2,2,2,2,2,2,2,2,4),(-7.83850150145777,
-7.78679682633793,-7.6694148644393,-7.55477823480178,-7.4373151677535,-7.32272259398481,
-7.20517736951867,-7.09062168679696,-6.97299330726751,-6.85846731695973,
-6.74075481453558,-6.62625131506633,-6.508453728985,-6.39396554585313,-6.27608190217634,
-6.16160191669192,-6.04363121088209,-5.96600277725799),.UNSPECIFIED.);
#318=B_SPLINE_CURVE_WITH_KNOTS('',3,(#32625,#32626,#32627,#32628,#32629,
#32630,#32631,#32632,#32633,#32634,#32635,#32636,#32637,#32638,#32639,#32640,
#32641,#32642,#32643,#32644,#32645,#32646,#32647,#32648,#32649,#32650,#32651,
#32652,#32653,#32654,#32655,#32656,#32657,#32658,#32659,#32660),
 .UNSPECIFIED.,.F.,.F.,(4,2,2,2,2,2,2,2,2,2,2,2,2,2,2,2,2,4),(-50.5123532699249,
-50.3966462141476,-50.2728251251281,-50.1537556037699,-50.0300885940287,
-49.9111672309698,-49.7876541048099,-49.6688807112583,-49.5455212729371,
-49.4268956600118,-49.3036897137199,-49.1852116924269,-49.0621590422651,
-48.9438284234721,-48.8209288734267,-48.7027454678352,-48.5799988217518,
-48.5765122072365),.UNSPECIFIED.);
#319=B_SPLINE_CURVE_WITH_KNOTS('',3,(#32665,#32666,#32667,#32668,#32669,
#32670,#32671,#32672,#32673,#32674,#32675,#32676,#32677,#32678,#32679,#32680,
#32681,#32682,#32683,#32684,#32685,#32686,#32687,#32688,#32689,#32690,#32691,
#32692,#32693,#32694,#32695,#32696,#32697,#32698,#32699,#32700),
 .UNSPECIFIED.,.F.,.F.,(4,2,2,2,2,2,2,2,2,2,2,2,2,2,2,2,2,4),(-9.71034922447295,
-9.64303824023506,-9.52555324115343,-9.41092911859412,-9.29352551362348,
-9.17885213083062,-9.06152881110041,-8.94679913569492,-8.82955489151035,
-8.71476200974326,-8.59759550315609,-8.48271269177544,-8.36556678591869,
-8.25075580545369,-8.13353254602213,-8.01878660157305,-7.90148461160325,
-7.83850150145777),.UNSPECIFIED.);
#320=B_SPLINE_CURVE_WITH_KNOTS('',3,(#32701,#32702,#32703,#32704,#32705,
#32706,#32707,#32708,#32709,#32710,#32711,#32712,#32713,#32714,#32715,#32716,
#32717,#32718,#32719,#32720,#32721,#32722,#32723,#32724,#32725,#32726,#32727,
#32728,#32729,#32730,#32731,#32732,#32733,#32734,#32735,#32736),
 .UNSPECIFIED.,.F.,.F.,(4,2,2,2,2,2,2,2,2,2,2,2,2,2,2,2,2,4),(-48.5765122072365,
-48.4619624398676,-48.3393685014224,-48.2214789535238,-48.099037526194,
-47.9812946222979,-47.8590055093283,-47.7414090591536,-47.6192720635222,
-47.5018218764501,-47.3798368008302,-47.2625326858626,-47.1406993325827,
-47.0235410982965,-46.9018592692971,-46.7848467237956,-46.6633162205828,
-46.6598453653102),.UNSPECIFIED.);
#321=B_SPLINE_CURVE_WITH_KNOTS('',3,(#32741,#32742,#32743,#32744,#32745,
#32746,#32747,#32748,#32749,#32750,#32751,#32752,#32753,#32754,#32755,#32756,
#32757,#32758,#32759,#32760,#32761,#32762,#32763,#32764,#32765,#32766,#32767,
#32768,#32769,#32770,#32771,#32772,#32773,#32774,#32775,#32776),
 .UNSPECIFIED.,.F.,.F.,(4,2,2,2,2,2,2,2,2,2,2,2,2,2,2,2,2,4),(-11.5834064169039,
-11.5020464607245,-11.383874304121,-11.2693870023825,-11.1513043704658,
-11.0368246707749,-10.9188304411037,-10.8043514485982,-10.6864445575209,
-10.5719592629818,-10.4541386951801,-10.339639999561,-10.2219047744793,
-10.1073855154856,-9.98973467070285,-9.87518765111858,-9.75762022283361,
-9.71034922447295),.UNSPECIFIED.);
#322=B_SPLINE_CURVE_WITH_KNOTS('',3,(#32777,#32778,#32779,#32780,#32781,
#32782,#32783,#32784,#32785,#32786,#32787,#32788,#32789,#32790,#32791,#32792,
#32793,#32794,#32795,#32796,#32797,#32798,#32799,#32800,#32801,#32802,#32803,
#32804,#32805,#32806,#32807,#32808,#32809,#32810,#32811,#32812),
 .UNSPECIFIED.,.F.,.F.,(4,2,2,2,2,2,2,2,2,2,2,2,2,2,2,2,2,4),(-46.6598453653102,
-46.5464491714436,-46.4250697950394,-46.3083480492585,-46.1871196001471,
-46.0705429640784,-45.9494652421493,-45.8330335214402,-45.7121063259267,
-45.5958193254485,-45.4750424548615,-45.3588999786348,-45.2382732306923,
-45.1222750818075,-45.0017982533583,-44.8859442338891,-44.765617120832,
-44.7621473413414),.UNSPECIFIED.);
#323=B_SPLINE_CURVE_WITH_KNOTS('',3,(#32817,#32818,#32819,#32820,#32821,
#32822,#32823,#32824,#32825,#32826,#32827,#32828,#32829,#32830,#32831,#32832,
#32833,#32834,#32835,#32836,#32837,#32838,#32839,#32840,#32841,#32842,#32843,
#32844,#32845,#32846,#32847,#32848,#32849,#32850,#32851,#32852),
 .UNSPECIFIED.,.F.,.F.,(4,2,2,2,2,2,2,2,2,2,2,2,2,2,2,2,2,4),(-13.4602816584202,
-13.3677504690497,-13.2488134515995,-13.1340370217358,-13.0152009606675,
-12.9004810337686,-12.7817442835188,-12.6670754689181,-12.5484364348836,
-12.4338131199453,-12.3152702656808,-12.200686620704,-12.0822384740026,
-11.9676884593812,-11.8493336169002,-11.7348109926818,-11.6165481227706,
-11.5834064169039),.UNSPECIFIED.);
#324=B_SPLINE_CURVE_WITH_KNOTS('',3,(#32853,#32854,#32855,#32856,#32857,
#32858,#32859,#32860,#32861,#32862,#32863,#32864,#32865,#32866,#32867,#32868,
#32869,#32870,#32871,#32872,#32873,#32874,#32875,#32876,#32877,#32878,#32879,
#32880,#32881,#32882,#32883,#32884,#32885,#32886,#32887,#32888),
 .UNSPECIFIED.,.F.,.F.,(4,2,2,2,2,2,2,2,2,2,2,2,2,2,2,2,2,4),(-44.7621473413414,
-44.6499070317433,-44.5297294289392,-44.414163069988,-44.2941347711661,
-44.1787119407951,-44.058832738453,-43.9435532336761,-43.8238229189713,
-43.7086865352514,-43.5891048978864,-43.4741114290031,-43.3546782571008,
-43.239827495009,-43.1205425749804,-43.0058343096585,-42.8866974260598,
-42.8832029855023),.UNSPECIFIED.);
#325=B_SPLINE_CURVE_WITH_KNOTS('',3,(#32893,#32894,#32895,#32896,#32897,
#32898,#32899,#32900,#32901,#32902,#32903,#32904,#32905,#32906,#32907,#32908,
#32909,#32910,#32911,#32912,#32913,#32914,#32915,#32916,#32917,#32918,#32919,
#32920,#32921,#32922,#32923,#32924,#32925,#32926,#32927,#32928),
 .UNSPECIFIED.,.F.,.F.,(4,2,2,2,2,2,2,2,2,2,2,2,2,2,2,2,2,4),(-15.3445125192805,
-15.2439072626969,-15.1240999953518,-15.0087042601519,-14.8890119441516,
-14.773707856193,-14.6541287387574,-14.5389126503526,-14.4194449642385,
-14.3043130251781,-14.1849549957844,-14.0699031470151,-13.9506530000678,
-13.8356769681113,-13.716532937833,-13.601628230118,-13.4825885677557,-13.4602816584202),
 .UNSPECIFIED.);
#326=B_SPLINE_CURVE_WITH_KNOTS('',3,(#32929,#32930,#32931,#32932,#32933,
#32934,#32935,#32936,#32937,#32938,#32939,#32940,#32941,#32942,#32943,#32944,
#32945,#32946,#32947,#32948,#32949,#32950,#32951,#32952,#32953,#32954,#32955,
#32956,#32957,#32958,#32959,#32960,#32961,#32962,#32963,#32964),
 .UNSPECIFIED.,.F.,.F.,(4,2,2,2,2,2,2,2,2,2,2,2,2,2,2,2,2,4),(-42.8832029855023,
-42.7721314453461,-42.6531423807262,-42.5387184701442,-42.4198770048811,
-42.3055949474507,-42.1869008595761,-42.072760435612,-41.9542135006233,
-41.8402144875176,-41.7218144781773,-41.6079566501668,-41.4897033362861,
-41.3759864642018,-41.2578796124106,-41.1443034634091,-41.026342836909,
-41.0227784649616),.UNSPECIFIED.);
#327=B_SPLINE_CURVE_WITH_KNOTS('',3,(#32969,#32970,#32971,#32972,#32973,
#32974,#32975,#32976,#32977,#32978,#32979,#32980,#32981,#32982,#32983,#32984,
#32985,#32986,#32987,#32988,#32989,#32990,#32991,#32992,#32993,#32994,#32995,
#32996,#32997,#32998,#32999,#33000,#33001,#33002,#33003,#33004),
 .UNSPECIFIED.,.F.,.F.,(4,2,2,2,2,2,2,2,2,2,2,2,2,2,2,2,2,4),(-17.239659277801,
-17.1263645119701,-17.012759266358,-16.8965209759557,-16.7758624329729,
-16.6597385709917,-16.5392063880205,-16.4231946561967,-16.3027873240138,
-16.1868852828097,-16.066601246905,-15.9508063077464,-15.8306439707352,
-15.7149533881291,-15.594911112786,-15.4793219763771,-15.3593980893255,
-15.3445125192805),.UNSPECIFIED.);
#328=B_SPLINE_CURVE_WITH_KNOTS('',3,(#33005,#33006,#33007,#33008,#33009,
#33010,#33011,#33012,#33013,#33014,#33015,#33016,#33017,#33018,#33019,#33020,
#33021,#33022,#33023,#33024,#33025,#33026,#33027,#33028,#33029,#33030,#33031,
#33032,#33033,#33034,#33035,#33036,#33037,#33038,#33039,#33040),
 .UNSPECIFIED.,.F.,.F.,(4,2,2,2,2,2,2,2,2,2,2,2,2,2,2,2,2,4),(-41.0227784649616,
-40.912907174184,-40.7950925324838,-40.6817971149564,-40.5641282135893,
-40.4509727955753,-40.333449385797,-40.2204337166497,-40.1030555451148,
-39.9901793688419,-39.8729461772583,-39.7602092321103,-39.6431207568703,
-39.5305227748983,-39.4135787466845,-39.3011194532662,-39.1843195966306,
-39.1806055994443),.UNSPECIFIED.);
#329=B_SPLINE_CURVE_WITH_KNOTS('',3,(#33045,#33046,#33047,#33048,#33049,
#33050,#33051,#33052,#33053,#33054,#33055,#33056,#33057,#33058,#33059,#33060,
#33061,#33062,#33063,#33064,#33065,#33066,#33067,#33068,#33069,#33070,#33071,
#33072,#33073,#33074,#33075,#33076,#33077,#33078,#33079,#33080),
 .UNSPECIFIED.,.F.,.F.,(4,2,2,2,2,2,2,2,2,2,2,2,2,2,2,2,2,4),(-1.8864038091393,
-1.88297644722096,-1.76336400027372,-1.64819816326404,-1.52843681680261,
-1.41312762991872,-1.29321718601239,-1.17776445769835,-1.05770471902055,
-0.942108258372344,-0.821899028143226,-0.706158644847652,-0.585799726779994,
-0.469915231058453,-0.349406429307703,-0.233377631863377,-0.116663456726142,
-1.00000007918766E-6),.UNSPECIFIED.);
#330=B_SPLINE_CURVE_WITH_KNOTS('',3,(#33081,#33082,#33083,#33084,#33085,
#33086,#33087,#33088,#33089,#33090,#33091,#33092,#33093,#33094,#33095,#33096,
#33097,#33098,#33099,#33100,#33101,#33102,#33103,#33104,#33105,#33106,#33107,
#33108,#33109,#33110,#33111,#33112,#33113,#33114,#33115,#33116),
 .UNSPECIFIED.,.F.,.F.,(4,2,2,2,2,2,2,2,2,2,2,2,2,2,2,2,2,4),(-39.1806055994443,
-39.0719987099611,-38.9553427428763,-38.8431599734215,-38.726647606802,
-38.6146026567122,-38.4982335939045,-38.3863261563847,-38.2701000926236,
-38.1583298512582,-38.0422464730891,-37.9306131011166,-37.8146720857803,
-37.7031752453158,-37.5873762600955,-37.4760156012962,-37.360358302823,
-37.3563546200977),.UNSPECIFIED.);
#331=B_SPLINE_CURVE_WITH_KNOTS('',3,(#33121,#33122,#33123,#33124,#33125,
#33126,#33127,#33128,#33129,#33130,#33131,#33132,#33133,#33134,#33135,#33136,
#33137,#33138,#33139,#33140,#33141,#33142,#33143,#33144,#33145,#33146,#33147,
#33148,#33149,#33150,#33151,#33152,#33153,#33154,#33155,#33156),
 .UNSPECIFIED.,.F.,.F.,(4,2,2,2,2,2,2,2,2,2,2,2,2,2,2,2,2,4),(-3.75416502035407,
-3.75072999190081,-3.6323014575776,-3.51827536100683,-3.39969954076099,
-3.28553165907193,-3.16680834748475,-3.05249848111017,-2.93362747400919,
-2.81917542471142,-2.70015651906918,-2.58556208983264,-2.46639508367228,
-2.35165807860358,-2.23234277091081,-2.11746299514582,-1.99799918578683,
-1.8864038091393),.UNSPECIFIED.);
#332=B_SPLINE_CURVE_WITH_KNOTS('',3,(#33157,#33158,#33159,#33160,#33161,
#33162,#33163,#33164,#33165,#33166,#33167,#33168,#33169,#33170,#33171,#33172,
#33173,#33174,#33175,#33176,#33177,#33178,#33179,#33180,#33181,#33182,#33183,
#33184,#33185,#33186,#33187,#33188,#33189,#33190,#33191,#33192),
 .UNSPECIFIED.,.F.,.F.,(4,2,2,2,2,2,2,2,2,2,2,2,2,2,2,2,2,4),(-37.3563546200977,
-37.249133462993,-37.1336174965104,-37.0225280991403,-36.9071530977245,
-36.796198751462,-36.6809643351962,-36.5701446327417,-36.4550504078441,
-36.3443649247666,-36.2294104826689,-36.1188587761375,-36.0040436925138,
-35.8936252999371,-35.7789491336822,-35.6686635712511,-35.554125863407,
-35.5495875005638),.UNSPECIFIED.);
#333=B_SPLINE_CURVE_WITH_KNOTS('',3,(#33197,#33198,#33199,#33200,#33201,
#33202,#33203,#33204,#33205,#33206,#33207,#33208,#33209,#33210,#33211,#33212,
#33213,#33214,#33215,#33216,#33217,#33218,#33219,#33220,#33221,#33222,#33223,
#33224,#33225,#33226,#33227,#33228,#33229,#33230,#33231,#33232),
 .UNSPECIFIED.,.F.,.F.,(4,2,2,2,2,2,2,2,2,2,2,2,2,2,2,2,2,4),(-5.60348486335477,
-5.60001012322833,-5.48275229191451,-5.3698530900914,-5.2524496759028,-5.1394103491365,
-5.02186113203936,-4.90868146518021,-4.79098622750961,-4.67766600793584,
-4.55982453421918,-4.44636355164717,-4.32837562843943,-4.21477367474718,
-4.09663909047685,-3.98289595953924,-3.86461450436494,-3.75416502035407),
 .UNSPECIFIED.);
#334=B_SPLINE_CURVE_WITH_KNOTS('',3,(#33233,#33234,#33235,#33236,#33237,
#33238,#33239,#33240,#33241,#33242,#33243,#33244,#33245,#33246,#33247,#33248,
#33249,#33250,#33251,#33252,#33253,#33254,#33255,#33256,#33257,#33258,#33259,
#33260,#33261,#33262,#33263,#33264,#33265,#33266,#33267,#33268),
 .UNSPECIFIED.,.F.,.F.,(4,2,2,2,2,2,2,2,2,2,2,2,2,2,2,2,2,4),(-35.5495875005638,
-35.4439726245336,-35.3295728971633,-35.2195514508088,-35.1052892058185,
-34.9953989947032,-34.8812737126131,-34.7715141513007,-34.6575252899646,
-34.5478957628118,-34.4340427560889,-34.3245426150538,-34.2108248714336,
-34.1014534337317,-33.9878703349176,-33.8786268805186,-33.765177779973,
-33.7596801984378),.UNSPECIFIED.);
#335=B_SPLINE_CURVE_WITH_KNOTS('',3,(#33273,#33274,#33275,#33276,#33277,
#33278,#33279,#33280,#33281,#33282,#33283,#33284,#33285,#33286,#33287,#33288,
#33289,#33290,#33291,#33292,#33293,#33294,#33295,#33296,#33297,#33298,#33299,
#33300,#33301,#33302,#33303,#33304,#33305,#33306,#33307,#33308),
 .UNSPECIFIED.,.F.,.F.,(4,2,2,2,2,2,2,2,2,2,2,2,2,2,2,2,2,4),(-7.43460594093514,
-7.43103508403617,-7.31493364113757,-7.20314731541428,-7.08690216096382,
-6.97497755039835,-6.85858843734785,-6.74652529782059,-6.62999198343581,
-6.51779007547386,-6.40111232103036,-6.28877140947195,-6.17194897996997,
-6.05946883365251,-5.94250149755131,-5.82988188902049,-5.71276941798947,
-5.60348486335477),.UNSPECIFIED.);
#336=B_SPLINE_CURVE_WITH_KNOTS('',3,(#33309,#33310,#33311,#33312,#33313,
#33314,#33315,#33316,#33317,#33318,#33319,#33320,#33321,#33322,#33323,#33324,
#33325,#33326,#33327,#33328,#33329,#33330,#33331,#33332,#33333,#33334,#33335,
#33336,#33337,#33338,#33339,#33340,#33341,#33342,#33343,#33344),
 .UNSPECIFIED.,.F.,.F.,(4,2,2,2,2,2,2,2,2,2,2,2,2,2,2,2,2,4),(-33.7596801984378,
-33.6560615489264,-33.5427457703844,-33.4337559599665,-33.3205727959264,
-33.2117085575971,-33.0986572677943,-32.9899177039548,-32.8769975138331,
-32.7683816743734,-32.6555917735641,-32.5470986521904,-32.4344381930159,
-32.3260667233496,-32.2135348193684,-32.1052838708055,-31.9928795954187,
-31.9856997234716),.UNSPECIFIED.);
#337=B_SPLINE_CURVE_WITH_KNOTS('',3,(#33349,#33350,#33351,#33352,#33353,
#33354,#33355,#33356,#33357,#33358,#33359,#33360,#33361,#33362,#33363,#33364,
#33365,#33366,#33367,#33368,#33369,#33370,#33371,#33372,#33373,#33374,#33375,
#33376,#33377,#33378,#33379,#33380,#33381,#33382,#33383,#33384),
 .UNSPECIFIED.,.F.,.F.,(4,2,2,2,2,2,2,2,2,2,2,2,2,2,2,2,2,4),(-9.24781408327546,
-9.24404785059257,-9.12908657031949,-9.01839704548918,-8.90329422945898,
-8.79246858929011,-8.67722394216834,-8.56626188992463,-8.45087512400147,
-8.33977637133277,-8.22424720601036,-8.11301147236165,-7.99733963367234,
-7.88596664573283,-7.77015186588773,-7.65864135707772,-7.54268337404331,
-7.43460594093514),.UNSPECIFIED.);
#338=B_SPLINE_CURVE_WITH_KNOTS('',3,(#33385,#33386,#33387,#33388,#33389,
#33390,#33391,#33392,#33393,#33394,#33395,#33396,#33397,#33398,#33399,#33400,
#33401,#33402,#33403,#33404,#33405,#33406,#33407,#33408,#33409,#33410,#33411,
#33412,#33413,#33414,#33415,#33416,#33417,#33418,#33419,#33420),
 .UNSPECIFIED.,.F.,.F.,(4,2,2,2,2,2,2,2,2,2,2,2,2,2,2,2,2,4),(-31.9856997234716,
-31.8847479687416,-31.7724703538844,-31.6644567766188,-31.5523048115627,
-31.4444079330731,-31.3323805633673,-31.224598949686,-31.1126950762707,
-31.0050272046579,-30.8932456831846,-30.7856899364194,-30.6740295768158,
-30.5665842372219,-30.4550438035427,-30.3477070467546,-30.2362852573616,
-30.2262289907375),.UNSPECIFIED.);
#339=B_SPLINE_CURVE_WITH_KNOTS('',3,(#33425,#33426,#33427,#33428,#33429,
#33430,#33431,#33432,#33433,#33434,#33435,#33436,#33437,#33438,#33439,#33440,
#33441,#33442,#33443,#33444,#33445,#33446,#33447,#33448,#33449,#33450,#33451,
#33452,#33453,#33454,#33455,#33456,#33457,#33458,#33459,#33460),
 .UNSPECIFIED.,.F.,.F.,(4,2,2,2,2,2,2,2,2,2,2,2,2,2,2,2,2,4),(-11.0434719915356,
-11.0393361985858,-10.9254954600852,-10.8158829367058,-10.7019033729697,
-10.5921574968065,-10.4780387286715,-10.3681591087133,-10.2539007700906,
-10.1438870302894,-10.0294887673364,-9.91934054557108,-9.8048020159083,
-9.69451896301604,-9.5798398349881,-9.46942161386276,-9.35460156584121,
-9.24781408327546),.UNSPECIFIED.);
#340=B_SPLINE_CURVE_WITH_KNOTS('',3,(#33461,#33462,#33463,#33464,#33465,
#33466,#33467,#33468,#33469,#33470,#33471,#33472,#33473,#33474,#33475,#33476,
#33477,#33478,#33479,#33480,#33481,#33482,#33483,#33484,#33485,#33486,#33487,
#33488,#33489,#33490,#33491,#33492,#33493,#33494,#33495,#33496),
 .UNSPECIFIED.,.F.,.F.,(4,2,2,2,2,2,2,2,2,2,2,2,2,2,2,2,2,4),(-30.2262289907375,
-30.1290551458449,-30.0177506739607,-29.9106251503024,-29.799436624984,
-29.6924135049774,-29.5813395125561,-29.474416478111,-29.3634555641427,
-29.2566301560602,-29.1457808278288,-29.0390504384916,-28.9283111681011,
-28.8216730341374,-28.7110422622252,-28.6044934572187,-28.4939695973085,
-28.4791693611398),.UNSPECIFIED.);
#341=B_SPLINE_CURVE_WITH_KNOTS('',3,(#33501,#33502,#33503,#33504,#33505,
#33506,#33507,#33508,#33509,#33510,#33511,#33512,#33513,#33514,#33515,#33516,
#33517,#33518,#33519,#33520,#33521,#33522,#33523,#33524,#33525,#33526,#33527,
#33528,#33529,#33530,#33531,#33532,#33533,#33534,#33535,#33536),
 .UNSPECIFIED.,.F.,.F.,(4,2,2,2,2,2,2,2,2,2,2,2,2,2,2,2,2,4),(-12.8220763382543,
-12.8172672572996,-12.7045215901235,-12.5959596100703,-12.4830787371158,
-12.3743872228875,-12.2613706246955,-12.1525490180385,-12.0393961966312,
-11.9304439657368,-11.8171544433878,-11.7080710810895,-11.5946443991462,
-11.4854294212359,-11.3718651389923,-11.2625180826477,-11.1488157762692,
-11.0434719915356),.UNSPECIFIED.);
#342=B_SPLINE_CURVE_WITH_KNOTS('',3,(#33537,#33538,#33539,#33540,#33541,
#33542,#33543,#33544,#33545,#33546,#33547,#33548,#33549,#33550,#33551,#33552,
#33553,#33554,#33555,#33556,#33557,#33558,#33559,#33560,#33561,#33562,#33563,
#33564,#33565,#33566,#33567,#33568,#33569,#33570,#33571,#33572),
 .UNSPECIFIED.,.F.,.F.,(4,2,2,2,2,2,2,2,2,2,2,2,2,2,2,2,2,4),(-28.4791693611398,
-28.3875070246388,-28.2770884681434,-28.1707088540541,-28.0603939759199,
-27.9540938629274,-27.8438810278951,-27.7376567686623,-27.6275443380962,
-27.5213920899141,-27.4113784291267,-27.3052941491546,-27.19790732132,-27.0895249674442,
-26.9821403317088,-26.8738980863906,-26.7665104947947,-26.7416213224891),
 .UNSPECIFIED.);
#343=B_SPLINE_CURVE_WITH_KNOTS('',3,(#33577,#33578,#33579,#33580,#33581,
#33582,#33583,#33584,#33585,#33586,#33587,#33588,#33589,#33590,#33591,#33592,
#33593,#33594,#33595,#33596,#33597,#33598,#33599,#33600,#33601,#33602,#33603,
#33604,#33605,#33606,#33607,#33608,#33609,#33610,#33611,#33612),
 .UNSPECIFIED.,.F.,.F.,(4,2,2,2,2,2,2,2,2,2,2,2,2,2,2,2,2,4),(-14.5843512552458,
-14.5783456507132,-14.4666599094173,-14.3591102293336,-14.2472943736648,
-14.1396208394509,-14.0276741285958,-13.9198758885642,-13.8077976145064,
-13.6998738631166,-13.5876633491269,-13.4796133239238,-13.3672699230625,
-13.259092901806,-13.1466159954471,-13.0383112934215,-12.9257002898058,
-12.8220763382543),.UNSPECIFIED.);
#344=B_SPLINE_CURVE_WITH_KNOTS('',3,(#33613,#33614,#33615,#33616,#33617,
#33618,#33619,#33620,#33621,#33622,#33623,#33624,#33625,#33626,#33627,#33628,
#33629,#33630,#33631,#33632,#33633,#33634,#33635,#33636,#33637,#33638,#33639,
#33640,#33641,#33642,#33643,#33644,#33645,#33646,#33647,#33648),
 .UNSPECIFIED.,.F.,.F.,(4,2,2,2,2,2,2,2,2,2,2,2,2,2,2,2,2,4),(-26.7416213224891,
-26.6584069731989,-26.5510113186852,-26.4430449411355,-26.3356361819669,
-26.227805159592,-26.1203783441819,-26.0126806650304,-25.905230956766,-25.7976643726548,
-25.6901870742437,-25.5827490886205,-25.4752396654594,-25.3679275225695,
-25.2603816246109,-25.1531923002647,-25.0456057818525,-25.0095548405133),
 .UNSPECIFIED.);
#345=B_SPLINE_CURVE_WITH_KNOTS('',3,(#33653,#33654,#33655,#33656,#33657,
#33658,#33659,#33660,#33661,#33662,#33663,#33664,#33665,#33666,#33667,#33668,
#33669,#33670,#33671,#33672,#33673,#33674,#33675,#33676,#33677,#33678,#33679,
#33680,#33681,#33682,#33683,#33684,#33685,#33686,#33687,#33688),
 .UNSPECIFIED.,.F.,.F.,(4,2,2,2,2,2,2,2,2,2,2,2,2,2,2,2,2,4),(-16.3313912073472,
-16.3233072623272,-16.2126313466116,-16.1060351236341,-15.9952363748485,
-15.8885252103429,-15.7776025742812,-15.6707751111625,-15.5597275770881,
-15.4527825369049,-15.3416091365489,-15.234545314564,-15.1232451209766,
-15.0160613815074,-14.9046335077918,-14.7973287798048,-14.6857723777617,
-14.5843512552458),.UNSPECIFIED.);
#346=B_SPLINE_CURVE_WITH_KNOTS('',3,(#33689,#33690,#33691,#33692,#33693,
#33694,#33695,#33696,#33697,#33698,#33699,#33700,#33701,#33702,#33703,#33704,
#33705,#33706,#33707,#33708,#33709,#33710,#33711,#33712,#33713,#33714,#33715,
#33716,#33717,#33718,#33719,#33720,#33721,#33722,#33723,#33724),
 .UNSPECIFIED.,.F.,.F.,(4,2,2,2,2,2,2,2,2,2,2,2,2,2,2,2,2,4),(-25.0095548405133,
-24.9385359760839,-24.8309049132433,-24.7239510451331,-24.6162717498346,
-24.5094299547549,-24.4016989857275,-24.2949651152216,-24.1871792849693,
-24.0805489094451,-23.9727052872149,-23.866173701574,-23.7582696121387,
-23.6518318444031,-23.5438648626452,-23.4375156855802,-23.3294836269944,
-23.279856360261),.UNSPECIFIED.);
#347=B_SPLINE_CURVE_WITH_KNOTS('',3,(#33729,#33730,#33731,#33732,#33733,
#33734,#33735,#33736,#33737,#33738,#33739,#33740,#33741,#33742,#33743,#33744,
#33745,#33746,#33747,#33748,#33749,#33750,#33751,#33752,#33753,#33754,#33755,
#33756,#33757,#33758,#33759,#33760,#33761,#33762,#33763,#33764),
 .UNSPECIFIED.,.F.,.F.,(4,2,2,2,2,2,2,2,2,2,2,2,2,2,2,2,2,4),(-18.0648505045038,
-18.0532589064653,-17.9435223335512,-17.8377855197036,-17.7279361558219,
-17.6220987648756,-17.5121352015826,-17.4061950390038,-17.2961159095967,
-17.1900709080828,-17.0798748891579,-16.973723101753,-16.8634089142914,
-16.7571485076961,-16.6467149177216,-16.5403441658243,-16.4297899846795,
-16.3313912073472),.UNSPECIFIED.);
#348=B_SPLINE_CURVE_WITH_KNOTS('',3,(#33765,#33766,#33767,#33768,#33769,
#33770,#33771,#33772,#33773,#33774,#33775,#33776,#33777,#33778,#33779,#33780,
#33781,#33782,#33783,#33784,#33785,#33786,#33787,#33788,#33789,#33790,#33791,
#33792,#33793,#33794,#33795,#33796,#33797,#33798,#33799,#33800),
 .UNSPECIFIED.,.F.,.F.,(4,2,2,2,2,2,2,2,2,2,2,2,2,2,2,2,2,4),(-23.279856360261,
-23.2232175726558,-23.1151184800197,-23.008929857083,-22.9007619836687,
-22.7946448568816,-22.6864066321872,-22.5803544617475,-22.4720444874161,
-22.3660510309762,-22.2576680642617,-22.1517269410299,-22.0432698589546,
-21.9373745771184,-21.8288423511376,-21.7229863362235,-21.6143780072058,
-21.5505504016126),.UNSPECIFIED.);
#349=B_SPLINE_CURVE_WITH_KNOTS('',3,(#33805,#33806,#33807,#33808,#33809,
#33810,#33811,#33812,#33813,#33814,#33815,#33816,#33817,#33818,#33819,#33820,
#33821,#33822,#33823,#33824,#33825,#33826,#33827,#33828,#33829,#33830,#33831,
#33832,#33833,#33834,#33835,#33836,#33837,#33838,#33839,#33840),
 .UNSPECIFIED.,.F.,.F.,(4,2,2,2,2,2,2,2,2,2,2,2,2,2,2,2,2,4),(-19.78711920009,
-19.7698563339641,-19.6609673312242,-19.5559385091401,-19.4469491127778,
-19.3418427059215,-19.2327512982833,-19.1275638383411,-19.0183688100397,
-18.9130970119967,-18.8037967682599,-18.6984375240007,-18.5890304904218,
-18.4835808619618,-18.374065489621,-18.2685227020834,-18.1588974720274,
-18.0648505045038),.UNSPECIFIED.);
#350=B_SPLINE_CURVE_WITH_KNOTS('',3,(#33841,#33842,#33843,#33844,#33845,
#33846,#33847,#33848,#33849,#33850,#33851,#33852,#33853,#33854,#33855,#33856,
#33857,#33858,#33859,#33860,#33861,#33862,#33863,#33864,#33865,#33866,#33867,
#33868,#33869,#33870,#33871,#33872,#33873,#33874,#33875,#33876),
 .UNSPECIFIED.,.F.,.F.,(4,2,2,2,2,2,2,2,2,2,2,2,2,2,2,2,2,4),(-21.5505504016126,
-21.5085546309099,-21.3998692850715,-21.2940718940921,-21.1853086404519,
-21.0795305848717,-20.9706885347095,-20.8649231955014,-20.7560014442002,
-20.6502422594702,-20.5412398710138,-20.4354803606454,-20.326396354935,
-20.2206301433518,-20.1114634864004,-20.0056843232298,-19.8964339201928,
-19.8198937274011),.UNSPECIFIED.);
#351=B_SPLINE_CURVE_WITH_KNOTS('',3,(#33881,#33882,#33883,#33884,#33885,
#33886,#33887,#33888,#33889,#33890,#33891,#33892,#33893,#33894,#33895,#33896,
#33897,#33898,#33899,#33900,#33901,#33902,#33903,#33904,#33905,#33906,#33907,
#33908,#33909,#33910,#33911,#33912,#33913,#33914,#33915,#33916),
 .UNSPECIFIED.,.F.,.F.,(4,2,2,2,2,2,2,2,2,2,2,2,2,2,2,2,2,4),(-21.5013063400995,
-21.4754634098236,-21.3673207575314,-21.2627641819231,-21.1545334840107,
-21.0499342013519,-20.9416140435757,-20.8369669813094,-20.7285558978255,
-20.6238561866133,-20.5153526667363,-20.4105956426116,-20.3019981382347,
-20.1971793430677,-20.0884862764785,-19.983601456934,-19.8748112287902,
-19.78711920009),.UNSPECIFIED.);
#352=B_SPLINE_CURVE_WITH_KNOTS('',3,(#33917,#33918,#33919,#33920,#33921,
#33922,#33923,#33924,#33925,#33926,#33927,#33928,#33929,#33930,#33931,#33932,
#33933,#33934,#33935,#33936,#33937,#33938,#33939,#33940,#33941,#33942,#33943,
#33944,#33945,#33946,#33947,#33948,#33949,#33950,#33951,#33952),
 .UNSPECIFIED.,.F.,.F.,(4,2,2,2,2,2,2,2,2,2,2,2,2,2,2,2,2,4),(-19.8198937274011,
-19.790635698669,-19.6813003895888,-19.5754771626003,-19.4660557206704,
-19.3602017144112,-19.2506928465104,-19.1448024717488,-19.0352048209613,
-18.9292726819867,-18.8195848317987,-18.7136057331458,-18.6038262130013,
-18.4977951640837,-18.3879224559889,-18.2818346737982,-18.171867219676,
-18.0853560917774),.UNSPECIFIED.);
#353=B_SPLINE_CURVE_WITH_KNOTS('',3,(#33957,#33958,#33959,#33960,#33961,
#33962,#33963,#33964,#33965,#33966,#33967,#33968,#33969,#33970,#33971,#33972,
#33973,#33974,#33975,#33976,#33977,#33978,#33979,#33980,#33981,#33982,#33983,
#33984,#33985,#33986,#33987,#33988,#33989,#33990,#33991,#33992),
 .UNSPECIFIED.,.F.,.F.,(4,2,2,2,2,2,2,2,2,2,2,2,2,2,2,2,2,4),(-23.2107745567376,
-23.1731702436624,-23.0656884326081,-22.9612688279359,-22.8537080700236,
-22.7492927201854,-22.6416520801072,-22.5372346143341,-22.4295131102289,
-22.3250872669613,-22.2172838615344,-22.1128435082049,-22.0049571026223,
-21.9004962531731,-21.7925256835865,-21.6880385136444,-21.5799825501392,
-21.5013063400995),.UNSPECIFIED.);
#354=B_SPLINE_CURVE_WITH_KNOTS('',3,(#33993,#33994,#33995,#33996,#33997,
#33998,#33999,#34000,#34001,#34002,#34003,#34004,#34005,#34006,#34007,#34008,
#34009,#34010,#34011,#34012,#34013,#34014,#34015,#34016,#34017,#34018,#34019,
#34020,#34021,#34022,#34023,#34024,#34025,#34026,#34027,#34028),
 .UNSPECIFIED.,.F.,.F.,(4,2,2,2,2,2,2,2,2,2,2,2,2,2,2,2,2,4),(-18.0853560917774,
-18.0657181297179,-17.9556543392361,-17.849439574889,-17.739277833515,-17.6329932339954,
-17.5227319110613,-17.4163735181846,-17.3060109747783,-17.1995750286937,
-17.0891096252262,-16.9825925592995,-16.8720226626297,-16.7654210976342,
-16.6547450876619,-16.5480558254253,-16.437272101092,-16.343613120543),
 .UNSPECIFIED.);
#355=B_SPLINE_CURVE_WITH_KNOTS('',3,(#34033,#34034,#34035,#34036,#34037,
#34038,#34039,#34040,#34041,#34042,#34043,#34044,#34045,#34046,#34047,#34048,
#34049,#34050,#34051,#34052,#34053,#34054,#34055,#34056,#34057,#34058,#34059,
#34060,#34061,#34062,#34063,#34064,#34065,#34066,#34067,#34068),
 .UNSPECIFIED.,.F.,.F.,(4,2,2,2,2,2,2,2,2,2,2,2,2,2,2,2,2,4),(-24.9183017004615,
-24.8665828889058,-24.759699498358,-24.655011382145,-24.5480567922721,-24.4434248725477,
-24.3363978924142,-24.2318158355854,-24.1247153854245,-24.0201767561447,
-23.9130018423663,-23.8085001317139,-23.7012498224075,-23.5967784763971,
-23.4894518779437,-23.3850043259115,-23.2776005612417,-23.2107745567376),
 .UNSPECIFIED.);
#356=B_SPLINE_CURVE_WITH_KNOTS('',3,(#34069,#34070,#34071,#34072,#34073,
#34074,#34075,#34076,#34077,#34078,#34079,#34080,#34081,#34082,#34083,#34084,
#34085,#34086,#34087,#34088,#34089,#34090,#34091,#34092,#34093,#34094,#34095,
#34096,#34097,#34098,#34099,#34100,#34101,#34102,#34103,#34104),
 .UNSPECIFIED.,.F.,.F.,(4,2,2,2,2,2,2,2,2,2,2,2,2,2,2,2,2,4),(-16.343613120543,
-16.3304921177346,-16.2195991023927,-16.1127255412756,-16.0017216874107,
-15.8947518519012,-15.7836356452055,-15.67656699135,-15.5653369541634,-15.4581670833479,
-15.34682177749,-15.2395484291535,-15.128086458181,-15.020707502638,-14.9091275135678,
-14.8016409449841,-14.6899416295231,-14.5913702832229),.UNSPECIFIED.);
#357=B_SPLINE_CURVE_WITH_KNOTS('',3,(#34109,#34110,#34111,#34112,#34113,
#34114,#34115,#34116,#34117,#34118,#34119,#34120,#34121,#34122,#34123,#34124,
#34125,#34126,#34127,#34128,#34129,#34130,#34131,#34132,#34133,#34134,#34135,
#34136,#34137,#34138,#34139,#34140,#34141,#34142,#34143,#34144),
 .UNSPECIFIED.,.F.,.F.,(4,2,2,2,2,2,2,2,2,2,2,2,2,2,2,2,2,4),(-26.6257527730801,
-26.5595330341774,-26.4531553556633,-26.3478065454012,-26.241373857084,
-26.136125938725,-26.0296354188406,-25.9244836714166,-25.817932749385,-25.71287219139,
-25.6062585413088,-25.5012839430023,-25.3946054731675,-25.289711371732,
-25.1829662104685,-25.0781469278626,-24.9713334060639,-24.9183017004615),
 .UNSPECIFIED.);
#358=B_SPLINE_CURVE_WITH_KNOTS('',3,(#34145,#34146,#34147,#34148,#34149,
#34150,#34151,#34152,#34153,#34154,#34155,#34156,#34157,#34158,#34159,#34160,
#34161,#34162,#34163,#34164,#34165,#34166,#34167,#34168,#34169,#34170,#34171,
#34172,#34173,#34174,#34175,#34176,#34177,#34178,#34179,#34180),
 .UNSPECIFIED.,.F.,.F.,(4,2,2,2,2,2,2,2,2,2,2,2,2,2,2,2,2,4),(-14.5913702832229,
-14.5823455590806,-14.4705256544105,-14.36281830369,-14.2508765928518,-14.1430562874532,
-14.0309915993766,-13.9230567627926,-13.8108679720163,-13.7028171197676,
-13.5905031458913,-13.4823348799311,-13.3698946868393,-13.2616076902261,
-13.1490402851216,-13.0406333169609,-12.9279377492393,-12.8259818435135),
 .UNSPECIFIED.);
#359=B_SPLINE_CURVE_WITH_KNOTS('',3,(#34185,#34186,#34187,#34188,#34189,
#34190,#34191,#34192,#34193,#34194,#34195,#34196,#34197,#34198,#34199,#34200,
#34201,#34202,#34203,#34204,#34205,#34206,#34207,#34208,#34209,#34210,#34211,
#34212,#34213,#34214,#34215,#34216,#34217,#34218,#34219,#34220),
 .UNSPECIFIED.,.F.,.F.,(4,2,2,2,2,2,2,2,2,2,2,2,2,2,2,2,2,4),(-28.3349853381226,
-28.2567214667917,-28.1486990903277,-28.0442274779986,-27.9362901024047,
-27.8318430252495,-27.7239894411045,-27.619561023636,-27.5117900874993,
-27.4073742969973,-27.2996849296331,-27.1952755920485,-27.0876667741569,
-26.98325759234,-26.8757283576048,-26.7713129316046,-26.6649871874145,-26.6257527730801),
 .UNSPECIFIED.);
#360=B_SPLINE_CURVE_WITH_KNOTS('',3,(#34221,#34222,#34223,#34224,#34225,
#34226,#34227,#34228,#34229,#34230,#34231,#34232,#34233,#34234,#34235,#34236,
#34237,#34238,#34239,#34240,#34241,#34242,#34243,#34244,#34245,#34246,#34247,
#34248,#34249,#34250,#34251,#34252,#34253,#34254,#34255,#34256),
 .UNSPECIFIED.,.F.,.F.,(4,2,2,2,2,2,2,2,2,2,2,2,2,2,2,2,2,4),(-12.8259818435135,
-12.8194096398901,-12.7065849998897,-12.5979346464299,-12.4849800640805,
-12.3762064260245,-12.263121069424,-12.1542231646846,-12.0410062386213,
-11.9319831397061,-11.8186338841484,-11.7094847145824,-11.5960024031513,
-11.4867263341141,-11.3731102725527,-11.2637065197223,-11.1499560443741,
-11.0455738233171),.UNSPECIFIED.);
#361=B_SPLINE_CURVE_WITH_KNOTS('',3,(#34261,#34262,#34263,#34264,#34265,
#34266,#34267,#34268,#34269,#34270,#34271,#34272,#34273,#34274,#34275,#34276,
#34277,#34278,#34279,#34280,#34281,#34282,#34283,#34284,#34285,#34286,#34287,
#34288,#34289,#34290,#34291,#34292,#34293,#34294,#34295,#34296),
 .UNSPECIFIED.,.F.,.F.,(4,2,2,2,2,2,2,2,2,2,2,2,2,2,2,2,2,4),(-30.0488168723486,
-29.9614261880733,-29.8526732714368,-29.7478161474901,-29.6391598895154,
-29.5343674916912,-29.4258062989781,-29.3210743110622,-29.2126066143105,
-29.1079305148352,-28.9995547767932,-28.8949298384416,-28.7866445616262,
-28.6820658522004,-28.5738695861414,-28.4693319712739,-28.3612233190107,
-28.3349853381226),.UNSPECIFIED.);
#362=B_SPLINE_CURVE_WITH_KNOTS('',3,(#34297,#34298,#34299,#34300,#34301,
#34302,#34303,#34304,#34305,#34306,#34307,#34308,#34309,#34310,#34311,#34312,
#34313,#34314,#34315,#34316,#34317,#34318,#34319,#34320,#34321,#34322,#34323,
#34324,#34325,#34326,#34327,#34328,#34329,#34330,#34331,#34332),
 .UNSPECIFIED.,.F.,.F.,(4,2,2,2,2,2,2,2,2,2,2,2,2,2,2,2,2,4),(-11.0455738233171,
-11.0404238649656,-10.926538341273,-10.8168770312622,-10.7028558522917,
-10.5930647438152,-10.4789073288171,-10.3689857877375,-10.2546915807464,
-10.1446390043743,-10.0302074728524,-9.92002328781561,-9.80545392134402,
-9.6951375815958,-9.58042989061549,-9.46998087557298,-9.35513439017667,
-9.24889674820361),.UNSPECIFIED.);
#363=B_SPLINE_CURVE_WITH_KNOTS('',3,(#34337,#34338,#34339,#34340,#34341,
#34342,#34343,#34344,#34345,#34346,#34347,#34348,#34349,#34350,#34351,#34352,
#34353,#34354,#34355,#34356,#34357,#34358,#34359,#34360,#34361,#34362,#34363,
#34364,#34365,#34366,#34367,#34368,#34369,#34370,#34371,#34372),
 .UNSPECIFIED.,.F.,.F.,(4,2,2,2,2,2,2,2,2,2,2,2,2,2,2,2,2,4),(-31.7705993303663,
-31.6767622191949,-31.5671782708775,-31.4616714603343,-31.3521968961548,
-31.2467823972444,-31.137415688639,-31.0320906769712,-30.9228302667284,
-30.8175917526226,-30.7084360595614,-30.6032808810914,-30.4942283053797,
-30.3891531217064,-30.2802020507996,-30.175203335912,-30.0663521510776,
-30.0488168723486),.UNSPECIFIED.);
#364=B_SPLINE_CURVE_WITH_KNOTS('',3,(#34373,#34374,#34375,#34376,#34377,
#34378,#34379,#34380,#34381,#34382,#34383,#34384,#34385,#34386,#34387,#34388,
#34389,#34390,#34391,#34392,#34393,#34394,#34395,#34396,#34397,#34398,#34399,
#34400,#34401,#34402,#34403,#34404,#34405,#34406,#34407,#34408),
 .UNSPECIFIED.,.F.,.F.,(4,2,2,2,2,2,2,2,2,2,2,2,2,2,2,2,2,4),(-9.24889674820361,
-9.24455220298207,-9.129566471758,-9.01885063765458,-8.90372522658263,-8.79287529139848,
-8.67760978279836,-8.56662531153122,-8.45121930306199,-8.34009987855865,
-8.22455298226888,-8.11329820399297,-7.99761004542018,-7.88621952830298,
-7.77038974562149,-7.65886311898992,-7.54289136220465,-7.4351272610323),
 .UNSPECIFIED.);
#365=B_SPLINE_CURVE_WITH_KNOTS('',3,(#34413,#34414,#34415,#34416,#34417,
#34418,#34419,#34420,#34421,#34422,#34423,#34424,#34425,#34426,#34427,#34428,
#34429,#34430,#34431,#34432,#34433,#34434,#34435,#34436,#34437,#34438,#34439,
#34440,#34441,#34442,#34443,#34444,#34445,#34446,#34447,#34448),
 .UNSPECIFIED.,.F.,.F.,(4,2,2,2,2,2,2,2,2,2,2,2,2,2,2,2,2,4),(-33.5034635227188,
-33.4052107333307,-33.2947011786237,-33.1883716652711,-33.0779823310297,
-32.9717626329138,-32.8614923165309,-32.7553806751721,-32.6452281287722,
-32.539222676534,-32.4291866073623,-32.3232853609123,-32.2133644321201,
-32.1075652856769,-31.9977581175486,-31.8920588359429,-31.7823640076096,
-31.7705993303663),.UNSPECIFIED.);
#366=B_SPLINE_CURVE_WITH_KNOTS('',3,(#34449,#34450,#34451,#34452,#34453,
#34454,#34455,#34456,#34457,#34458,#34459,#34460,#34461,#34462,#34463,#34464,
#34465,#34466,#34467,#34468,#34469,#34470,#34471,#34472,#34473,#34474,#34475,
#34476,#34477,#34478,#34479,#34480,#34481,#34482,#34483,#34484),
 .UNSPECIFIED.,.F.,.F.,(4,2,2,2,2,2,2,2,2,2,2,2,2,2,2,2,2,4),(-7.4351272610323,
-7.43122826878166,-7.3151141989672,-7.20331429393996,-7.08705758252279,
-6.97512053267358,-6.85872086075526,-6.74664634365187,-6.63010340137265,
-6.51789110461339,-6.40120459055263,-6.28885421106297,-6.1720238316763,
-6.05953507505318,-5.94256054414322,-5.82993312404414,-5.71281416226422,
-5.60370818057896),.UNSPECIFIED.);
#367=B_SPLINE_CURVE_WITH_KNOTS('',3,(#34489,#34490,#34491,#34492,#34493,
#34494,#34495,#34496,#34497,#34498,#34499,#34500,#34501,#34502,#34503,#34504,
#34505,#34506,#34507,#34508,#34509,#34510,#34511,#34512,#34513,#34514,#34515,
#34516,#34517,#34518,#34519,#34520,#34521,#34522,#34523,#34524),
 .UNSPECIFIED.,.F.,.F.,(4,2,2,2,2,2,2,2,2,2,2,2,2,2,2,2,2,4),(-35.249829569753,
-35.1485139120437,-35.037004621044,-34.92974441726,-34.8183633878881,-34.7112238400841,
-34.5999702123749,-34.4929502300442,-34.3818231049099,-34.2749215315651,
-34.1639199694648,-34.0571355781546,-33.9462585978623,-33.8395900864318,
-33.7288366639292,-33.62228265002,-33.5116517175468,-33.5034635227188),
 .UNSPECIFIED.);
#368=B_SPLINE_CURVE_WITH_KNOTS('',3,(#34525,#34526,#34527,#34528,#34529,
#34530,#34531,#34532,#34533,#34534,#34535,#34536,#34537,#34538,#34539,#34540,
#34541,#34542,#34543,#34544,#34545,#34546,#34547,#34548,#34549,#34550,#34551,
#34552,#34553,#34554,#34555,#34556,#34557,#34558,#34559,#34560),
 .UNSPECIFIED.,.F.,.F.,(4,2,2,2,2,2,2,2,2,2,2,2,2,2,2,2,2,4),(-5.60370818057896,
-5.60004779983838,-5.48278413422669,-5.36987855758419,-5.25246992112663,
-5.13942486484497,-5.02187099606657,-4.90868620073017,-4.79098684331131,
-4.67766205508293,-4.55981695750053,-4.44635192772174,-4.32836084291342,
-4.21475532773292,-4.09661801278269,-3.98287177280955,-3.86458798865395,
-3.75424064676522),.UNSPECIFIED.);
#369=B_SPLINE_CURVE_WITH_KNOTS('',3,(#34565,#34566,#34567,#34568,#34569,
#34570,#34571,#34572,#34573,#34574,#34575,#34576,#34577,#34578,#34579,#34580,
#34581,#34582,#34583,#34584,#34585,#34586,#34587,#34588,#34589,#34590,#34591,
#34592,#34593,#34594,#34595,#34596,#34597,#34598,#34599,#34600),
 .UNSPECIFIED.,.F.,.F.,(4,2,2,2,2,2,2,2,2,2,2,2,2,2,2,2,2,4),(-37.0113773411355,
-36.9078345617278,-36.7952724338226,-36.6870143515743,-36.5745861319252,
-36.4664555141774,-36.3541606029054,-36.2461567536563,-36.1339945235731,
-36.0261167084853,-35.9140865036374,-35.8063339472929,-35.6944350814774,
-35.5868069644492,-35.4750387197121,-35.3675341754426,-35.2558958005675,
-35.249829569753),.UNSPECIFIED.);
#370=B_SPLINE_CURVE_WITH_KNOTS('',3,(#34601,#34602,#34603,#34604,#34605,
#34606,#34607,#34608,#34609,#34610,#34611,#34612,#34613,#34614,#34615,#34616,
#34617,#34618,#34619,#34620,#34621,#34622,#34623,#34624,#34625,#34626,#34627,
#34628,#34629,#34630,#34631,#34632,#34633,#34634,#34635,#34636),
 .UNSPECIFIED.,.F.,.F.,(4,2,2,2,2,2,2,2,2,2,2,2,2,2,2,2,2,4),(-3.75424064676522,
-3.7507007886352,-3.63227029978869,-3.51824190830858,-3.39966448260667,
-3.28549467180693,-3.16677008016633,-3.05245862548541,-2.9335866416799,
-2.81913332161029,-2.70011372206143,-2.58551831792344,-2.4663508815052,
-2.35161317723662,-2.23229768509284,-2.11741746705273,-1.99795370242702,
-1.88641723413452),.UNSPECIFIED.);
#371=B_SPLINE_CURVE_WITH_KNOTS('',3,(#34641,#34642,#34643,#34644,#34645,
#34646,#34647,#34648,#34649,#34650,#34651,#34652,#34653,#34654,#34655,#34656,
#34657,#34658,#34659,#34660,#34661,#34662,#34663,#34664,#34665,#34666,#34667,
#34668,#34669,#34670,#34671,#34672,#34673,#34674,#34675,#34676),
 .UNSPECIFIED.,.F.,.F.,(4,2,2,2,2,2,2,2,2,2,2,2,2,2,2,2,2,4),(-38.7892191392797,
-38.6839424852085,-38.5702903229789,-38.4609912918716,-38.3474770154212,
-38.2383099131738,-38.1249330935883,-38.0158974509548,-37.9026576421227,
-37.7937529679977,-37.6806497055188,-37.5718754853313,-37.4589082853741,
-37.350263979368,-37.2374323374757,-37.1289173788685,-37.0162207687146,
-37.0113773411355),.UNSPECIFIED.);
#372=B_SPLINE_CURVE_WITH_KNOTS('',3,(#34677,#34678,#34679,#34680,#34681,
#34682,#34683,#34684,#34685,#34686,#34687,#34688,#34689,#34690,#34691,#34692,
#34693,#34694,#34695,#34696,#34697,#34698,#34699,#34700,#34701,#34702,#34703,
#34704,#34705,#34706,#34707,#34708,#34709,#34710,#34711,#34712),
 .UNSPECIFIED.,.F.,.F.,(4,2,2,2,2,2,2,2,2,2,2,2,2,2,2,2,2,4),(-1.88641723413452,
-1.88293076106139,-1.7633185725453,-1.6481527558743,-1.52839186711642,-1.41308290859082,
-1.29317310822235,-1.17772080218214,-1.0576618803597,-0.942066022770442,
-0.821857771055554,-0.706118159380599,-0.585760370627368,-0.469876803708684,
-0.349369271959349,-0.2333415499069,-0.116644727036975,-1.00000007829948E-6),
 .UNSPECIFIED.);
#373=B_SPLINE_CURVE_WITH_KNOTS('',3,(#34717,#34718,#34719,#34720,#34721,
#34722,#34723,#34724,#34725,#34726,#34727,#34728,#34729,#34730,#34731,#34732,
#34733,#34734,#34735,#34736,#34737,#34738,#34739,#34740,#34741,#34742,#34743,
#34744,#34745,#34746,#34747,#34748,#34749,#34750,#34751,#34752),
 .UNSPECIFIED.,.F.,.F.,(4,2,2,2,2,2,2,2,2,2,2,2,2,2,2,2,2,4),(-40.5840903660244,
-40.4773621269581,-40.362593181144,-40.2522239979018,-40.1375958644443,
-40.0273617375903,-39.9128740918523,-39.8027746806653,-39.6884271877721,
-39.578462139203,-39.4642544533322,-39.3544234010816,-39.2403551647114,
-39.1306577282415,-39.0167285713529,-38.9071643548272,-38.793373894062,
-38.7892191392797),.UNSPECIFIED.);
#374=B_SPLINE_CURVE_WITH_KNOTS('',3,(#34753,#34754,#34755,#34756,#34757,
#34758,#34759,#34760,#34761,#34762,#34763,#34764,#34765,#34766,#34767,#34768,
#34769,#34770,#34771,#34772,#34773,#34774,#34775,#34776,#34777,#34778,#34779,
#34780,#34781,#34782,#34783,#34784,#34785,#34786,#34787,#34788),
 .UNSPECIFIED.,.F.,.F.,(4,2,2,2,2,2,2,2,2,2,2,2,2,2,2,2,2,4),(-7.49403777883289,
-7.41673253643292,-7.33806391100879,-7.22291817343654,-7.10721789492446,
-6.9919436003314,-6.87628697708284,-6.7608805786065,-6.64526315078516,-6.52972139809384,
-6.41413848618954,-6.2984584175721,-6.18290514374928,-6.06708407617364,
-5.95155538779921,-5.83559090525242,-5.72008160003587,-5.63205117539197),
 .UNSPECIFIED.);
#375=B_SPLINE_CURVE_WITH_KNOTS('',3,(#34793,#34794,#34795,#34796,#34797,
#34798,#34799,#34800,#34801,#34802,#34803,#34804,#34805,#34806,#34807,#34808,
#34809,#34810,#34811,#34812,#34813,#34814,#34815,#34816,#34817,#34818,#34819,
#34820,#34821,#34822,#34823,#34824,#34825,#34826,#34827,#34828),
 .UNSPECIFIED.,.F.,.F.,(4,2,2,2,2,2,2,2,2,2,2,2,2,2,2,2,2,4),(-42.3964944372798,
-42.2884719551661,-42.1725658485947,-42.0611051693233,-41.9453421761501,
-41.834018927021,-41.7183987834928,-41.6072126959141,-41.4917351323945,
-41.3806859308888,-41.2653506714268,-41.1544380731067,-41.0392448349755,
-40.9284685489806,-40.8134170421869,-40.7027767690798,-40.5878666958406,
-40.5840903660244),.UNSPECIFIED.);
#376=B_SPLINE_CURVE_WITH_KNOTS('',3,(#34829,#34830,#34831,#34832,#34833,
#34834,#34835,#34836,#34837,#34838,#34839,#34840,#34841,#34842,#34843,#34844,
#34845,#34846,#34847,#34848,#34849,#34850,#34851,#34852,#34853,#34854,#34855,
#34856,#34857,#34858,#34859,#34860,#34861,#34862,#34863,#34864),
 .UNSPECIFIED.,.F.,.F.,(4,2,2,2,2,2,2,2,2,2,2,2,2,2,2,2,2,4),(-5.63205117539197,
-5.60397154046265,-5.48847629264442,-5.37221873379735,-5.25673212084505,
-5.14032536534831,-5.02484189465898,-4.90828445456914,-4.79279858972369,
-4.67608917084805,-4.56059535702089,-4.44373284322738,-4.32822553141539,
-4.21120896913925,-4.09280065613099,-3.97853814728176,-3.86002416031382,
-3.76459284001855),.UNSPECIFIED.);
#377=B_SPLINE_CURVE_WITH_KNOTS('',3,(#34869,#34870,#34871,#34872,#34873,
#34874,#34875,#34876,#34877,#34878,#34879,#34880,#34881,#34882,#34883,#34884,
#34885,#34886,#34887,#34888,#34889,#34890,#34891,#34892,#34893,#34894,#34895,
#34896,#34897,#34898,#34899,#34900,#34901,#34902,#34903,#34904),
 .UNSPECIFIED.,.F.,.F.,(4,2,2,2,2,2,2,2,2,2,2,2,2,2,2,2,2,4),(-44.2267979604378,
-44.1175661329609,-44.0005062076739,-43.8879370974253,-43.7710222273151,
-43.6585925002181,-43.5418224560014,-43.4295318834992,-43.3129064326076,
-43.2007547823476,-43.0842736886739,-42.9722607242104,-42.8559237478365,
-42.7440492283116,-42.6278561252182,-42.5161198050192,-42.4000703267746,
-42.3964944372798),.UNSPECIFIED.);
#378=B_SPLINE_CURVE_WITH_KNOTS('',3,(#34905,#34906,#34907,#34908,#34909,
#34910,#34911,#34912,#34913,#34914,#34915,#34916,#34917,#34918,#34919,#34920,
#34921,#34922,#34923,#34924,#34925,#34926,#34927,#34928,#34929,#34930,#34931,
#34932,#34933,#34934,#34935,#34936,#34937,#34938,#34939,#34940),
 .UNSPECIFIED.,.F.,.F.,(4,2,2,2,2,2,2,2,2,2,2,2,2,2,2,2,2,4),(-3.76459284001855,
-3.74568575401325,-3.62706433685894,-3.51264581413931,-3.39391520319397,
-3.27941255749952,-3.16057098984337,-3.04598042137986,-2.927026142345,-2.81234405171484,
-2.69327532186702,-2.57849830314693,-2.45931340462086,-2.34443823802314,
-2.22513548017335,-2.11015912441778,-1.99073684877269,-1.88834843134424),
 .UNSPECIFIED.);
#379=B_SPLINE_CURVE_WITH_KNOTS('',3,(#34945,#34946,#34947,#34948,#34949,
#34950,#34951,#34952,#34953,#34954,#34955,#34956,#34957,#34958,#34959,#34960,
#34961,#34962,#34963,#34964,#34965,#34966,#34967,#34968,#34969,#34970,#34971,
#34972,#34973,#34974,#34975,#34976,#34977,#34978,#34979,#34980),
 .UNSPECIFIED.,.F.,.F.,(4,2,2,2,2,2,2,2,2,2,2,2,2,2,2,2,2,4),(-46.0752889773848,
-45.964891178069,-45.8466628798698,-45.7329708487168,-45.6148893471227,
-45.5013384204638,-45.3834035051267,-45.2699934762495,-45.1522049350479,
-45.0389355951934,-44.9212932140859,-44.8081643522802,-44.6906679151483,
-44.5776793180225,-44.460328606502,-44.347480058098,-44.2302748513988,-44.2267979604378),
 .UNSPECIFIED.);
#380=B_SPLINE_CURVE_WITH_KNOTS('',3,(#34981,#34982,#34983,#34984,#34985,
#34986,#34987,#34988,#34989,#34990,#34991,#34992,#34993,#34994,#34995,#34996,
#34997,#34998,#34999,#35000,#35001,#35002,#35003,#35004,#35005,#35006,#35007,
#35008,#35009,#35010,#35011,#35012,#35013,#35014,#35015,#35016),
 .UNSPECIFIED.,.F.,.F.,(4,2,2,2,2,2,2,2,2,2,2,2,2,2,2,2,2,4),(-1.88834843134424,
-1.87565643327968,-1.7561130177999,-1.64092583480119,-1.52125969746077,
-1.40596319410974,-1.28617279582862,-1.17076456637983,-1.05084841334602,
-0.935326191460909,-0.815282836884644,-0.699644488109694,-0.579472533457261,
-0.4637160479124,-0.343414143669268,-0.227537628973816,-0.113637758694294,
0.),.UNSPECIFIED.);
#381=B_SPLINE_CURVE_WITH_KNOTS('',3,(#35021,#35022,#35023,#35024,#35025,
#35026,#35027,#35028,#35029,#35030,#35031,#35032,#35033,#35034,#35035,#35036,
#35037,#35038,#35039,#35040,#35041,#35042,#35043,#35044,#35045,#35046,#35047,
#35048,#35049,#35050,#35051,#35052,#35053,#35054,#35055,#35056),
 .UNSPECIFIED.,.F.,.F.,(4,2,2,2,2,2,2,2,2,2,2,2,2,2,2,2,2,4),(-47.9422113160818,
-47.8306672541019,-47.7112571821755,-47.5964290719752,-47.4771674302257,
-47.3624820212509,-47.2433686092934,-47.1288257063837,-47.0098603229286,
-46.8954597298667,-46.7766421726348,-46.6623836920508,-46.5437137576842,
-46.429597190954,-46.3110746749191,-46.1970998220542,-46.0787245185386,
-46.0752889773848),.UNSPECIFIED.);
#382=B_SPLINE_CURVE_WITH_KNOTS('',3,(#35057,#35058,#35059,#35060,#35061,
#35062,#35063,#35064,#35065,#35066,#35067,#35068,#35069,#35070,#35071,#35072,
#35073,#35074,#35075,#35076,#35077,#35078,#35079,#35080,#35081,#35082,#35083,
#35084,#35085,#35086,#35087,#35088,#35089,#35090,#35091,#35092),
 .UNSPECIFIED.,.F.,.F.,(4,2,2,2,2,2,2,2,2,2,2,2,2,2,2,2,2,4),(-9.73841549569248,
-9.64066589843865,-9.54184328358783,-9.42684071170168,-9.30840307871922,
-9.19339350762375,-9.07504249845454,-8.96001878949922,-8.84175342158102,
-8.72670837518871,-8.60852768245023,-8.49345406672159,-8.37535707971806,
-8.26024766039142,-8.14223338386421,-8.0270809552092,-7.90914834348772,
-7.85755307378671),.UNSPECIFIED.);
#383=B_SPLINE_CURVE_WITH_KNOTS('',3,(#35097,#35098,#35099,#35100,#35101,
#35102,#35103,#35104,#35105,#35106,#35107,#35108,#35109,#35110,#35111,#35112,
#35113,#35114,#35115,#35116,#35117,#35118,#35119,#35120,#35121,#35122,#35123,
#35124,#35125,#35126,#35127,#35128,#35129,#35130,#35131,#35132),
 .UNSPECIFIED.,.F.,.F.,(4,2,2,2,2,2,2,2,2,2,2,2,2,2,2,2,2,4),(-49.8277844545049,
-49.7151003815012,-49.5944957394318,-49.4785190939317,-49.3580644608813,
-49.242232049276,-49.1219272296907,-49.0062388625519,-48.8860836604681,
-48.77053914787,-48.6505333668662,-48.5351325183314,-48.4152759614772,-48.300018585919,
-48.18031105572,-48.0651969613802,-47.9456382597193,-47.9422113160818),
 .UNSPECIFIED.);
#384=B_SPLINE_CURVE_WITH_KNOTS('',3,(#35133,#35134,#35135,#35136,#35137,
#35138,#35139,#35140,#35141,#35142,#35143,#35144,#35145,#35146,#35147,#35148,
#35149,#35150,#35151,#35152,#35153,#35154,#35155,#35156,#35157,#35158,#35159,
#35160,#35161,#35162,#35163,#35164,#35165,#35166,#35167,#35168),
 .UNSPECIFIED.,.F.,.F.,(4,2,2,2,2,2,2,2,2,2,2,2,2,2,2,2,2,4),(-7.85755307378671,
-7.79394575966839,-7.67609369044231,-7.56083389685531,-7.44306114393897,
-7.32773720801898,-7.21004241380288,-7.09464755478704,-6.97702919010705,
-6.86155628126466,-6.74401263106893,-6.62845525109629,-6.51098440652207,
-6.39533637675224,-6.27793619918513,-6.16219158472876,-6.04485968769943,
-5.97715388014199),.UNSPECIFIED.);
#385=B_SPLINE_CURVE_WITH_KNOTS('',3,(#35173,#35174,#35175,#35176,#35177,
#35178,#35179,#35180,#35181,#35182,#35183,#35184,#35185,#35186,#35187,#35188,
#35189,#35190,#35191,#35192,#35193,#35194,#35195,#35196,#35197,#35198,#35199,
#35200,#35201,#35202,#35203,#35204,#35205,#35206,#35207,#35208),
 .UNSPECIFIED.,.F.,.F.,(4,2,2,2,2,2,2,2,2,2,2,2,2,2,2,2,2,4),(-51.7322148856786,
-51.6183893945336,-51.4965776761934,-51.3794403848007,-51.2577802299048,
-51.14078867526,-51.0192798901623,-50.9024338852763,-50.7810762762027,-50.6643756339059,
-50.5431690069267,-50.4266135398375,-50.3055577008387,-50.1891472213314,
-50.0682419759833,-49.9519762961531,-49.8312214498766,-49.8277844545049),
 .UNSPECIFIED.);
#386=B_SPLINE_CURVE_WITH_KNOTS('',3,(#35209,#35210,#35211,#35212,#35213,
#35214,#35215,#35216,#35217,#35218,#35219,#35220,#35221,#35222,#35223,#35224,
#35225,#35226,#35227,#35228,#35229,#35230,#35231,#35232,#35233,#35234,#35235,
#35236,#35237,#35238,#35239,#35240,#35241,#35242,#35243,#35244),
 .UNSPECIFIED.,.F.,.F.,(4,2,2,2,2,2,2,2,2,2,2,2,2,2,2,2,2,4),(-5.97715388014199,
-5.92901281616251,-5.811746551025,-5.69579202819225,-5.57858847398357,-5.46252119631723,
-5.34537715406377,-5.2291923179436,-5.11210430953573,-4.99579741723946,
-4.87876168885324,-4.76377104513167,-4.64521911964579,-4.53022541977396,
-4.41158432394141,-4.29658068603151,-4.17784927068626,-4.09558903017493),
 .UNSPECIFIED.);
#387=B_SPLINE_CURVE_WITH_KNOTS('',3,(#35249,#35250,#35251,#35252,#35253,
#35254,#35255,#35256,#35257,#35258,#35259,#35260,#35261,#35262,#35263,#35264,
#35265,#35266,#35267,#35268,#35269,#35270,#35271,#35272,#35273,#35274,#35275,
#35276,#35277,#35278,#35279,#35280,#35281,#35282,#35283,#35284),
 .UNSPECIFIED.,.F.,.F.,(4,2,2,2,2,2,2,2,2,2,2,2,2,2,2,2,2,4),(-53.6557025845032,
-53.5407298928425,-53.4176987034498,-53.2993887996668,-53.1765107209798,
-53.0583480463698,-52.9356228849868,-52.8176072531345,-52.6950348156857,
-52.5771660401742,-52.4547461333068,-52.3370240277007,-52.2147564580623,
-52.0971808358888,-51.9750654101091,-51.8576360848382,-51.7356726095103,
-51.7322148856786),.UNSPECIFIED.);
#388=B_SPLINE_CURVE_WITH_KNOTS('',3,(#35285,#35286,#35287,#35288,#35289,
#35290,#35291,#35292,#35293,#35294,#35295,#35296,#35297,#35298,#35299,#35300,
#35301,#35302,#35303,#35304,#35305,#35306,#35307,#35308,#35309,#35310,#35311,
#35312,#35313,#35314,#35315,#35316,#35317,#35318,#35319,#35320),
 .UNSPECIFIED.,.F.,.F.,(4,2,2,2,2,2,2,2,2,2,2,2,2,2,2,2,2,4),(-4.09558903017493,
-4.06282895703941,-3.9440060047118,-3.82896244084379,-3.71004666222381,
-3.59497345330519,-3.47596348634699,-3.360854431037,-3.24174884241533,-3.1265979441254,
-3.00739523272272,-2.8921967083926,-2.77289531047598,-2.65764359698508,
-2.53824189272868,-2.42293165109723,-2.30342797211658,-2.21008111793747),
 .UNSPECIFIED.);
#389=B_SPLINE_CURVE_WITH_KNOTS('',3,(#35327,#35328,#35329,#35330,#35331,
#35332,#35333,#35334,#35335,#35336,#35337,#35338,#35339,#35340,#35341,#35342,
#35343,#35344,#35345,#35346,#35347,#35348,#35349,#35350,#35351,#35352,#35353,
#35354,#35355,#35356,#35357,#35358),.UNSPECIFIED.,.F.,.F.,(4,2,2,2,2,2,
2,2,2,2,2,2,2,2,2,4),(-55.2720782428214,-55.1926108670175,-55.1144496740328,
-54.9951040192258,-54.8711501794093,-54.7519530597782,-54.6281534924038,
-54.5091047211471,-54.3854592323477,-54.266558622755,-54.1430670187691,
-54.0243143842106,-53.9009764713722,-53.7823716252871,-53.6591872100146,
-53.6557025845032),.UNSPECIFIED.);
#390=B_SPLINE_CURVE_WITH_KNOTS('',3,(#35359,#35360,#35361,#35362,#35363,
#35364,#35365,#35366,#35367,#35368,#35369,#35370,#35371,#35372,#35373,#35374,
#35375,#35376,#35377,#35378,#35379,#35380,#35381,#35382,#35383,#35384,#35385,
#35386,#35387,#35388,#35389,#35390,#35391,#35392,#35393,#35394),
 .UNSPECIFIED.,.F.,.F.,(4,2,2,2,2,2,2,2,2,2,2,2,2,2,2,2,2,4),(-2.21008111793747,
-2.18805408967434,-2.0684467272563,-1.9530043179717,-1.83329153171217,-1.71777593488302,
-1.59795596147469,-1.48236273898472,-1.36243380093483,-1.24675873327631,
-1.12671904736753,-1.0109581286233,-0.890805913968434,-0.774955345935989,
-0.654688831510368,-0.538745017138309,-0.418362448705376,-0.317026523413959),
 .UNSPECIFIED.);
#391=B_SPLINE_CURVE_WITH_KNOTS('',3,(#35405,#35406,#35407,#35408,#35409,
#35410,#35411,#35412,#35413,#35414,#35415,#35416,#35417,#35418,#35419,#35420,
#35421,#35422,#35423,#35424,#35425,#35426,#35427,#35428,#35429,#35430,#35431,
#35432,#35433,#35434,#35435,#35436),.UNSPECIFIED.,.F.,.F.,(4,2,2,2,2,2,
2,2,2,2,2,2,2,2,2,4),(0.,0.0392663678244995,0.0704169284194691,0.0927548217162514,
0.110721970139896,0.123565722758962,0.128289439509511,0.131295508607438,
0.134067308634044,0.137660564724108,0.145063726347613,0.161462983996547,
0.177979987307193,0.198867571223351,0.226369846271957,0.257489265746057),
 .UNSPECIFIED.);
#392=B_SPLINE_CURVE_WITH_KNOTS('',3,(#35440,#35441,#35442,#35443,#35444,
#35445,#35446,#35447,#35448,#35449,#35450,#35451,#35452,#35453,#35454,#35455,
#35456,#35457,#35458,#35459,#35460,#35461,#35462,#35463,#35464,#35465,#35466,
#35467,#35468,#35469,#35470,#35471),.UNSPECIFIED.,.F.,.F.,(4,2,2,2,2,2,
2,2,2,2,2,2,2,2,2,4),(0.,0.0392663678249377,0.0704169284194495,0.0927548217152616,
0.110721970138253,0.123565722756902,0.12828943950701,0.131295508605003,
0.134067308631639,0.137660564721307,0.145063726344776,0.161462983993541,
0.177979987304027,0.198867571220078,0.226369846268986,0.257489265743641),
 .UNSPECIFIED.);
#393=B_SPLINE_CURVE_WITH_KNOTS('',3,(#35476,#35477,#35478,#35479,#35480,
#35481,#35482,#35483,#35484,#35485,#35486,#35487,#35488,#35489,#35490,#35491,
#35492,#35493,#35494,#35495,#35496,#35497,#35498,#35499,#35500,#35501,#35502,
#35503,#35504,#35505,#35506,#35507),.UNSPECIFIED.,.F.,.F.,(4,2,2,2,2,2,
2,2,2,2,2,2,2,2,2,4),(0.,0.039266367824589,0.0704169284199113,0.092754821717152,
0.110721970141282,0.123565722760872,0.128289439511348,0.131295508609272,
0.134067308635804,0.137660564725569,0.145063726349089,0.161462983998042,
0.177979987308742,0.198867571225001,0.22636984627417,0.257489265748717),
 .UNSPECIFIED.);
#394=B_SPLINE_CURVE_WITH_KNOTS('',3,(#35511,#35512,#35513,#35514,#35515,
#35516,#35517,#35518,#35519,#35520,#35521,#35522,#35523,#35524,#35525,#35526,
#35527,#35528,#35529,#35530,#35531,#35532,#35533,#35534,#35535,#35536,#35537,
#35538,#35539,#35540,#35541,#35542),.UNSPECIFIED.,.F.,.F.,(4,2,2,2,2,2,
2,2,2,2,2,2,2,2,2,4),(0.,0.0392663678249047,0.0704169284198803,0.0927548217163086,
0.110721970139767,0.123565722758766,0.128289439509206,0.13129550860702,
0.134067308633502,0.137660564723442,0.145063726347079,0.161462983996174,
0.177979987306964,0.198867571223311,0.226369846272921,0.257489265748311),
 .UNSPECIFIED.);
#395=B_SPLINE_CURVE_WITH_KNOTS('',3,(#35547,#35548,#35549,#35550,#35551,
#35552,#35553,#35554,#35555,#35556,#35557,#35558,#35559,#35560,#35561,#35562,
#35563,#35564,#35565,#35566,#35567,#35568,#35569,#35570,#35571,#35572,#35573,
#35574,#35575,#35576,#35577,#35578),.UNSPECIFIED.,.F.,.F.,(4,2,2,2,2,2,
2,2,2,2,2,2,2,2,2,4),(0.,0.0392663678248331,0.0704169284201615,0.0927548217171289,
0.110721970141034,0.123565722760465,0.128289439510992,0.131295508609155,
0.134067308635896,0.137660564725619,0.145063726348897,0.161462983997348,
0.177979987307562,0.198867571223244,0.226369846271105,0.257489265744014),
 .UNSPECIFIED.);
#396=B_SPLINE_CURVE_WITH_KNOTS('',3,(#35582,#35583,#35584,#35585,#35586,
#35587,#35588,#35589,#35590,#35591,#35592,#35593,#35594,#35595,#35596,#35597,
#35598,#35599,#35600,#35601,#35602,#35603,#35604,#35605,#35606,#35607,#35608,
#35609,#35610,#35611,#35612,#35613),.UNSPECIFIED.,.F.,.F.,(4,2,2,2,2,2,
2,2,2,2,2,2,2,2,2,4),(0.,0.0392663678247495,0.070416928419445,0.0927548217155992,
0.110721970138876,0.123565722757605,0.128289439508189,0.131295508606264,
0.134067308632887,0.137660564722685,0.145063726346118,0.161462983994792,
0.177979987305081,0.198867571220603,0.226369846268855,0.257489265742627),
 .UNSPECIFIED.);
#397=B_SPLINE_CURVE_WITH_KNOTS('',3,(#35618,#35619,#35620,#35621,#35622,
#35623,#35624,#35625,#35626,#35627,#35628,#35629,#35630,#35631,#35632,#35633,
#35634,#35635,#35636,#35637,#35638,#35639,#35640,#35641,#35642,#35643,#35644,
#35645,#35646,#35647,#35648,#35649),.UNSPECIFIED.,.F.,.F.,(4,2,2,2,2,2,
2,2,2,2,2,2,2,2,2,4),(0.,0.0392663678249739,0.0704169284201815,0.0927548217168303,
0.110721970140497,0.123565722759709,0.12828943951013,0.131295508608142,
0.134067308634776,0.137660564724678,0.145063726348717,0.161462983998648,
0.17797998731033,0.198867571227874,0.22636984627903,0.257489265756248),
 .UNSPECIFIED.);
#398=B_SPLINE_CURVE_WITH_KNOTS('',3,(#35653,#35654,#35655,#35656,#35657,
#35658,#35659,#35660,#35661,#35662,#35663,#35664,#35665,#35666,#35667,#35668,
#35669,#35670,#35671,#35672,#35673,#35674,#35675,#35676,#35677,#35678,#35679,
#35680,#35681,#35682,#35683,#35684),.UNSPECIFIED.,.F.,.F.,(4,2,2,2,2,2,
2,2,2,2,2,2,2,2,2,4),(0.,0.0392663678247806,0.0704169284192398,0.0927548217150881,
0.110721970138062,0.123565722756726,0.128289439506608,0.131295508604434,
0.134067308631067,0.137660564720986,0.145063726344604,0.161462983993715,
0.177979987304472,0.198867571220671,0.2263698462694,0.257489265743336),
 .UNSPECIFIED.);
#399=B_SPLINE_CURVE_WITH_KNOTS('',3,(#35689,#35690,#35691,#35692,#35693,
#35694,#35695,#35696,#35697,#35698,#35699,#35700,#35701,#35702,#35703,#35704,
#35705,#35706,#35707,#35708,#35709,#35710,#35711,#35712,#35713,#35714,#35715,
#35716,#35717,#35718,#35719,#35720),.UNSPECIFIED.,.F.,.F.,(4,2,2,2,2,2,
2,2,2,2,2,2,2,2,2,4),(0.,0.0392663678244778,0.0704169284194323,0.0927548217161555,
0.110721970139643,0.123565722758622,0.128289439508742,0.131295508606697,
0.134067308633816,0.137660564725199,0.145063726351016,0.161462984005015,
0.177979987320616,0.198867571242853,0.226369846299339,0.257489265781862),
 .UNSPECIFIED.);
#400=B_SPLINE_CURVE_WITH_KNOTS('',3,(#35724,#35725,#35726,#35727,#35728,
#35729,#35730,#35731,#35732,#35733,#35734,#35735,#35736,#35737,#35738,#35739,
#35740,#35741,#35742,#35743,#35744,#35745,#35746,#35747,#35748,#35749,#35750,
#35751,#35752,#35753,#35754,#35755),.UNSPECIFIED.,.F.,.F.,(4,2,2,2,2,2,
2,2,2,2,2,2,2,2,2,4),(0.,0.0392663678248244,0.0704169284195352,0.0927548217156887,
0.110721970139069,0.123565722757938,0.128289439508065,0.131295508606377,
0.134067308633623,0.137660564724286,0.145063726348926,0.161462984000236,
0.177979987313331,0.198867571232472,0.226369846285091,0.257489265763111),
 .UNSPECIFIED.);
#401=B_SPLINE_CURVE_WITH_KNOTS('',3,(#35760,#35761,#35762,#35763,#35764,
#35765,#35766,#35767,#35768,#35769,#35770,#35771,#35772,#35773,#35774,#35775,
#35776,#35777,#35778,#35779,#35780,#35781,#35782,#35783,#35784,#35785,#35786,
#35787,#35788,#35789,#35790,#35791),.UNSPECIFIED.,.F.,.F.,(4,2,2,2,2,2,
2,2,2,2,2,2,2,2,2,4),(0.,0.0392663678249251,0.070416928419892,0.0927548217161836,
0.110721970139611,0.123565722758602,0.128289439508551,0.131295508606161,
0.13406730863253,0.137660564722374,0.145063726346409,0.161462983995986,
0.177979987307282,0.198867571224163,0.226369846273867,0.257489265749124),
 .UNSPECIFIED.);
#402=B_SPLINE_CURVE_WITH_KNOTS('',3,(#35795,#35796,#35797,#35798,#35799,
#35800,#35801,#35802,#35803,#35804,#35805,#35806,#35807,#35808,#35809,#35810,
#35811,#35812,#35813,#35814,#35815,#35816,#35817,#35818,#35819,#35820,#35821,
#35822,#35823,#35824,#35825,#35826),.UNSPECIFIED.,.F.,.F.,(4,2,2,2,2,2,
2,2,2,2,2,2,2,2,2,4),(0.,0.0392663678246274,0.0704169284197599,0.0927548217167053,
0.110721970140675,0.123565722759913,0.128289439510793,0.131295508608582,
0.134067308634807,0.137660564724331,0.145063726347116,0.161462983994171,
0.177979987302965,0.198867571216829,0.226369846262802,0.257489265733735),
 .UNSPECIFIED.);
#403=B_SPLINE_CURVE_WITH_KNOTS('',3,(#35831,#35832,#35833,#35834,#35835,
#35836,#35837,#35838,#35839,#35840,#35841,#35842,#35843,#35844,#35845,#35846,
#35847,#35848,#35849,#35850,#35851,#35852,#35853,#35854,#35855,#35856,#35857,
#35858,#35859,#35860,#35861,#35862),.UNSPECIFIED.,.F.,.F.,(4,2,2,2,2,2,
2,2,2,2,2,2,2,2,2,4),(0.,0.0392663678247802,0.070416928419353,0.0927548217152033,
0.110721970137883,0.123565722756308,0.128289439505835,0.131295508603904,
0.134067308631161,0.137660564722251,0.14506372634802,0.161462984001055,
0.177979987315666,0.198867571236657,0.226369846291255,0.257489265771073),
 .UNSPECIFIED.);
#404=B_SPLINE_CURVE_WITH_KNOTS('',3,(#35866,#35867,#35868,#35869,#35870,
#35871,#35872,#35873,#35874,#35875,#35876,#35877,#35878,#35879,#35880,#35881,
#35882,#35883,#35884,#35885,#35886,#35887,#35888,#35889,#35890,#35891,#35892,
#35893,#35894,#35895,#35896,#35897),.UNSPECIFIED.,.F.,.F.,(4,2,2,2,2,2,
2,2,2,2,2,2,2,2,2,4),(0.,0.0392663678245154,0.0704169284191378,0.0927548217152303,
0.110721970138229,0.123565722756741,0.128289439506368,0.131295508603649,
0.134067308629744,0.137660564719498,0.145063726343503,0.161462983992689,
0.177979987303389,0.198867571219121,0.226369846267092,0.257489265740257),
 .UNSPECIFIED.);
#405=B_SPLINE_CURVE_WITH_KNOTS('',3,(#35902,#35903,#35904,#35905,#35906,
#35907,#35908,#35909,#35910,#35911,#35912,#35913,#35914,#35915,#35916,#35917,
#35918,#35919,#35920,#35921,#35922,#35923,#35924,#35925,#35926,#35927,#35928,
#35929,#35930,#35931,#35932,#35933),.UNSPECIFIED.,.F.,.F.,(4,2,2,2,2,2,
2,2,2,2,2,2,2,2,2,4),(0.,0.0392663678246403,0.0704169284196593,0.0927548217162621,
0.110721970139792,0.123565722758691,0.128289439509469,0.131295508607455,
0.134067308634163,0.137660564724622,0.145063726348764,0.161462983999486,
0.177979987311735,0.198867571229894,0.226369846281758,0.25748926576032),
 .UNSPECIFIED.);
#406=B_SPLINE_CURVE_WITH_KNOTS('',3,(#35937,#35938,#35939,#35940,#35941,
#35942,#35943,#35944,#35945,#35946,#35947,#35948,#35949,#35950,#35951,#35952,
#35953,#35954,#35955,#35956,#35957,#35958,#35959,#35960,#35961,#35962,#35963,
#35964,#35965,#35966,#35967,#35968),.UNSPECIFIED.,.F.,.F.,(4,2,2,2,2,2,
2,2,2,2,2,2,2,2,2,4),(0.,0.0392663678247903,0.070416928419749,0.0927548217163387,
0.110721970139937,0.123565722758935,0.128289439509696,0.131295508608072,
0.134067308634654,0.137660564723633,0.145063726346522,0.161462983994072,
0.177979987303378,0.198867571217868,0.226369846264756,0.257489265736797),
 .UNSPECIFIED.);
#407=B_SPLINE_CURVE_WITH_KNOTS('',3,(#35973,#35974,#35975,#35976,#35977,
#35978,#35979,#35980,#35981,#35982,#35983,#35984,#35985,#35986,#35987,#35988,
#35989,#35990,#35991,#35992,#35993,#35994,#35995,#35996,#35997,#35998,#35999,
#36000,#36001,#36002,#36003,#36004),.UNSPECIFIED.,.F.,.F.,(4,2,2,2,2,2,
2,2,2,2,2,2,2,2,2,4),(0.,0.0392663678247125,0.0704169284195073,0.0927548217158198,
0.110721970139137,0.123565722757943,0.128289439508104,0.131295508606656,
0.134067308633928,0.137660564724143,0.145063726348696,0.161462983999483,
0.17797998731199,0.198867571230429,0.226369846281902,0.257489265758881),
 .UNSPECIFIED.);
#408=B_SPLINE_CURVE_WITH_KNOTS('',3,(#36008,#36009,#36010,#36011,#36012,
#36013,#36014,#36015,#36016,#36017,#36018,#36019,#36020,#36021,#36022,#36023,
#36024,#36025,#36026,#36027,#36028,#36029,#36030,#36031,#36032,#36033,#36034,
#36035,#36036,#36037,#36038,#36039),.UNSPECIFIED.,.F.,.F.,(4,2,2,2,2,2,
2,2,2,2,2,2,2,2,2,4),(0.,0.0392663678246693,0.0704169284192301,0.0927548217150732,
0.110721970137704,0.123565722755857,0.128289439505946,0.131295508603737,
0.134067308630246,0.13766056472024,0.145063726344291,0.161462983993872,
0.177979987304981,0.198867571221343,0.226369846269783,0.257489265742993),
 .UNSPECIFIED.);
#409=B_SPLINE_CURVE_WITH_KNOTS('',3,(#36044,#36045,#36046,#36047,#36048,
#36049,#36050,#36051,#36052,#36053,#36054,#36055,#36056,#36057,#36058,#36059,
#36060,#36061,#36062,#36063,#36064,#36065,#36066,#36067,#36068,#36069,#36070,
#36071,#36072,#36073,#36074,#36075),.UNSPECIFIED.,.F.,.F.,(4,2,2,2,2,2,
2,2,2,2,2,2,2,2,2,4),(0.,0.0392663678249069,0.0704169284199938,0.0927548217165904,
0.110721970140226,0.123565722759382,0.128289439509785,0.131295508607764,
0.13406730863429,0.137660564723914,0.145063726347582,0.161462983996786,
0.177979987307717,0.198867571224335,0.226369846273865,0.257489265748956),
 .UNSPECIFIED.);
#410=B_SPLINE_CURVE_WITH_KNOTS('',3,(#36079,#36080,#36081,#36082,#36083,
#36084,#36085,#36086,#36087,#36088,#36089,#36090,#36091,#36092,#36093,#36094,
#36095,#36096,#36097,#36098,#36099,#36100,#36101,#36102,#36103,#36104,#36105,
#36106,#36107,#36108,#36109,#36110),.UNSPECIFIED.,.F.,.F.,(4,2,2,2,2,2,
2,2,2,2,2,2,2,2,2,4),(0.,0.039266367824699,0.0704169284194923,0.0927548217158646,
0.11072197013936,0.123565722758493,0.128289439508746,0.131295508606819,
0.134067308633445,0.13766056472298,0.145063726346669,0.161462983996177,
0.177979987307315,0.198867571224074,0.226369846273922,0.257489265749371),
 .UNSPECIFIED.);
#411=B_SPLINE_CURVE_WITH_KNOTS('',3,(#36120,#36121,#36122,#36123,#36124,
#36125,#36126,#36127,#36128,#36129,#36130,#36131,#36132,#36133,#36134,#36135,
#36136,#36137,#36138,#36139,#36140,#36141,#36142,#36143,#36144,#36145,#36146,
#36147,#36148,#36149,#36150,#36151),.UNSPECIFIED.,.F.,.F.,(4,2,2,2,2,2,
2,2,2,2,2,2,2,2,2,4),(-1.76634793841595E-15,0.0392663678245224,0.0704169284190363,
0.0927548217151552,0.110721970138219,0.123565722756832,0.128289439506975,
0.131295508604955,0.134067308631658,0.137660564721908,0.145063726347255,
0.161462983999379,0.177979987313175,0.198867571232894,0.226369846286481,
0.257489265765706),.UNSPECIFIED.);
#412=B_SPLINE_CURVE_WITH_KNOTS('',3,(#36155,#36156,#36157,#36158,#36159,
#36160,#36161,#36162,#36163,#36164,#36165,#36166,#36167,#36168,#36169,#36170,
#36171,#36172,#36173,#36174,#36175,#36176,#36177,#36178,#36179,#36180,#36181,
#36182,#36183,#36184,#36185,#36186),.UNSPECIFIED.,.F.,.F.,(4,2,2,2,2,2,
2,2,2,2,2,2,2,2,2,4),(-3.43854363132254E-15,0.0392663678246992,0.0704169284198385,
0.0927548217167047,0.110721970140455,0.123565722759784,0.128289439510127,
0.131295508608258,0.134067308635215,0.137660564725771,0.145063726350863,
0.16146298400288,0.177979987316548,0.198867571236671,0.226369846290545,
0.257489265770492),.UNSPECIFIED.);
#413=B_SPLINE_CURVE_WITH_KNOTS('',3,(#36190,#36191,#36192,#36193,#36194,
#36195,#36196,#36197,#36198,#36199,#36200,#36201,#36202,#36203,#36204,#36205,
#36206,#36207,#36208,#36209,#36210,#36211,#36212,#36213,#36214,#36215,#36216,
#36217,#36218,#36219,#36220,#36221),.UNSPECIFIED.,.F.,.F.,(4,2,2,2,2,2,
2,2,2,2,2,2,2,2,2,4),(-3.34439138581297E-15,0.0392663678246232,0.0704169284196317,
0.0927548217162855,0.110721970139993,0.123565722759132,0.128289439510069,
0.13129550860811,0.134067308634763,0.137660564724976,0.1450637263486,0.161462983997844,
0.177979987308744,0.198867571225209,0.226369846274388,0.257489265749007),
 .UNSPECIFIED.);
#414=B_SPLINE_CURVE_WITH_KNOTS('',3,(#36225,#36226,#36227,#36228,#36229,
#36230,#36231,#36232,#36233,#36234,#36235,#36236,#36237,#36238,#36239,#36240,
#36241,#36242,#36243,#36244,#36245,#36246,#36247,#36248,#36249,#36250,#36251,
#36252,#36253,#36254,#36255,#36256),.UNSPECIFIED.,.F.,.F.,(4,2,2,2,2,2,
2,2,2,2,2,2,2,2,2,4),(-3.43854363132217E-15,0.0392663678249148,0.0704169284200044,
0.0927548217166559,0.110721970140529,0.123565722759803,0.128289439510254,
0.13129550860835,0.134067308634935,0.137660564724413,0.145063726347793,
0.161462983996495,0.177979987306919,0.198867571222842,0.226369846271352,
0.257489265745074),.UNSPECIFIED.);
#415=B_SPLINE_CURVE_WITH_KNOTS('',3,(#36260,#36261,#36262,#36263,#36264,
#36265,#36266,#36267,#36268,#36269,#36270,#36271,#36272,#36273,#36274,#36275,
#36276,#36277,#36278,#36279,#36280,#36281,#36282,#36283,#36284,#36285,#36286,
#36287,#36288,#36289,#36290,#36291),.UNSPECIFIED.,.F.,.F.,(4,2,2,2,2,2,
2,2,2,2,2,2,2,2,2,4),(-1.76634793841593E-15,0.0392663678246619,0.070416928419432,
0.0927548217157895,0.110721970139278,0.123565722758194,0.128289439508417,
0.131295508606941,0.134067308634171,0.137660564724305,0.1450637263484,0.161462983998334,
0.177979987309968,0.198867571227245,0.226369846278035,0.257489265754873),
 .UNSPECIFIED.);
#416=B_SPLINE_CURVE_WITH_KNOTS('',3,(#36295,#36296,#36297,#36298,#36299,
#36300,#36301,#36302,#36303,#36304,#36305,#36306,#36307,#36308,#36309,#36310,
#36311,#36312,#36313,#36314,#36315,#36316,#36317,#36318,#36319,#36320,#36321,
#36322,#36323,#36324,#36325,#36326),.UNSPECIFIED.,.F.,.F.,(4,2,2,2,2,2,
2,2,2,2,2,2,2,2,2,4),(-3.25023914030354E-15,0.0392663678248276,0.0704169284192996,
0.092754821715151,0.110721970137982,0.123565722756635,0.128289439506694,
0.131295508604321,0.13406730863081,0.137660564720951,0.145063726344476,
0.161462983993191,0.177979987303611,0.198867571219355,0.226369846267676,
0.257489265741455),.UNSPECIFIED.);
#417=B_SPLINE_CURVE_WITH_KNOTS('',3,(#36330,#36331,#36332,#36333,#36334,
#36335,#36336,#36337,#36338,#36339,#36340,#36341,#36342,#36343,#36344,#36345,
#36346,#36347,#36348,#36349,#36350,#36351,#36352,#36353,#36354,#36355,#36356,
#36357,#36358,#36359,#36360,#36361),.UNSPECIFIED.,.F.,.F.,(4,2,2,2,2,2,
2,2,2,2,2,2,2,2,2,4),(-3.43854363132254E-15,0.0392663678247849,0.0704169284203094,
0.0927548217175492,0.110721970141637,0.123565722761111,0.128289439511682,
0.131295508609654,0.134067308636262,0.137660564726202,0.145063726349868,
0.161462983999319,0.17797998731052,0.198867571227385,0.226369846277203,
0.257489265752561),.UNSPECIFIED.);
#418=B_SPLINE_CURVE_WITH_KNOTS('',3,(#36365,#36366,#36367,#36368,#36369,
#36370,#36371,#36372,#36373,#36374,#36375,#36376,#36377,#36378,#36379,#36380,
#36381,#36382,#36383,#36384,#36385,#36386,#36387,#36388,#36389,#36390,#36391,
#36392,#36393,#36394,#36395,#36396),.UNSPECIFIED.,.F.,.F.,(4,2,2,2,2,2,
2,2,2,2,2,2,2,2,2,4),(-3.62684812234152E-15,0.0392663678249345,0.070416928420165,
0.0927548217169184,0.110721970140689,0.12356572276004,0.128289439510604,
0.131295508608354,0.134067308634811,0.137660564724923,0.145063726348958,
0.161462983999017,0.177979987310905,0.198867571228708,0.226369846279955,
0.257489265757467),.UNSPECIFIED.);
#419=B_SPLINE_CURVE_WITH_KNOTS('',3,(#36410,#36411,#36412,#36413,#36414,
#36415,#36416,#36417,#36418,#36419,#36420,#36421,#36422,#36423,#36424,#36425,
#36426,#36427,#36428,#36429,#36430,#36431,#36432,#36433,#36434,#36435,#36436,
#36437,#36438,#36439,#36440,#36441),.UNSPECIFIED.,.F.,.F.,(4,2,2,2,2,2,
2,2,2,2,2,2,2,2,2,4),(-3.62684812234151E-15,0.0392663678245326,0.0704169284186608,
0.0927548217142498,0.110721970136877,0.123565722755316,0.128289439504875,
0.131295508602739,0.134067308629719,0.137660564720433,0.145063726345226,
0.161462983996599,0.177979987309569,0.198867571228362,0.226369846280901,
0.257489265759448),.UNSPECIFIED.);
#420=B_SPLINE_CURVE_WITH_KNOTS('',3,(#36445,#36446,#36447,#36448,#36449,
#36450,#36451,#36452,#36453,#36454,#36455,#36456,#36457,#36458,#36459,#36460,
#36461,#36462,#36463,#36464,#36465,#36466,#36467,#36468,#36469,#36470,#36471,
#36472,#36473,#36474,#36475,#36476),.UNSPECIFIED.,.F.,.F.,(4,2,2,2,2,2,
2,2,2,2,2,2,2,2,2,4),(-5.29904381524748E-15,0.0392663678245013,0.0704169284189458,
0.0927548217149502,0.110721970138046,0.123565722756779,0.128289439506874,
0.131295508604914,0.134067308631792,0.137660564721975,0.145063726345566,
0.161462983994717,0.177979987305542,0.198867571221693,0.226369846270547,
0.257489265744874),.UNSPECIFIED.);
#421=B_SPLINE_CURVE_WITH_KNOTS('',3,(#36480,#36481,#36482,#36483,#36484,
#36485,#36486,#36487,#36488,#36489,#36490,#36491,#36492,#36493,#36494,#36495,
#36496,#36497,#36498,#36499,#36500,#36501,#36502,#36503,#36504,#36505,#36506,
#36507,#36508,#36509,#36510,#36511),.UNSPECIFIED.,.F.,.F.,(4,2,2,2,2,2,
2,2,2,2,2,2,2,2,2,4),(-1.67219569290643E-15,0.0392663678247147,0.0704169284193986,
0.0927548217155684,0.110721970138799,0.123565722757588,0.128289439508,0.131295508606025,
0.134067308632753,0.13766056472281,0.145063726346428,0.161462983995307,
0.177979987305903,0.198867571221865,0.22636984627118,0.257489265746664),
 .UNSPECIFIED.);
#422=B_SPLINE_CURVE_WITH_KNOTS('',3,(#36515,#36516,#36517,#36518,#36519,
#36520,#36521,#36522,#36523,#36524,#36525,#36526,#36527,#36528,#36529,#36530,
#36531,#36532,#36533,#36534,#36535,#36536,#36537,#36538,#36539,#36540,#36541,
#36542,#36543,#36544,#36545,#36546),.UNSPECIFIED.,.F.,.F.,(4,2,2,2,2,2,
2,2,2,2,2,2,2,2,2,4),(-3.53269587683169E-15,0.0392663678247277,0.0704169284193875,
0.0927548217155201,0.11072197013873,0.123565722757556,0.128289439507877,
0.13129550860585,0.134067308632342,0.137660564721825,0.145063726345164,
0.161462983993392,0.17797998730333,0.198867571218531,0.226369846266786,
0.2574892657409),.UNSPECIFIED.);
#423=B_SPLINE_CURVE_WITH_KNOTS('',3,(#36550,#36551,#36552,#36553,#36554,
#36555,#36556,#36557,#36558,#36559,#36560,#36561,#36562,#36563,#36564,#36565,
#36566,#36567,#36568,#36569,#36570,#36571,#36572,#36573,#36574,#36575,#36576,
#36577,#36578,#36579,#36580,#36581),.UNSPECIFIED.,.F.,.F.,(4,2,2,2,2,2,
2,2,2,2,2,2,2,2,2,4),(0.,0.0392663678247719,0.0704169284195709,0.0927548217157682,
0.110721970138893,0.123565722757687,0.128289439507762,0.131295508605502,
0.134067308632007,0.137660564721959,0.145063726345763,0.161462983995323,
0.177979987306524,0.198867571223098,0.226369846272715,0.257489265748122),
 .UNSPECIFIED.);
#424=B_SPLINE_CURVE_WITH_KNOTS('',3,(#36585,#36586,#36587,#36588,#36589,
#36590,#36591,#36592,#36593,#36594,#36595,#36596,#36597,#36598,#36599,#36600,
#36601,#36602,#36603,#36604,#36605,#36606,#36607,#36608,#36609,#36610,#36611,
#36612,#36613,#36614,#36615,#36616),.UNSPECIFIED.,.F.,.F.,(4,2,2,2,2,2,
2,2,2,2,2,2,2,2,2,4),(-1.76634793841592E-15,0.0392663678247361,0.0704169284199132,
0.0927548217167579,0.110721970140471,0.123565722759657,0.128289439510084,
0.131295508608104,0.134067308634866,0.137660564725111,0.145063726349294,
0.16146298399946,0.177979987311368,0.198867571229017,0.226369846280088,
0.25748926575724),.UNSPECIFIED.);
#425=B_SPLINE_CURVE_WITH_KNOTS('',3,(#36620,#36621,#36622,#36623,#36624,
#36625,#36626,#36627,#36628,#36629,#36630,#36631,#36632,#36633,#36634,#36635,
#36636,#36637,#36638,#36639,#36640,#36641,#36642,#36643,#36644,#36645,#36646,
#36647,#36648,#36649,#36650,#36651),.UNSPECIFIED.,.F.,.F.,(4,2,2,2,2,2,
2,2,2,2,2,2,2,2,2,4),(0.,0.0392663678245323,0.0704169284195438,0.0927548217162293,
0.110721970139834,0.12356572275881,0.128289439508994,0.13129550860705,0.134067308633916,
0.13766056472422,0.145063726348449,0.16146298399857,0.177979987310414,0.198867571227846,
0.226369846278175,0.257489265753618),.UNSPECIFIED.);
#426=B_SPLINE_CURVE_WITH_KNOTS('',3,(#36655,#36656,#36657,#36658,#36659,
#36660,#36661,#36662,#36663,#36664,#36665,#36666,#36667,#36668,#36669,#36670,
#36671,#36672,#36673,#36674,#36675,#36676,#36677,#36678,#36679,#36680,#36681,
#36682,#36683,#36684,#36685,#36686),.UNSPECIFIED.,.F.,.F.,(4,2,2,2,2,2,
2,2,2,2,2,2,2,2,2,4),(-1.67219569290647E-15,0.0392663678247851,0.0704169284199364,
0.0927548217166158,0.110721970140177,0.123565722759255,0.128289439509636,
0.13129550860772,0.134067308634613,0.137660564724923,0.145063726348494,
0.161462983997478,0.177979987308109,0.198867571224169,0.226369846273075,
0.257489265747719),.UNSPECIFIED.);
#427=B_SPLINE_CURVE_WITH_KNOTS('',3,(#36701,#36702,#36703,#36704,#36705,
#36706,#36707,#36708,#36709,#36710,#36711,#36712,#36713,#36714,#36715,#36716,
#36717,#36718,#36719,#36720,#36721,#36722,#36723,#36724,#36725,#36726,#36727,
#36728,#36729,#36730,#36731,#36732),.UNSPECIFIED.,.F.,.F.,(4,2,2,2,2,2,
2,2,2,2,2,2,2,2,2,4),(0.,0.0392663678244286,0.0704169284192886,0.0927548217159949,
0.110721970139649,0.123565722758812,0.128289439509101,0.131295508607411,
0.134067308634294,0.137660564723937,0.145063726347504,0.161462983996596,
0.177979987307378,0.198867571223475,0.22636984627213,0.257489265746436),
 .UNSPECIFIED.);
#428=B_SPLINE_CURVE_WITH_KNOTS('',3,(#36736,#36737,#36738,#36739,#36740,
#36741,#36742,#36743,#36744,#36745,#36746,#36747,#36748,#36749,#36750,#36751,
#36752,#36753,#36754,#36755,#36756,#36757,#36758,#36759,#36760,#36761,#36762,
#36763,#36764,#36765,#36766,#36767),.UNSPECIFIED.,.F.,.F.,(4,2,2,2,2,2,
2,2,2,2,2,2,2,2,2,4),(-1.67219569290635E-15,0.0392663678244886,0.0704169284192001,
0.0927548217156716,0.11072197013908,0.123565722758101,0.128289439508155,
0.131295508605815,0.134067308632236,0.13766056472206,0.145063726345475,
0.161462983994193,0.177979987304618,0.19886757122036,0.226369846268546,
0.257489265742088),.UNSPECIFIED.);
#429=B_SPLINE_CURVE_WITH_KNOTS('',3,(#36771,#36772,#36773,#36774,#36775,
#36776,#36777,#36778,#36779,#36780,#36781,#36782,#36783,#36784,#36785,#36786,
#36787,#36788,#36789,#36790,#36791,#36792,#36793,#36794,#36795,#36796,#36797,
#36798,#36799,#36800,#36801,#36802),.UNSPECIFIED.,.F.,.F.,(4,2,2,2,2,2,
2,2,2,2,2,2,2,2,2,4),(-3.43854363132256E-15,0.0392663678247843,0.0704169284198121,
0.0927548217163949,0.110721970139939,0.123565722758948,0.128289439509206,
0.131295508607079,0.134067308633498,0.137660564722997,0.145063726346605,
0.161462983995843,0.177979987306685,0.198867571223128,0.226369846272286,
0.257489265746815),.UNSPECIFIED.);
#430=B_SPLINE_CURVE_WITH_KNOTS('',3,(#36806,#36807,#36808,#36809,#36810,
#36811,#36812,#36813,#36814,#36815,#36816,#36817,#36818,#36819,#36820,#36821,
#36822,#36823,#36824,#36825,#36826,#36827,#36828,#36829,#36830,#36831,#36832,
#36833,#36834,#36835,#36836,#36837),.UNSPECIFIED.,.F.,.F.,(4,2,2,2,2,2,
2,2,2,2,2,2,2,2,2,4),(3.62684812234147E-15,0.0392663678247153,0.0704169284195201,
0.0927548217158921,0.110721970139242,0.12356572275814,0.128289439508467,
0.131295508606043,0.134067308632338,0.137660564722272,0.145063726345893,
0.161462983995342,0.177979987306438,0.198867571223068,0.226369846272216,
0.25748926574638),.UNSPECIFIED.);
#431=B_SPLINE_CURVE_WITH_KNOTS('',3,(#36841,#36842,#36843,#36844,#36845,
#36846,#36847,#36848,#36849,#36850,#36851,#36852,#36853,#36854,#36855,#36856,
#36857,#36858,#36859,#36860,#36861,#36862,#36863,#36864,#36865,#36866,#36867,
#36868,#36869,#36870,#36871,#36872),.UNSPECIFIED.,.F.,.F.,(4,2,2,2,2,2,
2,2,2,2,2,2,2,2,2,4),(1.76634793841596E-15,0.0392663678246221,0.070416928418827,
0.0927548217143397,0.110721970136809,0.123565722754925,0.128289439504577,
0.131295508601993,0.134067308628616,0.137660564719576,0.145063726344241,
0.161462983995214,0.177979987307686,0.198867571225782,0.226369846276743,
0.257489265752939),.UNSPECIFIED.);
#432=B_SPLINE_CURVE_WITH_KNOTS('',3,(#36876,#36877,#36878,#36879,#36880,
#36881,#36882,#36883,#36884,#36885,#36886,#36887,#36888,#36889,#36890,#36891,
#36892,#36893,#36894,#36895,#36896,#36897,#36898,#36899,#36900,#36901,#36902,
#36903,#36904,#36905,#36906,#36907),.UNSPECIFIED.,.F.,.F.,(4,2,2,2,2,2,
2,2,2,2,2,2,2,2,2,4),(1.67219569290649E-15,0.0392663678248474,0.0704169284201005,
0.0927548217170368,0.110721970141041,0.123565722760672,0.128289439511198,
0.131295508609165,0.134067308635788,0.137660564725585,0.145063726348477,
0.161462983996445,0.177979987306176,0.198867571221256,0.226369846269141,
0.257489265742917),.UNSPECIFIED.);
#433=B_SPLINE_CURVE_WITH_KNOTS('',3,(#36911,#36912,#36913,#36914,#36915,
#36916,#36917,#36918,#36919,#36920,#36921,#36922,#36923,#36924,#36925,#36926,
#36927,#36928,#36929,#36930,#36931,#36932,#36933,#36934,#36935,#36936,#36937,
#36938,#36939,#36940,#36941,#36942),.UNSPECIFIED.,.F.,.F.,(4,2,2,2,2,2,
2,2,2,2,2,2,2,2,2,4),(1.57804344739692E-15,0.0392663678243967,0.0704169284187512,
0.0927548217148942,0.110721970138087,0.123565722756915,0.128289439507759,
0.131295508605752,0.134067308632248,0.137660564721969,0.145063726344741,
0.161462983992119,0.177979987301147,0.198867571215294,0.226369846261679,
0.257489265732903),.UNSPECIFIED.);
#434=B_SPLINE_CURVE_WITH_KNOTS('',3,(#36946,#36947,#36948,#36949,#36950,
#36951,#36952,#36953,#36954,#36955,#36956,#36957,#36958,#36959,#36960,#36961,
#36962,#36963,#36964,#36965,#36966,#36967,#36968,#36969,#36970,#36971,#36972,
#36973,#36974,#36975,#36976,#36977),.UNSPECIFIED.,.F.,.F.,(4,2,2,2,2,2,
2,2,2,2,2,2,2,2,2,4),(1.48389120188744E-15,0.0392663678246362,0.0704169284193307,
0.0927548217156513,0.11072197013894,0.123565722757702,0.128289439508219,
0.13129550860668,0.134067308633863,0.137660564724131,0.14506372634765,0.161462983996701,
0.177979987307462,0.198867571223755,0.22636984627265,0.257489265747157),
 .UNSPECIFIED.);
#435=B_SPLINE_CURVE_WITH_KNOTS('',3,(#36981,#36982,#36983,#36984,#36985,
#36986,#36987,#36988,#36989,#36990,#36991,#36992,#36993,#36994,#36995,#36996,
#36997,#36998,#36999,#37000,#37001,#37002,#37003,#37004,#37005,#37006,#37007,
#37008,#37009,#37010,#37011,#37012),.UNSPECIFIED.,.F.,.F.,(4,2,2,2,2,2,
2,2,2,2,2,2,2,2,2,4),(-1.86050018392547E-15,0.0392663678246196,0.070416928419344,
0.0927548217158401,0.110721970139278,0.123565722758188,0.128289439508702,
0.131295508606563,0.134067308633031,0.137660564722894,0.145063726346462,
0.161462983995227,0.177979987305691,0.198867571221603,0.226369846269658,
0.257489265742502),.UNSPECIFIED.);
#436=B_SPLINE_CURVE_WITH_KNOTS('',3,(#37016,#37017,#37018,#37019,#37020,
#37021,#37022,#37023,#37024,#37025,#37026,#37027,#37028,#37029,#37030,#37031,
#37032,#37033,#37034,#37035,#37036,#37037,#37038,#37039,#37040,#37041,#37042,
#37043,#37044,#37045,#37046,#37047),.UNSPECIFIED.,.F.,.F.,(4,2,2,2,2,2,
2,2,2,2,2,2,2,2,2,4),(0.,0.039266367824605,0.0704169284192653,0.0927548217155983,
0.110721970139038,0.123565722758227,0.128289439508356,0.131295508606434,
0.134067308633204,0.137660564722963,0.145063726346308,0.161462983994947,
0.177979987305301,0.198867571221117,0.22636984626943,0.257489265742971),
 .UNSPECIFIED.);
#437=B_SPLINE_CURVE_WITH_KNOTS('',3,(#37051,#37052,#37053,#37054,#37055,
#37056,#37057,#37058,#37059,#37060,#37061,#37062,#37063,#37064,#37065,#37066,
#37067,#37068,#37069,#37070,#37071,#37072,#37073,#37074,#37075,#37076,#37077,
#37078,#37079,#37080,#37081,#37082),.UNSPECIFIED.,.F.,.F.,(4,2,2,2,2,2,
2,2,2,2,2,2,2,2,2,4),(-1.76634793841601E-15,0.0392663678246844,0.0704169284198206,
0.0927548217167689,0.110721970140703,0.123565722760151,0.128289439510863,
0.131295508609073,0.134067308635863,0.137660564725819,0.145063726349486,
0.161462983998877,0.177979987310031,0.198867571226897,0.226369846277016,
0.257489265752877),.UNSPECIFIED.);
#438=B_SPLINE_CURVE_WITH_KNOTS('',3,(#37086,#37087,#37088,#37089,#37090,
#37091,#37092,#37093,#37094,#37095,#37096,#37097,#37098,#37099,#37100,#37101,
#37102,#37103,#37104,#37105,#37106,#37107,#37108,#37109,#37110,#37111,#37112,
#37113,#37114,#37115,#37116,#37117),.UNSPECIFIED.,.F.,.F.,(4,2,2,2,2,2,
2,2,2,2,2,2,2,2,2,4),(-1.76634793841602E-15,0.0392663678249098,0.0704169284202436,
0.0927548217171559,0.110721970140946,0.123565722760192,0.128289439510643,
0.13129550860873,0.134067308635531,0.137660564725647,0.14506372634943,0.161462983998864,
0.17797998731004,0.198867571226972,0.226369846276657,0.257489265751791),
 .UNSPECIFIED.);
#439=B_SPLINE_CURVE_WITH_KNOTS('',3,(#37121,#37122,#37123,#37124,#37125,
#37126,#37127,#37128,#37129,#37130,#37131,#37132,#37133,#37134,#37135,#37136,
#37137,#37138,#37139,#37140,#37141,#37142,#37143,#37144,#37145,#37146,#37147,
#37148,#37149,#37150,#37151,#37152),.UNSPECIFIED.,.F.,.F.,(4,2,2,2,2,2,
2,2,2,2,2,2,2,2,2,4),(1.76634793841582E-15,0.0392663678245818,0.0704169284194132,
0.0927548217159401,0.110721970139461,0.123565722758553,0.128289439508967,
0.131295508606888,0.134067308633461,0.137660564723424,0.14506372634746,
0.161462983997496,0.17797998730928,0.198867571226825,0.226369846276753,
0.257489265751656),.UNSPECIFIED.);
#440=B_SPLINE_CURVE_WITH_KNOTS('',3,(#37156,#37157,#37158,#37159,#37160,
#37161,#37162,#37163,#37164,#37165,#37166,#37167,#37168,#37169,#37170,#37171,
#37172,#37173,#37174,#37175,#37176,#37177,#37178,#37179,#37180,#37181,#37182,
#37183,#37184,#37185,#37186,#37187),.UNSPECIFIED.,.F.,.F.,(4,2,2,2,2,2,
2,2,2,2,2,2,2,2,2,4),(-1.76634793841602E-15,0.0392663678247105,0.0704169284196071,
0.0927548217161623,0.110721970139774,0.123565722758804,0.128289439509258,
0.131295508607385,0.134067308634216,0.137660564724393,0.145063726348231,
0.161462983997576,0.1779799873087,0.198867571225463,0.226369846275158,0.25748926575035),
 .UNSPECIFIED.);
#441=B_SPLINE_CURVE_WITH_KNOTS('',3,(#37191,#37192,#37193,#37194,#37195,
#37196,#37197,#37198,#37199,#37200,#37201,#37202,#37203,#37204,#37205,#37206,
#37207,#37208,#37209,#37210,#37211,#37212,#37213,#37214,#37215,#37216,#37217,
#37218,#37219,#37220,#37221,#37222),.UNSPECIFIED.,.F.,.F.,(4,2,2,2,2,2,
2,2,2,2,2,2,2,2,2,4),(0.,0.039266367824639,0.0704169284196416,0.0927548217164797,
0.110721970140397,0.123565722759903,0.128289439510384,0.131295508608112,
0.134067308634667,0.137660564725083,0.145063726349291,0.16146298399955,
0.177979987311731,0.198867571229869,0.226369846281328,0.257489265758592),
 .UNSPECIFIED.);
#442=B_SPLINE_CURVE_WITH_KNOTS('',3,(#37226,#37227,#37228,#37229,#37230,
#37231,#37232,#37233,#37234,#37235,#37236,#37237,#37238,#37239,#37240,#37241,
#37242,#37243,#37244,#37245,#37246,#37247,#37248,#37249,#37250,#37251,#37252,
#37253,#37254,#37255,#37256,#37257),.UNSPECIFIED.,.F.,.F.,(4,2,2,2,2,2,
2,2,2,2,2,2,2,2,2,4),(-1.76634793841584E-15,0.0392663678248517,0.0704169284197748,
0.0927548217161432,0.110721970139464,0.123565722758405,0.128289439508459,
0.131295508606329,0.134067308633017,0.137660564723293,0.145063726348177,
0.161462983999597,0.177979987312819,0.198867571232171,0.226369846284916,
0.257489265763157),.UNSPECIFIED.);
#443=B_SPLINE_CURVE_WITH_KNOTS('',3,(#37265,#37266,#37267,#37268,#37269,
#37270,#37271,#37272,#37273,#37274),.UNSPECIFIED.,.F.,.F.,(4,2,2,2,4),(-0.317026523413959,
-0.302322031379582,-0.181822057847978,-0.0905311996482953,-9.99999998141377E-7),
 .UNSPECIFIED.);
#444=B_SPLINE_CURVE_WITH_KNOTS('',3,(#37333,#37334,#37335,#37336,#37337,
#37338,#37339,#37340,#37341,#37342,#37343,#37344,#37345,#37346),
 .UNSPECIFIED.,.F.,.F.,(4,2,2,2,2,2,4),(-0.844978516211101,-0.706255465582548,
-0.570455953228873,-0.422452321689898,-0.274454069952361,-0.138687373055613,
0.),.UNSPECIFIED.);
#445=B_SPLINE_CURVE_WITH_KNOTS('',3,(#37347,#37348,#37349,#37350,#37351,
#37352,#37353,#37354,#37355,#37356),.UNSPECIFIED.,.F.,.F.,(4,2,2,2,4),(-0.564860666687477,
-0.387918780397416,-0.216626435797941,-0.0894002839461589,0.),
 .UNSPECIFIED.);
#446=B_SPLINE_CURVE_WITH_KNOTS('',3,(#37357,#37358,#37359,#37360,#37361,
#37362,#37363,#37364,#37365,#37366),.UNSPECIFIED.,.F.,.F.,(4,2,2,2,4),(-0.305777613429687,
-0.25789998327206,-0.189518825213173,-0.0962950640176603,0.),
 .UNSPECIFIED.);
#447=B_SPLINE_CURVE_WITH_KNOTS('',3,(#37373,#37374,#37375,#37376,#37377,
#37378,#37379,#37380,#37381,#37382),.UNSPECIFIED.,.F.,.F.,(4,2,2,2,4),(-0.305777613709471,
-0.257899983501032,-0.189518825369156,-0.0962950640743464,0.),
 .UNSPECIFIED.);
#448=B_SPLINE_CURVE_WITH_KNOTS('',3,(#37384,#37385,#37386,#37387,#37388,
#37389,#37390,#37391,#37392,#37393),.UNSPECIFIED.,.F.,.F.,(4,2,2,2,4),(-0.564860671099225,
-0.387918783323875,-0.216626437248832,-0.0894002842905878,0.),
 .UNSPECIFIED.);
#449=B_SPLINE_CURVE_WITH_KNOTS('',3,(#37394,#37395,#37396,#37397,#37398,
#37399,#37400,#37401,#37402,#37403,#37404,#37405,#37406,#37407),
 .UNSPECIFIED.,.F.,.F.,(4,2,2,2,2,2,4),(-0.844959728295684,-0.706031861511686,
-0.570044179645694,-0.421929648490435,-0.273898821298179,-0.13839817385903,
0.),.UNSPECIFIED.);
#450=B_SPLINE_CURVE_WITH_KNOTS('',3,(#44279,#44280,#44281,#44282,#44283,
#44284,#44285,#44286,#44287,#44288,#44289,#44290,#44291,#44292,#44293,#44294,
#44295,#44296,#44297,#44298,#44299,#44300,#44301,#44302,#44303,#44304,#44305),
 .UNSPECIFIED.,.F.,.F.,(4,2,2,2,3,2,2,2,2,2,2,2,4),(0.922537325049047,0.999310505714261,
1.07608368637947,1.15306672655577,1.23004976673206,1.30703280690836,1.38401584708465,
1.46078902774986,1.53756220841508,1.61433538908029,1.69110856974551,1.7680916099218,
1.84507465009809),.UNSPECIFIED.);
#451=B_SPLINE_CURVE_WITH_KNOTS('',3,(#44306,#44307,#44308,#44309,#44310,
#44311,#44312,#44313,#44314,#44315),.UNSPECIFIED.,.F.,.F.,(4,2,2,2,4),(1.84507465009809,
1.92205769027439,1.99904073045068,2.0758139111159,2.15258709178111),
 .UNSPECIFIED.);
#452=B_SPLINE_CURVE_WITH_KNOTS('',3,(#44318,#44319,#44320,#44321,#44322,
#44323,#44324,#44325,#44326,#44327,#44328,#44329,#44330,#44331,#44332,#44333,
#44334,#44335,#44336,#44337,#44338,#44339,#44340,#44341,#44342,#44343,#44344,
#44345,#44346,#44347,#44348,#44349,#44350,#44351),.UNSPECIFIED.,.T.,.F.,
(4,2,2,2,2,2,2,2,2,2,2,2,2,2,2,2,4),(-1.23004976673206,-1.15306672655577,
-1.07608368637947,-0.999310505714261,-0.922537325049047,-0.845764144383833,
-0.76899096371862,-0.692007923542325,-0.615024883366031,-0.538041843189737,
-0.461058803013443,-0.384285622348229,-0.307512441683016,-0.230739261017802,
-0.153966080352588,-0.0769830401762941,0.),.UNSPECIFIED.);
#453=B_SPLINE_CURVE_WITH_KNOTS('',3,(#44399,#44400,#44401,#44402,#44403,
#44404,#44405,#44406,#44407,#44408,#44409,#44410,#44411,#44412,#44413,#44414,
#44415,#44416,#44417,#44418,#44419,#44420,#44421,#44422,#44423,#44424,#44425,
#44426,#44427,#44428,#44429,#44430,#44431,#44432,#44433,#44434,#44435,#44436,
#44437,#44438,#44439,#44440,#44441),.UNSPECIFIED.,.F.,.F.,(4,3,3,3,3,3,
3,3,3,3,3,3,3,3,4),(0.,0.000265218733424361,0.000529943392799562,0.000791311297886273,
0.00104485851075797,0.00120949425781351,0.00140442813951922,0.00159510196316745,
0.00177939478496708,0.00181424138672026,0.00194996928456625,0.00208057934802266,
0.00220782711137267,0.00232952375057779,0.00241898851562701),
 .UNSPECIFIED.);
#454=B_SPLINE_CURVE_WITH_KNOTS('',3,(#44450,#44451,#44452,#44453,#44454,
#44455,#44456,#44457),.UNSPECIFIED.,.F.,.F.,(4,2,2,4),(1.10972417955536E-15,
0.000601563815809569,0.00120312763161803,0.00240625526323496),
 .UNSPECIFIED.);
#455=B_SPLINE_CURVE_WITH_KNOTS('',3,(#44486,#44487,#44488,#44489,#44490,
#44491,#44492,#44493,#44494,#44495,#44496,#44497,#44498,#44499,#44500,#44501,
#44502,#44503,#44504,#44505,#44506,#44507,#44508,#44509,#44510,#44511,#44512,
#44513,#44514,#44515,#44516,#44517,#44518,#44519,#44520,#44521,#44522,#44523,
#44524,#44525),.UNSPECIFIED.,.F.,.F.,(4,3,3,3,3,3,3,3,3,3,3,3,3,4),(0.,
0.000120731756906386,0.000244724286038655,0.000330382072298398,0.00038742395842631,
0.000451543376039767,0.000587355431077626,0.000736422494620045,0.000783140574770168,
0.0007839342580256,0.00111532596981935,0.00117471086215525,0.00117522277660967,
0.00156628114954034),.UNSPECIFIED.);
#456=B_SPLINE_CURVE_WITH_KNOTS('',3,(#44533,#44534,#44535,#44536,#44537,
#44538,#44539,#44540,#44541,#44542,#44543,#44544,#44545,#44546,#44547,#44548,
#44549,#44550,#44551,#44552,#44553,#44554,#44555,#44556,#44557,#44558,#44559,
#44560,#44561,#44562,#44563,#44564,#44565,#44566,#44567,#44568,#44569),
 .UNSPECIFIED.,.F.,.F.,(4,3,3,3,3,3,3,3,3,3,3,3,4),(0.,0.000121030957133445,
0.000244083459183201,0.000368145253824231,0.000391521746120079,0.000542549206905392,
0.000692240215942904,0.000782245350403997,0.000783043492240158,0.0011402076544283,
0.00117391722717013,0.00117456523836024,0.00156608698448032),
 .UNSPECIFIED.);
#457=B_SPLINE_CURVE_WITH_KNOTS('',3,(#44678,#44679,#44680,#44681,#44682,
#44683,#44684),.UNSPECIFIED.,.F.,.F.,(4,3,4),(8.8191888018214E-12,0.00104225234663735,
0.00196541786057149),.UNSPECIFIED.);
#458=B_SPLINE_CURVE_WITH_KNOTS('',3,(#44686,#44687,#44688,#44689,#44690,
#44691,#44692,#44693,#44694,#44695,#44696,#44697,#44698,#44699,#44700,#44701,
#44702,#44703,#44704,#44705,#44706,#44707,#44708,#44709,#44710,#44711,#44712,
#44713,#44714,#44715,#44716),.UNSPECIFIED.,.F.,.F.,(4,3,3,3,3,3,3,3,3,3,
4),(0.,0.000282229008902596,0.000596615472147253,0.000672888082078944,0.000674913983482446,
0.00113908191323505,0.0013477148488729,0.00134982796696489,0.00185411344461373,
0.00236801844152055,0.00269965593392979),.UNSPECIFIED.);
#459=B_SPLINE_CURVE_WITH_KNOTS('',3,(#44724,#44725,#44726,#44727,#44728,
#44729,#44730,#44731,#44732,#44733,#44734,#44735,#44736,#44737,#44738,#44739,
#44740,#44741,#44742,#44743,#44744,#44745,#44746,#44747,#44748,#44749,#44750,
#44751),.UNSPECIFIED.,.F.,.F.,(4,3,3,3,3,3,3,3,3,4),(0.,0.000683898970964164,
0.00134585328061937,0.00134792532155823,0.00179669833308319,0.00201877992092906,
0.0020208379703943,0.00232967550949865,0.00260160458154724,0.00269170656123875),
 .UNSPECIFIED.);
#460=B_SPLINE_CURVE_WITH_KNOTS('',3,(#44753,#44754,#44755,#44756,#44757,
#44758,#44759),.UNSPECIFIED.,.F.,.F.,(4,3,4),(1.55158384577955E-17,0.00104225233782226,
0.0019654178517479),.UNSPECIFIED.);
#461=B_SPLINE_CURVE_WITH_KNOTS('',3,(#44766,#44767,#44768,#44769,#44770,
#44771,#44772,#44773,#44774,#44775,#44776,#44777),.UNSPECIFIED.,.F.,.F.,
(4,2,2,2,2,4),(0.,0.023927482322817,0.0451601219442732,0.0651153892897719,
0.0785588651844482,0.0909362631271192),.UNSPECIFIED.);
#462=B_SPLINE_CURVE_WITH_KNOTS('',3,(#44785,#44786,#44787,#44788,#44789,
#44790),.UNSPECIFIED.,.F.,.F.,(4,2,4),(1.03628274237769E-6,0.0204474690808872,
0.0408541618075523),.UNSPECIFIED.);
#463=B_SPLINE_CURVE_WITH_KNOTS('',3,(#44831,#44832,#44833,#44834),
 .UNSPECIFIED.,.F.,.F.,(4,4),(0.,0.00159208620889079),.UNSPECIFIED.);
#464=B_SPLINE_CURVE_WITH_KNOTS('',3,(#44836,#44837,#44838,#44839,#44840,
#44841),.UNSPECIFIED.,.F.,.F.,(4,2,4),(-0.0108288738373355,-0.00541184520716738,
0.),.UNSPECIFIED.);
#465=B_SPLINE_CURVE_WITH_KNOTS('',3,(#44857,#44858,#44859,#44860,#44861,
#44862),.UNSPECIFIED.,.F.,.F.,(4,2,4),(-0.0108279843969241,-0.00541695432919009,
-7.41619925991033E-7),.UNSPECIFIED.);
#466=B_SPLINE_CURVE_WITH_KNOTS('',3,(#44868,#44869,#44870,#44871),
 .UNSPECIFIED.,.F.,.F.,(4,4),(1.72172026516128E-9,0.00159208793060872),
 .UNSPECIFIED.);
#467=B_SPLINE_CURVE_WITH_KNOTS('',3,(#44877,#44878,#44879,#44880,#44881,
#44882,#44883,#44884,#44885,#44886,#44887,#44888),.UNSPECIFIED.,.F.,.F.,
(4,2,2,2,2,4),(-0.0909372297788789,-0.0786310994776589,-0.0652694224322856,
-0.0453380124663928,-0.0241275039307517,0.),.UNSPECIFIED.);
#468=B_SPLINE_CURVE_WITH_KNOTS('',3,(#44922,#44923,#44924,#44925,#44926,
#44927),.UNSPECIFIED.,.F.,.F.,(4,2,4),(-0.0408541865438099,-0.0204437555046671,
-1.03628388816493E-6),.UNSPECIFIED.);
#469=B_SPLINE_CURVE_WITH_KNOTS('',3,(#44929,#44930,#44931,#44932,#44933,
#44934,#44935,#44936,#44937,#44938,#44939,#44940,#44941,#44942,#44943,#44944,
#44945,#44946,#44947,#44948,#44949,#44950,#44951,#44952,#44953,#44954,#44955,
#44956,#44957,#44958,#44959,#44960,#44961,#44962),.UNSPECIFIED.,.F.,.F.,
(4,3,3,3,3,3,3,3,3,3,3,4),(0.,0.000262944884148408,0.000263234297577755,
0.000494857606554129,0.000525889768296816,0.000526476175615979,0.00064121097647369,
0.000757086494550119,0.000788834652445224,0.000880494124966269,0.000970158609493951,
0.00105177953659363),.UNSPECIFIED.);
#470=B_SPLINE_CURVE_WITH_KNOTS('',3,(#44966,#44967,#44968,#44969,#44970,
#44971,#44972,#44973,#44974,#44975,#44976,#44977,#44978,#44979,#44980,#44981,
#44982,#44983,#44984,#44985,#44986,#44987,#44988,#44989,#44990,#44991,#44992,
#44993,#44994,#44995,#44996,#44997,#44998,#44999,#45000,#45001,#45002),
 .UNSPECIFIED.,.F.,.F.,(4,3,3,3,3,3,3,3,3,3,3,3,4),(0.,0.000244362774360397,
0.000262384380603159,0.000262964527186242,0.000497872683618592,0.0005253349756591,
0.000525929054372485,0.000639225228153213,0.000753740945662581,0.000788893581558727,
0.000881307299681151,0.000971994008335542,0.00105185810874497),
 .UNSPECIFIED.);
#471=B_SPLINE_CURVE_WITH_KNOTS('',3,(#45251,#45252,#45253,#45254,#45255,
#45256,#45257,#45258,#45259,#45260,#45261,#45262,#45263,#45264),
 .UNSPECIFIED.,.F.,.F.,(4,2,2,2,2,2,4),(-0.478011466323298,-0.477450068616196,
-0.4160793870133,-0.355479826428422,-0.296403852091954,-0.238674806903838,
-0.238656685114328),.UNSPECIFIED.);
#472=B_SPLINE_CURVE_WITH_KNOTS('',3,(#45268,#45269,#45270,#45271,#45272,
#45273,#45274,#45275),.UNSPECIFIED.,.F.,.F.,(4,2,2,4),(-1.28046581538947,
-1.24694324764166,-1.16660067584426,-1.12172029214894),.UNSPECIFIED.);
#473=B_SPLINE_CURVE_WITH_KNOTS('',3,(#45276,#45277,#45278,#45279,#45280,
#45281,#45282,#45283,#45284,#45285,#45286,#45287),.UNSPECIFIED.,.F.,.F.,
(4,2,2,2,2,4),(1.32320401424985,1.33548572406861,1.3557039818829,1.41353490960294,
1.47136583732297,1.75011843198071),.UNSPECIFIED.);
#474=B_SPLINE_CURVE_WITH_KNOTS('',3,(#45293,#45294,#45295,#45296,#45297,
#45298,#45299,#45300,#45301,#45302,#45303,#45304,#45305,#45306),
 .UNSPECIFIED.,.F.,.F.,(4,2,2,2,2,2,4),(-0.238656685112889,-0.181355245214609,
-0.12330633361927,-0.0637887774894114,-0.0319236327969544,-1.27398092075737E-14,
0.000561480190367634),.UNSPECIFIED.);
#475=B_SPLINE_CURVE_WITH_KNOTS('',3,(#45310,#45311,#45312,#45313,#45314,
#45315,#45316,#45317,#45318,#45319,#45320,#45321),.UNSPECIFIED.,.F.,.F.,
(4,2,2,2,2,4),(0.893026008311947,1.17177860296978,1.22960953068981,1.28744045840985,
1.30765871622413,1.3199404260429),.UNSPECIFIED.);
#476=B_SPLINE_CURVE_WITH_KNOTS('',3,(#45322,#45323,#45324,#45325,#45326,
#45327,#45328,#45329,#45330,#45331),.UNSPECIFIED.,.F.,.F.,(4,2,2,2,4),(-0.624724582317791,
-0.602042604282301,-0.537958860857827,-0.489657632758387,-0.482259949143694),
 .UNSPECIFIED.);
#477=B_SPLINE_CURVE_WITH_KNOTS('',3,(#45337,#45338,#45339,#45340,#45341,
#45342,#45343,#45344,#45345,#45346,#45347,#45348,#45349,#45350,#45351,#45352,
#45353,#45354,#45355,#45356,#45357,#45358),.UNSPECIFIED.,.F.,.F.,(4,2,2,
2,1,1,1,1,2,2,2,2,4),(0.,0.250000000000738,0.375000000001107,0.43750000000129,
0.468750000001377,0.484375000001422,0.492187500001443,0.496093750001453,
0.49804687500145,0.500000000001447,0.750000000000721,0.87500000000036,1.),
 .UNSPECIFIED.);
#478=B_SPLINE_CURVE_WITH_KNOTS('',3,(#45361,#45362,#45363,#45364,#45365,
#45366,#45367,#45368,#45369,#45370,#45371,#45372,#45373,#45374,#45375,#45376),
 .UNSPECIFIED.,.F.,.F.,(4,2,2,2,2,2,2,4),(-0.539155078775716,-0.498671728991868,
-0.431839786572352,-0.357600677552978,-0.261503696582492,-0.134722695832283,
0.,0.0010080897643522),.UNSPECIFIED.);
#479=B_SPLINE_CURVE_WITH_KNOTS('',3,(#45382,#45383,#45384,#45385,#45386,
#45387,#45388,#45389,#45390,#45391,#45392,#45393,#45394,#45395,#45396,#45397,
#45398,#45399,#45400,#45401,#45402,#45403),.UNSPECIFIED.,.F.,.F.,(4,2,2,
2,2,1,1,1,1,2,2,2,4),(0.000307299979407227,0.124999999999807,0.249999999999614,
0.374999999999422,0.437499999999325,0.46874999999927,0.484374999999239,
0.492187499999224,0.496093749999213,0.498046874999211,0.499999999999209,
0.749999999999605,1.),.UNSPECIFIED.);
#480=B_SPLINE_CURVE_WITH_KNOTS('',3,(#45406,#45407,#45408,#45409,#45410,
#45411,#45412,#45413,#45414,#45415,#45416,#45417,#45418,#45419,#45420,#45421),
 .UNSPECIFIED.,.F.,.F.,(4,2,2,2,2,2,2,4),(-1.54028535744593,-1.53927726768737,
-1.40455457263243,-1.27777357261349,-1.18167659219378,-1.10743748360041,
-1.04060554156496,-1.00012219201053),.UNSPECIFIED.);
#481=B_SPLINE_CURVE_WITH_KNOTS('',3,(#45655,#45656,#45657,#45658,#45659,
#45660,#45661,#45662,#45663,#45664,#45665,#45666,#45667,#45668,#45669,#45670,
#45671,#45672,#45673,#45674,#45675,#45676,#45677,#45678,#45679,#45680,#45681,
#45682,#45683,#45684,#45685,#45686,#45687,#45688,#45689,#45690,#45691,#45692,
#45693,#45694,#45695,#45696,#45697,#45698,#45699,#45700,#45701,#45702,#45703,
#45704,#45705,#45706,#45707,#45708,#45709,#45710,#45711,#45712,#45713,#45714,
#45715,#45716,#45717,#45718,#45719,#45720,#45721,#45722,#45723,#45724,#45725,
#45726,#45727),.UNSPECIFIED.,.F.,.F.,(4,3,3,3,3,3,3,3,3,3,3,3,3,3,3,3,3,
3,3,3,3,3,3,3,4),(-4.11257062550913E-5,0.000211162300231747,0.00046350988042877,
0.000715878564535794,0.000968550589332387,0.00114123113312901,0.00138545825899057,
0.00162944378491571,0.00173240955282102,0.0019623825795414,0.00219370350738769,
0.00232358797251303,0.00250954819935604,0.00269528994831476,0.00288121303245579,
0.00291476639220505,0.00314628582243956,0.00337751095812055,0.00350594481189706,
0.00370563324181197,0.00390550571072881,0.00409712323158908,0.00432708598005531,
0.00455518200144187,0.00468830165128109),.UNSPECIFIED.);
#482=B_SPLINE_CURVE_WITH_KNOTS('',3,(#45728,#45729,#45730,#45731,#45732,
#45733,#45734,#45735,#45736,#45737,#45738,#45739,#45740,#45741),
 .UNSPECIFIED.,.F.,.F.,(4,2,2,2,2,2,4),(-0.95463956460269,-0.953847234743663,
-0.831921008082044,-0.711276912435687,-0.593231640056803,-0.477522014556901,
-0.476788308545111),.UNSPECIFIED.);
#483=B_SPLINE_CURVE_WITH_KNOTS('',3,(#45743,#45744,#45745,#45746,#45747,
#45748,#45749,#45750),.UNSPECIFIED.,.F.,.F.,(4,2,2,4),(-1.1200552360125,
-1.06565795604777,-0.91947526211342,-0.773292568179073),.UNSPECIFIED.);
#484=B_SPLINE_CURVE_WITH_KNOTS('',3,(#45752,#45753,#45754,#45755,#45756,
#45757,#45758,#45759,#45760,#45761,#45762,#45763,#45764,#45765,#45766,#45767,
#45768,#45769,#45770,#45771,#45772,#45773,#45774,#45775,#45776,#45777,#45778,
#45779,#45780,#45781,#45782,#45783,#45784,#45785,#45786,#45787,#45788,#45789,
#45790,#45791,#45792,#45793,#45794,#45795,#45796,#45797,#45798,#45799,#45800,
#45801,#45802,#45803,#45804,#45805,#45806,#45807,#45808,#45809,#45810,#45811,
#45812,#45813,#45814,#45815,#45816,#45817,#45818,#45819,#45820,#45821,#45822,
#45823,#45824),.UNSPECIFIED.,.F.,.F.,(4,3,3,3,3,3,3,3,3,3,3,3,3,3,3,3,3,
3,3,3,3,3,3,3,4),(0.,0.000225667550044305,0.000453521175865013,0.00058601050704541,
0.000784129836157538,0.000982083285598081,0.00117202101409082,0.00140097570403084,
0.00163057513263886,0.00175803152113623,0.00194229610832416,0.00212641016209573,
0.00231079586156332,0.00234404202818164,0.00257328610067309,0.00280154068634866,
0.00293005253522705,0.00317214395432889,0.00341450191345266,0.00351606304227246,
0.00384363571960531,0.00410207354931787,0.00429883028119473,0.00449594514523909,
0.00468808405636328),.UNSPECIFIED.);
#485=B_SPLINE_CURVE_WITH_KNOTS('',3,(#45825,#45826,#45827,#45828,#45829,
#45830,#45831,#45832,#45833,#45834,#45835,#45836,#45837,#45838),
 .UNSPECIFIED.,.F.,.F.,(4,2,2,2,2,2,4),(-0.477116828714656,-0.476383034932386,
-0.360659365287303,-0.242599765287782,-0.121941026584239,-2.22044604925031E-15,
0.000792426037240202),.UNSPECIFIED.);
#486=B_SPLINE_CURVE_WITH_KNOTS('',3,(#45840,#45841,#45842,#45843,#45844,
#45845,#45846,#45847),.UNSPECIFIED.,.F.,.F.,(4,2,2,4),(-2.26503183854715,
-2.1188491446128,-1.97266645067846,-1.91826917071372),.UNSPECIFIED.);
#487=B_SPLINE_CURVE_WITH_KNOTS('',3,(#45855,#45856,#45857,#45858,#45859,
#45860,#45861,#45862,#45863,#45864),.UNSPECIFIED.,.F.,.F.,(4,2,2,2,4),(-1.32111970138292,
-1.30631571776553,-1.23358981994045,-1.16086392211537,-1.01541212646521),
 .UNSPECIFIED.);
#488=B_SPLINE_CURVE_WITH_KNOTS('',3,(#45876,#45877,#45878,#45879,#45880,
#45881,#45882,#45883,#45884,#45885),.UNSPECIFIED.,.F.,.F.,(4,2,2,2,4),(-2.36315569877945,
-2.21770390312929,-2.14497800530421,-2.07225210747913,-2.05744812386174),
 .UNSPECIFIED.);
#489=B_SPLINE_CURVE_WITH_KNOTS('',3,(#45956,#45957,#45958,#45959,#45960,
#45961),.UNSPECIFIED.,.F.,.F.,(4,2,4),(9.99994026930247E-7,0.0176151554172842,
0.0352487921890912),.UNSPECIFIED.);
#490=B_SPLINE_CURVE_WITH_KNOTS('',3,(#45963,#45964,#45965,#45966,#45967,
#45968,#45969,#45970,#45971,#45972,#45973,#45974,#45975,#45976,#45977,#45978,
#45979,#45980,#45981,#45982,#45983,#45984,#45985,#45986,#45987,#45988,#45989,
#45990,#45991,#45992,#45993,#45994,#45995,#45996,#45997,#45998,#45999,#46000,
#46001,#46002,#46003,#46004,#46005,#46006,#46007,#46008,#46009,#46010,#46011,
#46012,#46013,#46014),.UNSPECIFIED.,.F.,.F.,(4,3,3,3,3,3,3,3,3,3,3,3,3,
3,3,3,3,4),(0.000349648495401886,0.000435856450628066,0.000518346998497937,
0.000600826327770219,0.000683750987549706,0.000694480316306607,0.000804774657733104,
0.000922043397533562,0.00103931213733402,0.00116300366655803,0.00129638856133148,
0.00138414395836143,0.00145781361132506,0.0015307723859531,0.00155655986887515,
0.00162456036766277,0.00169016314809249,0.00172897577938886),
 .UNSPECIFIED.);
#491=B_SPLINE_CURVE_WITH_KNOTS('',3,(#46018,#46019,#46020,#46021,#46022,
#46023,#46024,#46025,#46026,#46027,#46028,#46029,#46030,#46031,#46032,#46033,
#46034,#46035,#46036,#46037,#46038,#46039,#46040,#46041,#46042,#46043,#46044,
#46045,#46046,#46047,#46048,#46049,#46050,#46051,#46052,#46053,#46054,#46055,
#46056,#46057,#46058,#46059,#46060,#46061,#46062,#46063,#46064,#46065,#46066,
#46067,#46068,#46069,#46070,#46071,#46072,#46073,#46074,#46075),
 .UNSPECIFIED.,.F.,.F.,(4,3,3,3,3,3,3,3,3,3,3,3,3,3,3,3,3,3,3,4),(0.,6.18208684431606E-5,
0.000125984546932246,0.00017272653853377,0.000254497619285616,0.000336923412298459,
0.00034545307706754,0.000446850586818363,0.000547260798830634,0.000644898132372486,
0.000690906154135026,0.000804288074237915,0.000913238839396781,0.00101713942033291,
0.00103635923120251,0.00112272247834549,0.00120469306612868,0.0012867711835707,
0.00136943274587814,0.00138181221977441),.UNSPECIFIED.);
#492=B_SPLINE_CURVE_WITH_KNOTS('',3,(#46076,#46077,#46078,#46079,#46080,
#46081),.UNSPECIFIED.,.F.,.F.,(4,2,4),(2.506792132088E-5,0.0175792343156468,
0.0353218856598025),.UNSPECIFIED.);
#493=B_SPLINE_CURVE_WITH_KNOTS('',3,(#46115,#46116,#46117,#46118,#46119,
#46120),.UNSPECIFIED.,.F.,.F.,(4,1,1,4),(0.376076502031257,0.738151675687099,
0.838151675687099,1.),.UNSPECIFIED.);
#494=B_SPLINE_CURVE_WITH_KNOTS('',3,(#46122,#46123,#46124,#46125,#46126,
#46127),.UNSPECIFIED.,.F.,.F.,(4,2,4),(-0.64239307361528,-0.386347437361555,
-6.40648423200219E-10),.UNSPECIFIED.);
#495=B_SPLINE_CURVE_WITH_KNOTS('',3,(#46131,#46132,#46133,#46134,#46135,
#46136),.UNSPECIFIED.,.F.,.F.,(4,1,1,4),(0.0598879851737023,0.738151675687099,
0.838151675687099,1.),.UNSPECIFIED.);
#496=B_SPLINE_CURVE_WITH_KNOTS('',3,(#46142,#46143,#46144,#46145,#46146,
#46147,#46148,#46149,#46150,#46151,#46152,#46153),.UNSPECIFIED.,.F.,.F.,
(4,2,2,2,2,4),(-0.843680482904519,-0.817052168712459,-0.771952825368238,
-0.653804262290151,-0.443525213357367,-1.91323158427181E-7),
 .UNSPECIFIED.);
#497=B_SPLINE_CURVE_WITH_KNOTS('',3,(#46161,#46162,#46163,#46164,#46165,
#46166),.UNSPECIFIED.,.F.,.F.,(4,1,1,4),(0.0598879851737348,0.738151675687099,
0.838151675687099,1.),.UNSPECIFIED.);
#498=B_SPLINE_CURVE_WITH_KNOTS('',3,(#46168,#46169,#46170,#46171,#46172,
#46173,#46174,#46175,#46176,#46177,#46178,#46179,#46180,#46181,#46182,#46183,
#46184,#46185,#46186,#46187,#46188,#46189,#46190,#46191,#46192,#46193,#46194,
#46195,#46196,#46197,#46198,#46199,#46200,#46201,#46202,#46203,#46204,#46205,
#46206,#46207,#46208,#46209,#46210,#46211,#46212,#46213,#46214,#46215,#46216,
#46217,#46218,#46219,#46220,#46221,#46222,#46223,#46224,#46225,#46226,#46227,
#46228,#46229,#46230,#46231,#46232,#46233,#46234,#46235,#46236,#46237,#46238,
#46239,#46240,#46241,#46242,#46243,#46244,#46245,#46246),.UNSPECIFIED.,
 .F.,.F.,(4,3,3,3,3,3,3,3,3,3,3,3,3,3,3,3,3,3,3,3,3,3,3,3,3,3,4),(0.,0.00133019741218274,
0.00338235256079639,0.00652827854954051,0.00749519144790343,0.00804058416816147,
0.0120370484455271,0.0157490242005424,0.0160811683363229,0.0208199774885995,
0.024033074620882,0.0241217525044844,0.0295749122668503,0.0321623366726459,
0.0323411021984972,0.0384974117946658,0.0449050664554913,0.0482435050089688,
0.0490120029708162,0.0550890503579654,0.0562840891771302,0.0573667064243252,
0.060304381261211,0.0615453779150555,0.0623145273032513,0.063632912088931,
0.0643246733452917),.UNSPECIFIED.);
#499=B_SPLINE_CURVE_WITH_KNOTS('',3,(#46252,#46253,#46254,#46255,#46256,
#46257,#46258,#46259,#46260,#46261,#46262,#46263,#46264,#46265,#46266,#46267,
#46268,#46269,#46270,#46271,#46272,#46273,#46274,#46275,#46276,#46277,#46278,
#46279,#46280,#46281,#46282,#46283,#46284,#46285,#46286,#46287,#46288,#46289,
#46290,#46291,#46292,#46293,#46294,#46295,#46296,#46297,#46298,#46299,#46300,
#46301,#46302,#46303,#46304,#46305,#46306,#46307,#46308,#46309,#46310,#46311,
#46312,#46313,#46314,#46315,#46316,#46317,#46318,#46319,#46320,#46321,#46322,
#46323,#46324,#46325,#46326,#46327,#46328,#46329,#46330),.UNSPECIFIED.,
 .F.,.F.,(4,3,3,3,3,3,3,3,3,3,3,3,3,3,3,3,3,3,3,3,3,3,3,3,3,3,4),(0.,0.000694963224053612,
0.00201945044095915,0.00279216000467784,0.0040389008819183,0.0069901733868374,
0.00807780176383661,0.0141829780064518,0.0153835484055692,0.0161556035276732,
0.0226284612866144,0.0288382348705923,0.0321316140743103,0.0323112070553464,
0.0377896082937388,0.040389008819183,0.0404780971676904,0.0452388410930198,
0.0484668105830197,0.0488004921202978,0.0528154549227909,0.0565446123468563,
0.0570925295361479,0.0602530171328019,0.0612244055941231,0.063286059589963,
0.0646224141106929),.UNSPECIFIED.);
#500=B_SPLINE_CURVE_WITH_KNOTS('',3,(#46339,#46340,#46341,#46342,#46343,
#46344,#46345,#46346,#46347,#46348,#46349,#46350,#46351,#46352,#46353,#46354,
#46355,#46356,#46357,#46358,#46359,#46360),.UNSPECIFIED.,.F.,.F.,(4,2,2,
2,2,2,2,2,2,2,4),(0.,0.00822683057377827,0.0164536611475565,0.0246804917213348,
0.0329073222951131,0.0493609834426696,0.0575878140164479,0.061701229303337,
0.0637579369467816,0.0647862907685039,0.0658146445902262),.UNSPECIFIED.);
#501=B_SPLINE_CURVE_WITH_KNOTS('',3,(#46361,#46362,#46363,#46364,#46365,
#46366,#46367,#46368,#46369,#46370,#46371,#46372,#46373,#46374,#46375,#46376,
#46377,#46378,#46379,#46380,#46381,#46382,#46383,#46384),.UNSPECIFIED.,
 .F.,.F.,(4,2,2,2,2,2,2,2,2,2,2,4),(-6.00000000093941E-8,0.00051597907764729,
0.00103201815529459,0.00206409631058923,0.00412825262117847,0.0082565652423569,
0.0165131904847138,0.0330264409694275,0.0412830662117844,0.0495396914541413,
0.0577963166964982,0.0660529419388551),.UNSPECIFIED.);
#502=B_SPLINE_CURVE_WITH_KNOTS('',3,(#46400,#46401,#46402,#46403,#46404,
#46405),.UNSPECIFIED.,.F.,.F.,(4,2,4),(-1.76748570019267,-0.704486820958434,
-1.00000183531384E-6),.UNSPECIFIED.);
#503=B_SPLINE_CURVE_WITH_KNOTS('',3,(#46407,#46408,#46409,#46410,#46411,
#46412),.UNSPECIFIED.,.F.,.F.,(4,1,1,4),(0.376076502030214,0.738151675687099,
0.838151675687099,1.),.UNSPECIFIED.);
#504=B_SPLINE_CURVE_WITH_KNOTS('',3,(#46417,#46418,#46419,#46420,#46421,
#46422,#46423,#46424,#46425,#46426,#46427,#46428),.UNSPECIFIED.,.F.,.F.,
(4,2,2,2,2,4),(-0.957807021571877,-0.464707050841796,-0.230924084318286,
-0.0995694788423429,-0.0494291617315582,-0.0198244706793161),
 .UNSPECIFIED.);
#505=B_SPLINE_CURVE_WITH_KNOTS('',3,(#46430,#46431,#46432,#46433,#46434,
#46435,#46436,#46437,#46438,#46439,#46440,#46441,#46442,#46443,#46444,#46445,
#46446,#46447,#46448,#46449,#46450,#46451,#46452,#46453,#46454,#46455,#46456,
#46457),.UNSPECIFIED.,.F.,.F.,(4,3,3,3,3,3,3,3,3,4),(2.77555756156289E-17,
0.00571779521669806,0.00742042674236585,0.00752642944116232,0.0140544642997195,
0.0148408534847317,0.0186294855440519,0.0236729311553377,0.0285768772393396,
0.0296817069694633),.UNSPECIFIED.);
#506=B_SPLINE_CURVE_WITH_KNOTS('',3,(#46458,#46459,#46460,#46461,#46462,
#46463,#46464,#46465,#46466,#46467,#46468,#46469,#46470),.UNSPECIFIED.,
 .F.,.F.,(4,3,3,3,4),(0.0315167029732621,0.0353810056968997,0.0390981239403465,
0.0415114270041217,0.0422033631272556),.UNSPECIFIED.);
#507=B_SPLINE_CURVE_WITH_KNOTS('',3,(#46472,#46473,#46474,#46475,#46476,
#46477,#46478,#46479,#46480,#46481,#46482,#46483,#46484),.UNSPECIFIED.,
 .F.,.F.,(4,3,3,3,4),(0.,0.000690309032879575,0.00438171613044424,0.00821369103151036,
0.0106615304346148),.UNSPECIFIED.);
#508=B_SPLINE_CURVE_WITH_KNOTS('',3,(#46485,#46486,#46487,#46488,#46489,
#46490,#46491,#46492,#46493,#46494,#46495,#46496,#46497,#46498,#46499,#46500,
#46501,#46502,#46503,#46504,#46505,#46506,#46507,#46508,#46509,#46510,#46511,
#46512),.UNSPECIFIED.,.F.,.F.,(4,3,3,3,3,3,3,3,3,4),(0.0124922114387784,
0.0173786759880834,0.0224014774550337,0.0235184435261858,0.0272981666037043,
0.0338108507614971,0.0345953907531371,0.0347011441861673,0.0404054939590322,
0.0421041217686302),.UNSPECIFIED.);
#509=B_SPLINE_CURVE_WITH_KNOTS('',3,(#46558,#46559,#46560,#46561,#46562,
#46563,#46564,#46565,#46566,#46567,#46568,#46569),.UNSPECIFIED.,.F.,.F.,
(4,2,1,1,2,2,4),(0.,0.00781250000000001,0.015625,0.03125,0.0624999999999999,
0.125,0.242820560992689),.UNSPECIFIED.);
#510=B_SPLINE_CURVE_WITH_KNOTS('',3,(#46571,#46572,#46573,#46574,#46575,
#46576,#46577,#46578,#46579,#46580,#46581,#46582,#46583,#46584,#46585,#46586,
#46587,#46588,#46589,#46590,#46591,#46592,#46593,#46594,#46595,#46596,#46597,
#46598,#46599,#46600,#46601,#46602,#46603,#46604,#46605,#46606,#46607,#46608,
#46609,#46610,#46611,#46612,#46613,#46614,#46615,#46616,#46617,#46618,#46619,
#46620,#46621,#46622,#46623,#46624,#46625,#46626,#46627,#46628),
 .UNSPECIFIED.,.F.,.F.,(4,3,3,3,3,3,3,3,3,3,3,3,3,3,3,3,3,3,3,4),(0.,0.000180857725498468,
0.000242475536420596,0.000462636248961816,0.000484380312649641,0.000484543019812994,
0.000726570468974455,0.000726736566375218,0.000847847927148936,0.000968760625299268,
0.000968976684750301,0.00109011139518026,0.00121095078162408,0.00121122083086588,
0.00145314093794889,0.00145337525175495,0.00167755435588957,0.00169564548526077,
0.00188459038844521,0.00193752125059852),.UNSPECIFIED.);
#511=B_SPLINE_CURVE_WITH_KNOTS('',3,(#46630,#46631,#46632,#46633,#46634,
#46635,#46636,#46637,#46638,#46639,#46640,#46641,#46642,#46643,#46644,#46645,
#46646,#46647),.UNSPECIFIED.,.F.,.F.,(4,2,2,2,2,2,2,2,4),(0.0216871878151901,
0.032680217438002,0.0436732470608138,0.0546662766836257,0.0601627914950316,
0.0629110489007346,0.0642851776035861,0.0649722419550118,0.0656593063064375),
 .UNSPECIFIED.);
#512=B_SPLINE_CURVE_WITH_KNOTS('',3,(#46651,#46652,#46653,#46654,#46655,
#46656,#46657,#46658,#46659,#46660,#46661,#46662,#46663,#46664,#46665,#46666,
#46667,#46668),.UNSPECIFIED.,.F.,.F.,(4,2,2,2,2,2,2,2,4),(0.,0.000689842611306874,
0.00137968522261375,0.00275937044522753,0.00551874089045509,0.0110374817809102,
0.0220749635618205,0.0331124453427309,0.0441499271236412),.UNSPECIFIED.);
#513=B_SPLINE_CURVE_WITH_KNOTS('',3,(#46670,#46671,#46672,#46673,#46674,
#46675,#46676,#46677,#46678,#46679,#46680,#46681,#46682,#46683,#46684,#46685,
#46686,#46687,#46688,#46689,#46690,#46691,#46692,#46693,#46694,#46695,#46696,
#46697,#46698,#46699,#46700,#46701,#46702,#46703,#46704,#46705,#46706,#46707,
#46708,#46709,#46710,#46711,#46712,#46713,#46714,#46715,#46716,#46717,#46718,
#46719,#46720,#46721,#46722,#46723,#46724),.UNSPECIFIED.,.F.,.F.,(4,3,3,
3,3,3,3,3,3,3,3,3,3,3,3,3,3,3,4),(9.33050753687133E-16,0.00018425279266257,
0.000235878931742768,0.000454457410544906,0.000472142579138733,0.000472396351922799,
0.000708293271574268,0.000708594527884195,0.000826400049535313,0.000944531464697737,
0.000944792703845591,0.00106266228766045,0.00118075303404218,0.00118099087980699,
0.0014168040003498,0.00141718905576838,0.00165316656365015,0.001850849561933,
0.00188958540769117),.UNSPECIFIED.);
#514=B_SPLINE_CURVE_WITH_KNOTS('',3,(#46828,#46829,#46830,#46831,#46832,
#46833,#46834,#46835,#46836,#46837,#46838,#46839,#46840,#46841,#46842,#46843,
#46844,#46845,#46846,#46847,#46848,#46849,#46850,#46851,#46852,#46853,#46854,
#46855,#46856,#46857,#46858,#46859,#46860,#46861,#46862,#46863,#46864,#46865,
#46866,#46867,#46868,#46869,#46870,#46871,#46872,#46873,#46874,#46875,#46876),
 .UNSPECIFIED.,.F.,.F.,(4,3,3,3,3,3,3,3,3,3,3,3,3,3,3,3,4),(0.,0.000109468558295443,
0.000219785271344123,0.000330646009385498,0.00044249674566146,0.000468452330512348,
0.000589929933612792,0.000715263674224842,0.000847107675387793,0.000936904661024695,
0.00105512166097558,0.0011758327883036,0.00129946242311971,0.00140535699153704,
0.00158825025111182,0.00178591157987006,0.00187380932204939),
 .UNSPECIFIED.);
#515=B_SPLINE_CURVE_WITH_KNOTS('',3,(#46979,#46980,#46981,#46982,#46983,
#46984,#46985,#46986,#46987,#46988,#46989,#46990,#46991,#46992,#46993,#46994,
#46995,#46996,#46997,#46998,#46999,#47000,#47001,#47002,#47003,#47004,#47005,
#47006,#47007,#47008,#47009,#47010,#47011,#47012,#47013,#47014,#47015,#47016,
#47017,#47018,#47019,#47020,#47021,#47022,#47023,#47024,#47025,#47026,#47027),
 .UNSPECIFIED.,.F.,.F.,(4,3,3,3,3,3,3,3,3,3,3,3,3,3,3,3,4),(-6.33283738354695E-6,
0.000175132894873384,0.000348429481852089,0.000462988112447956,0.00058681834786203,
0.000709001656163456,0.000827259972155947,0.00093230906227946,0.0010641247249674,
0.00119160914162567,0.00131279282513799,0.00140163001211096,0.00151896024956884,
0.0016299235561327,0.00174028554103239,0.00184999846319747,0.00187095096194247),
 .UNSPECIFIED.);
#516=B_SPLINE_CURVE_WITH_KNOTS('',3,(#47033,#47034,#47035,#47036,#47037,
#47038,#47039,#47040,#47041,#47042,#47043,#47044,#47045,#47046,#47047,#47048,
#47049,#47050,#47051,#47052),.UNSPECIFIED.,.F.,.F.,(4,2,2,2,2,2,2,2,2,4),
(1.63264169611634E-6,0.00112071490622925,0.00249410485118844,0.00667587597325017,
0.0315279582548989,0.0586878942058162,0.0843353212386066,0.111794096810849,
0.141395316871198,0.169000061137383),.UNSPECIFIED.);
#517=B_SPLINE_CURVE_WITH_KNOTS('',3,(#47053,#47054,#47055,#47056,#47057,
#47058,#47059,#47060,#47061,#47062,#47063,#47064,#47065,#47066,#47067,#47068,
#47069,#47070,#47071,#47072),.UNSPECIFIED.,.F.,.F.,(4,2,2,2,2,2,2,2,2,4),
(0.,0.0273497535277419,0.0569920982606061,0.0844751673709711,0.110215240941746,
0.137351156959471,0.162388202840594,0.166588867976713,0.167966825157961,
0.169089008366351),.UNSPECIFIED.);
#518=B_SPLINE_CURVE_WITH_KNOTS('',3,(#47531,#47532,#47533,#47534,#47535,
#47536,#47537,#47538,#47539,#47540,#47541,#47542,#47543,#47544),
 .UNSPECIFIED.,.F.,.F.,(4,2,2,2,2,2,4),(0.039886669715827,0.0401044661515991,
0.0495727843168759,0.0592161981418575,0.0692076983643014,0.0797697497054474,
0.0800012054326904),.UNSPECIFIED.);
#519=B_SPLINE_CURVE_WITH_KNOTS('',3,(#47547,#47548,#47549,#47550,#47551,
#47552,#47553,#47554,#47555,#47556,#47557,#47558),.UNSPECIFIED.,.F.,.F.,
(4,2,2,2,2,4),(-0.000230133150951674,0.,0.0101766413292995,0.0200160913840905,
0.0297402908990685,0.0394076883089345),.UNSPECIFIED.);
#520=B_SPLINE_CURVE_WITH_KNOTS('',3,(#47560,#47561,#47562,#47563,#47564,
#47565,#47566,#47567,#47568,#47569,#47570,#47571),.UNSPECIFIED.,.F.,.F.,
(4,2,2,2,2,4),(-0.0398866697156879,-0.0305471274410706,-0.0206752787312571,
-0.010434866365749,0.,0.000231445227518166),.UNSPECIFIED.);
#521=B_SPLINE_CURVE_WITH_KNOTS('',3,(#47573,#47574,#47575,#47576,#47577,
#47578,#47579,#47580,#47581,#47582,#47583,#47584,#47585,#47586,#47587,#47588,
#47589,#47590,#47591,#47592,#47593,#47594,#47595,#47596,#47597,#47598,#47599,
#47600),.UNSPECIFIED.,.F.,.F.,(4,3,3,3,3,3,3,3,3,4),(-1.09105494845026E-5,
3.84251023745443E-5,8.55160249623879E-5,0.000132661739759183,0.000179909175493616,
0.000186432057951685,0.00023702907904941,0.000287481797438324,0.000337436285325506,
0.000383774665387872),.UNSPECIFIED.);
#522=B_SPLINE_CURVE_WITH_KNOTS('',3,(#47606,#47607,#47608,#47609,#47610,
#47611,#47612,#47613,#47614,#47615,#47616,#47617),.UNSPECIFIED.,.F.,.F.,
(4,2,2,2,2,4),(-0.0790455097686946,-0.0788153766177156,-0.0686387352884633,
-0.0587992852337163,-0.0490750857187486,-0.0394076883088853),
 .UNSPECIFIED.);
#523=B_SPLINE_CURVE_WITH_KNOTS('',3,(#47618,#47619,#47620,#47621,#47622,
#47623,#47624,#47625,#47626,#47627,#47628,#47629,#47630,#47631,#47632,#47633,
#47634,#47635,#47636,#47637,#47638,#47639,#47640,#47641,#47642,#47643,#47644,
#47645),.UNSPECIFIED.,.F.,.F.,(4,3,3,3,3,3,3,3,3,4),(0.,4.94468472281981E-5,
9.92247531380756E-5,0.00014929675610942,0.000195377841020618,0.000238646755348352,
0.000281883277306065,0.00032509948720421,0.000368395674290727,0.000390755682041237),
 .UNSPECIFIED.);
#524=B_SPLINE_CURVE_WITH_KNOTS('',3,(#47652,#47653,#47654,#47655,#47656,
#47657,#47658,#47659,#47660,#47661,#47662,#47663),.UNSPECIFIED.,.F.,.F.,
(4,2,2,2,2,4),(-0.000231445227522379,0.,0.0104348663658747,0.0206752787314242,
0.0305471274412819,0.0398866697158144),.UNSPECIFIED.);
#525=B_SPLINE_CURVE_WITH_KNOTS('',3,(#47665,#47666,#47667,#47668,#47669,
#47670,#47671,#47672,#47673,#47674,#47675,#47676),.UNSPECIFIED.,.F.,.F.,
(4,2,2,2,2,4),(-0.0799975657698679,-0.0797661310415978,-0.0693317380416801,
-0.0590917902207848,-0.0492203893360867,-0.0398812707391191),
 .UNSPECIFIED.);
#526=(
BOUNDED_SURFACE()
B_SPLINE_SURFACE(3,3,((#12266,#12267,#12268,#12269,#12270,#12271,#12272,
#12273,#12274,#12275,#12276,#12277,#12278,#12279,#12280,#12281,#12282,#12283,
#12284,#12285,#12286,#12287,#12288,#12289),(#12290,#12291,#12292,#12293,
#12294,#12295,#12296,#12297,#12298,#12299,#12300,#12301,#12302,#12303,#12304,
#12305,#12306,#12307,#12308,#12309,#12310,#12311,#12312,#12313),(#12314,
#12315,#12316,#12317,#12318,#12319,#12320,#12321,#12322,#12323,#12324,#12325,
#12326,#12327,#12328,#12329,#12330,#12331,#12332,#12333,#12334,#12335,#12336,
#12337),(#12338,#12339,#12340,#12341,#12342,#12343,#12344,#12345,#12346,
#12347,#12348,#12349,#12350,#12351,#12352,#12353,#12354,#12355,#12356,#12357,
#12358,#12359,#12360,#12361),(#12362,#12363,#12364,#12365,#12366,#12367,
#12368,#12369,#12370,#12371,#12372,#12373,#12374,#12375,#12376,#12377,#12378,
#12379,#12380,#12381,#12382,#12383,#12384,#12385),(#12386,#12387,#12388,
#12389,#12390,#12391,#12392,#12393,#12394,#12395,#12396,#12397,#12398,#12399,
#12400,#12401,#12402,#12403,#12404,#12405,#12406,#12407,#12408,#12409),
(#12410,#12411,#12412,#12413,#12414,#12415,#12416,#12417,#12418,#12419,
#12420,#12421,#12422,#12423,#12424,#12425,#12426,#12427,#12428,#12429,#12430,
#12431,#12432,#12433)),.UNSPECIFIED.,.T.,.F.,.F.)
B_SPLINE_SURFACE_WITH_KNOTS((4,3,4),(4,2,2,2,2,2,2,2,2,2,2,4),(0.,0.5,1.),
(0.916063809045508,0.917441355582055,0.918818902118601,0.921573995191693,
0.924329088264786,0.925706634801332,0.927084181337879,0.932594367484064,
0.935349460557156,0.936727007093702,0.937415780361976,0.938104553630249),
 .UNSPECIFIED.)
GEOMETRIC_REPRESENTATION_ITEM()
RATIONAL_B_SPLINE_SURFACE(((1.,1.,1.,1.,1.,1.,1.,1.,1.,1.,1.,1.,1.,1.,1.,
1.,1.,1.,1.,1.,1.,1.,1.,1.),(0.333333333333333,0.333333333333333,0.333333333333333,
0.333333333333333,0.333333333333333,0.333333333333333,0.333333333333333,
0.333333333333333,0.333333333333333,0.333333333333333,0.333333333333333,
0.333333333333333,0.333333333333333,0.333333333333333,0.333333333333333,
0.333333333333333,0.333333333333333,0.333333333333333,0.333333333333333,
0.333333333333333,0.333333333333333,0.333333333333333,0.333333333333333,
0.333333333333333),(0.333333333333333,0.333333333333333,0.333333333333333,
0.333333333333333,0.333333333333333,0.333333333333333,0.333333333333333,
0.333333333333333,0.333333333333333,0.333333333333333,0.333333333333333,
0.333333333333333,0.333333333333333,0.333333333333333,0.333333333333333,
0.333333333333333,0.333333333333333,0.333333333333333,0.333333333333333,
0.333333333333333,0.333333333333333,0.333333333333333,0.333333333333333,
0.333333333333333),(1.,1.,1.,1.,1.,1.,1.,1.,1.,1.,1.,1.,1.,1.,1.,1.,1.,
1.,1.,1.,1.,1.,1.,1.),(0.333333333333333,0.333333333333333,0.333333333333333,
0.333333333333333,0.333333333333333,0.333333333333333,0.333333333333333,
0.333333333333333,0.333333333333333,0.333333333333333,0.333333333333333,
0.333333333333333,0.333333333333333,0.333333333333333,0.333333333333333,
0.333333333333333,0.333333333333333,0.333333333333333,0.333333333333333,
0.333333333333333,0.333333333333333,0.333333333333333,0.333333333333333,
0.333333333333333),(0.333333333333333,0.333333333333333,0.333333333333333,
0.333333333333333,0.333333333333333,0.333333333333333,0.333333333333333,
0.333333333333333,0.333333333333333,0.333333333333333,0.333333333333333,
0.333333333333333,0.333333333333333,0.333333333333333,0.333333333333333,
0.333333333333333,0.333333333333333,0.333333333333333,0.333333333333333,
0.333333333333333,0.333333333333333,0.333333333333333,0.333333333333333,
0.333333333333333),(1.,1.,1.,1.,1.,1.,1.,1.,1.,1.,1.,1.,1.,1.,1.,1.,1.,
1.,1.,1.,1.,1.,1.,1.)))
REPRESENTATION_ITEM('')
SURFACE()
);
#527=(
BOUNDED_SURFACE()
B_SPLINE_SURFACE(3,3,((#12485,#12486,#12487,#12488,#12489,#12490,#12491,
#12492,#12493,#12494,#12495,#12496,#12497,#12498,#12499,#12500,#12501,#12502,
#12503,#12504,#12505,#12506,#12507,#12508,#12509,#12510,#12511,#12512,#12513,
#12514,#12515,#12516,#12517,#12518,#12519,#12520,#12521,#12522,#12523,#12524,
#12525,#12526,#12527,#12528,#12529,#12530,#12531,#12532,#12533,#12534,#12535,
#12536,#12537,#12538,#12539,#12540,#12541,#12542,#12543,#12544,#12545,#12546,
#12547,#12548,#12549,#12550,#12551,#12552,#12553,#12554,#12555,#12556,#12557,
#12558,#12559,#12560,#12561,#12562,#12563,#12564,#12565,#12566,#12567,#12568,
#12569,#12570,#12571,#12572,#12573,#12574,#12575,#12576,#12577,#12578,#12579,
#12580,#12581,#12582,#12583,#12584,#12585,#12586,#12587,#12588,#12589,#12590,
#12591,#12592,#12593,#12594,#12595,#12596,#12597,#12598,#12599,#12600,#12601,
#12602,#12603,#12604,#12605,#12606,#12607,#12608,#12609,#12610,#12611,#12612,
#12613,#12614,#12615,#12616,#12617,#12618,#12619,#12620,#12621,#12622,#12623,
#12624,#12625,#12626,#12627,#12628,#12629,#12630,#12631,#12632,#12633,#12634,
#12635,#12636,#12637,#12638,#12639,#12640,#12641,#12642,#12643,#12644,#12645,
#12646,#12647,#12648,#12649,#12650,#12651,#12652),(#12653,#12654,#12655,
#12656,#12657,#12658,#12659,#12660,#12661,#12662,#12663,#12664,#12665,#12666,
#12667,#12668,#12669,#12670,#12671,#12672,#12673,#12674,#12675,#12676,#12677,
#12678,#12679,#12680,#12681,#12682,#12683,#12684,#12685,#12686,#12687,#12688,
#12689,#12690,#12691,#12692,#12693,#12694,#12695,#12696,#12697,#12698,#12699,
#12700,#12701,#12702,#12703,#12704,#12705,#12706,#12707,#12708,#12709,#12710,
#12711,#12712,#12713,#12714,#12715,#12716,#12717,#12718,#12719,#12720,#12721,
#12722,#12723,#12724,#12725,#12726,#12727,#12728,#12729,#12730,#12731,#12732,
#12733,#12734,#12735,#12736,#12737,#12738,#12739,#12740,#12741,#12742,#12743,
#12744,#12745,#12746,#12747,#12748,#12749,#12750,#12751,#12752,#12753,#12754,
#12755,#12756,#12757,#12758,#12759,#12760,#12761,#12762,#12763,#12764,#12765,
#12766,#12767,#12768,#12769,#12770,#12771,#12772,#12773,#12774,#12775,#12776,
#12777,#12778,#12779,#12780,#12781,#12782,#12783,#12784,#12785,#12786,#12787,
#12788,#12789,#12790,#12791,#12792,#12793,#12794,#12795,#12796,#12797,#12798,
#12799,#12800,#12801,#12802,#12803,#12804,#12805,#12806,#12807,#12808,#12809,
#12810,#12811,#12812,#12813,#12814,#12815,#12816,#12817,#12818,#12819,#12820),
(#12821,#12822,#12823,#12824,#12825,#12826,#12827,#12828,#12829,#12830,
#12831,#12832,#12833,#12834,#12835,#12836,#12837,#12838,#12839,#12840,#12841,
#12842,#12843,#12844,#12845,#12846,#12847,#12848,#12849,#12850,#12851,#12852,
#12853,#12854,#12855,#12856,#12857,#12858,#12859,#12860,#12861,#12862,#12863,
#12864,#12865,#12866,#12867,#12868,#12869,#12870,#12871,#12872,#12873,#12874,
#12875,#12876,#12877,#12878,#12879,#12880,#12881,#12882,#12883,#12884,#12885,
#12886,#12887,#12888,#12889,#12890,#12891,#12892,#12893,#12894,#12895,#12896,
#12897,#12898,#12899,#12900,#12901,#12902,#12903,#12904,#12905,#12906,#12907,
#12908,#12909,#12910,#12911,#12912,#12913,#12914,#12915,#12916,#12917,#12918,
#12919,#12920,#12921,#12922,#12923,#12924,#12925,#12926,#12927,#12928,#12929,
#12930,#12931,#12932,#12933,#12934,#12935,#12936,#12937,#12938,#12939,#12940,
#12941,#12942,#12943,#12944,#12945,#12946,#12947,#12948,#12949,#12950,#12951,
#12952,#12953,#12954,#12955,#12956,#12957,#12958,#12959,#12960,#12961,#12962,
#12963,#12964,#12965,#12966,#12967,#12968,#12969,#12970,#12971,#12972,#12973,
#12974,#12975,#12976,#12977,#12978,#12979,#12980,#12981,#12982,#12983,#12984,
#12985,#12986,#12987,#12988),(#12989,#12990,#12991,#12992,#12993,#12994,
#12995,#12996,#12997,#12998,#12999,#13000,#13001,#13002,#13003,#13004,#13005,
#13006,#13007,#13008,#13009,#13010,#13011,#13012,#13013,#13014,#13015,#13016,
#13017,#13018,#13019,#13020,#13021,#13022,#13023,#13024,#13025,#13026,#13027,
#13028,#13029,#13030,#13031,#13032,#13033,#13034,#13035,#13036,#13037,#13038,
#13039,#13040,#13041,#13042,#13043,#13044,#13045,#13046,#13047,#13048,#13049,
#13050,#13051,#13052,#13053,#13054,#13055,#13056,#13057,#13058,#13059,#13060,
#13061,#13062,#13063,#13064,#13065,#13066,#13067,#13068,#13069,#13070,#13071,
#13072,#13073,#13074,#13075,#13076,#13077,#13078,#13079,#13080,#13081,#13082,
#13083,#13084,#13085,#13086,#13087,#13088,#13089,#13090,#13091,#13092,#13093,
#13094,#13095,#13096,#13097,#13098,#13099,#13100,#13101,#13102,#13103,#13104,
#13105,#13106,#13107,#13108,#13109,#13110,#13111,#13112,#13113,#13114,#13115,
#13116,#13117,#13118,#13119,#13120,#13121,#13122,#13123,#13124,#13125,#13126,
#13127,#13128,#13129,#13130,#13131,#13132,#13133,#13134,#13135,#13136,#13137,
#13138,#13139,#13140,#13141,#13142,#13143,#13144,#13145,#13146,#13147,#13148,
#13149,#13150,#13151,#13152,#13153,#13154,#13155,#13156),(#13157,#13158,
#13159,#13160,#13161,#13162,#13163,#13164,#13165,#13166,#13167,#13168,#13169,
#13170,#13171,#13172,#13173,#13174,#13175,#13176,#13177,#13178,#13179,#13180,
#13181,#13182,#13183,#13184,#13185,#13186,#13187,#13188,#13189,#13190,#13191,
#13192,#13193,#13194,#13195,#13196,#13197,#13198,#13199,#13200,#13201,#13202,
#13203,#13204,#13205,#13206,#13207,#13208,#13209,#13210,#13211,#13212,#13213,
#13214,#13215,#13216,#13217,#13218,#13219,#13220,#13221,#13222,#13223,#13224,
#13225,#13226,#13227,#13228,#13229,#13230,#13231,#13232,#13233,#13234,#13235,
#13236,#13237,#13238,#13239,#13240,#13241,#13242,#13243,#13244,#13245,#13246,
#13247,#13248,#13249,#13250,#13251,#13252,#13253,#13254,#13255,#13256,#13257,
#13258,#13259,#13260,#13261,#13262,#13263,#13264,#13265,#13266,#13267,#13268,
#13269,#13270,#13271,#13272,#13273,#13274,#13275,#13276,#13277,#13278,#13279,
#13280,#13281,#13282,#13283,#13284,#13285,#13286,#13287,#13288,#13289,#13290,
#13291,#13292,#13293,#13294,#13295,#13296,#13297,#13298,#13299,#13300,#13301,
#13302,#13303,#13304,#13305,#13306,#13307,#13308,#13309,#13310,#13311,#13312,
#13313,#13314,#13315,#13316,#13317,#13318,#13319,#13320,#13321,#13322,#13323,
#13324),(#13325,#13326,#13327,#13328,#13329,#13330,#13331,#13332,#13333,
#13334,#13335,#13336,#13337,#13338,#13339,#13340,#13341,#13342,#13343,#13344,
#13345,#13346,#13347,#13348,#13349,#13350,#13351,#13352,#13353,#13354,#13355,
#13356,#13357,#13358,#13359,#13360,#13361,#13362,#13363,#13364,#13365,#13366,
#13367,#13368,#13369,#13370,#13371,#13372,#13373,#13374,#13375,#13376,#13377,
#13378,#13379,#13380,#13381,#13382,#13383,#13384,#13385,#13386,#13387,#13388,
#13389,#13390,#13391,#13392,#13393,#13394,#13395,#13396,#13397,#13398,#13399,
#13400,#13401,#13402,#13403,#13404,#13405,#13406,#13407,#13408,#13409,#13410,
#13411,#13412,#13413,#13414,#13415,#13416,#13417,#13418,#13419,#13420,#13421,
#13422,#13423,#13424,#13425,#13426,#13427,#13428,#13429,#13430,#13431,#13432,
#13433,#13434,#13435,#13436,#13437,#13438,#13439,#13440,#13441,#13442,#13443,
#13444,#13445,#13446,#13447,#13448,#13449,#13450,#13451,#13452,#13453,#13454,
#13455,#13456,#13457,#13458,#13459,#13460,#13461,#13462,#13463,#13464,#13465,
#13466,#13467,#13468,#13469,#13470,#13471,#13472,#13473,#13474,#13475,#13476,
#13477,#13478,#13479,#13480,#13481,#13482,#13483,#13484,#13485,#13486,#13487,
#13488,#13489,#13490,#13491,#13492),(#13493,#13494,#13495,#13496,#13497,
#13498,#13499,#13500,#13501,#13502,#13503,#13504,#13505,#13506,#13507,#13508,
#13509,#13510,#13511,#13512,#13513,#13514,#13515,#13516,#13517,#13518,#13519,
#13520,#13521,#13522,#13523,#13524,#13525,#13526,#13527,#13528,#13529,#13530,
#13531,#13532,#13533,#13534,#13535,#13536,#13537,#13538,#13539,#13540,#13541,
#13542,#13543,#13544,#13545,#13546,#13547,#13548,#13549,#13550,#13551,#13552,
#13553,#13554,#13555,#13556,#13557,#13558,#13559,#13560,#13561,#13562,#13563,
#13564,#13565,#13566,#13567,#13568,#13569,#13570,#13571,#13572,#13573,#13574,
#13575,#13576,#13577,#13578,#13579,#13580,#13581,#13582,#13583,#13584,#13585,
#13586,#13587,#13588,#13589,#13590,#13591,#13592,#13593,#13594,#13595,#13596,
#13597,#13598,#13599,#13600,#13601,#13602,#13603,#13604,#13605,#13606,#13607,
#13608,#13609,#13610,#13611,#13612,#13613,#13614,#13615,#13616,#13617,#13618,
#13619,#13620,#13621,#13622,#13623,#13624,#13625,#13626,#13627,#13628,#13629,
#13630,#13631,#13632,#13633,#13634,#13635,#13636,#13637,#13638,#13639,#13640,
#13641,#13642,#13643,#13644,#13645,#13646,#13647,#13648,#13649,#13650,#13651,
#13652,#13653,#13654,#13655,#13656,#13657,#13658,#13659,#13660)),
 .UNSPECIFIED.,.T.,.F.,.F.)
B_SPLINE_SURFACE_WITH_KNOTS((4,3,4),(4,2,2,2,2,2,2,2,2,2,2,2,2,2,2,2,2,
2,2,2,2,2,2,2,2,2,2,2,2,2,2,2,2,2,2,2,2,2,2,2,2,2,2,2,2,2,2,2,2,2,2,2,2,
2,2,2,2,2,2,2,2,2,2,2,2,2,2,2,2,2,2,2,2,2,2,2,2,2,2,2,2,2,2,4),(0.,0.5,
1.),(0.0896131586159842,0.0909349273058256,0.092256695995667,0.09490023337535,
0.100187308134716,0.110761457653447,0.121335607172179,0.131909756690911,
0.142406945548381,0.152904134405852,0.163401323263323,0.173898512120793,
0.184326267064866,0.194754022008939,0.205181776953011,0.215609531897084,
0.225968774255778,0.236328016614473,0.246687258973167,0.257046501331861,
0.268365392558388,0.279684283784914,0.29100317501144,0.302322066237966,
0.313563979866736,0.324805893495506,0.336047807124276,0.347289720753047,
0.358457560536344,0.369625400319641,0.380793240102939,0.391961079886236,
0.403057648451734,0.414154217017233,0.425250785582731,0.43634735414823,
0.447375242283774,0.458403130419317,0.469431018554861,0.480458906690405,
0.491420626849432,0.50238234700846,0.513344067167488,0.524305787326516,
0.535203741266554,0.546101695206592,0.55699964914663,0.567897603086667,
0.578734005374906,0.589570407663145,0.600406809951383,0.611243212239622,
0.62202044333232,0.632797674425018,0.643574905517716,0.654352136610414,
0.665072195325672,0.675792254040929,0.686512312756186,0.697232371471444,
0.707897173370898,0.718561975270352,0.729226777169807,0.739891579069261,
0.750503305564763,0.761115032060264,0.771726758555766,0.782338485051267,
0.79289871583597,0.803458946620673,0.814019177405375,0.824579408190078,
0.835090233536042,0.845601058882007,0.856111884227971,0.866622709573936,
0.877085607262584,0.887548504951232,0.89801140263988,0.908474300328528,
0.912269054687018,0.914166431866263,0.915115120455886,0.916063809045508),
 .UNSPECIFIED.)
GEOMETRIC_REPRESENTATION_ITEM()
RATIONAL_B_SPLINE_SURFACE(((1.,1.,1.,1.,1.,1.,1.,1.,1.,1.,1.,1.,1.,1.,1.,
1.,1.,1.,1.,1.,1.,1.,1.,1.,1.,1.,1.,1.,1.,1.,1.,1.,1.,1.,1.,1.,1.,1.,1.,
1.,1.,1.,1.,1.,1.,1.,1.,1.,1.,1.,1.,1.,1.,1.,1.,1.,1.,1.,1.,1.,1.,1.,1.,
1.,1.,1.,1.,1.,1.,1.,1.,1.,1.,1.,1.,1.,1.,1.,1.,1.,1.,1.,1.,1.,1.,1.,1.,
1.,1.,1.,1.,1.,1.,1.,1.,1.,1.,1.,1.,1.,1.,1.,1.,1.,1.,1.,1.,1.,1.,1.,1.,
1.,1.,1.,1.,1.,1.,1.,1.,1.,1.,1.,1.,1.,1.,1.,1.,1.,1.,1.,1.,1.,1.,1.,1.,
1.,1.,1.,1.,1.,1.,1.,1.,1.,1.,1.,1.,1.,1.,1.,1.,1.,1.,1.,1.,1.,1.,1.,1.,
1.,1.,1.,1.,1.,1.,1.,1.,1.),(0.333333333333333,0.333333333333333,0.333333333333333,
0.333333333333333,0.333333333333333,0.333333333333333,0.333333333333333,
0.333333333333333,0.333333333333333,0.333333333333333,0.333333333333333,
0.333333333333333,0.333333333333333,0.333333333333333,0.333333333333333,
0.333333333333333,0.333333333333333,0.333333333333333,0.333333333333333,
0.333333333333333,0.333333333333333,0.333333333333333,0.333333333333333,
0.333333333333333,0.333333333333333,0.333333333333333,0.333333333333333,
0.333333333333333,0.333333333333333,0.333333333333333,0.333333333333333,
0.333333333333333,0.333333333333333,0.333333333333333,0.333333333333333,
0.333333333333333,0.333333333333333,0.333333333333333,0.333333333333333,
0.333333333333333,0.333333333333333,0.333333333333333,0.333333333333333,
0.333333333333333,0.333333333333333,0.333333333333333,0.333333333333333,
0.333333333333333,0.333333333333333,0.333333333333333,0.333333333333333,
0.333333333333333,0.333333333333333,0.333333333333333,0.333333333333333,
0.333333333333333,0.333333333333333,0.333333333333333,0.333333333333333,
0.333333333333333,0.333333333333333,0.333333333333333,0.333333333333333,
0.333333333333333,0.333333333333333,0.333333333333333,0.333333333333333,
0.333333333333333,0.333333333333333,0.333333333333333,0.333333333333333,
0.333333333333333,0.333333333333333,0.333333333333333,0.333333333333333,
0.333333333333333,0.333333333333333,0.333333333333333,0.333333333333333,
0.333333333333333,0.333333333333333,0.333333333333333,0.333333333333333,
0.333333333333333,0.333333333333333,0.333333333333333,0.333333333333333,
0.333333333333333,0.333333333333333,0.333333333333333,0.333333333333333,
0.333333333333333,0.333333333333333,0.333333333333333,0.333333333333333,
0.333333333333333,0.333333333333333,0.333333333333333,0.333333333333333,
0.333333333333333,0.333333333333333,0.333333333333333,0.333333333333333,
0.333333333333333,0.333333333333333,0.333333333333333,0.333333333333333,
0.333333333333333,0.333333333333333,0.333333333333333,0.333333333333333,
0.333333333333333,0.333333333333333,0.333333333333333,0.333333333333333,
0.333333333333333,0.333333333333333,0.333333333333333,0.333333333333333,
0.333333333333333,0.333333333333333,0.333333333333333,0.333333333333333,
0.333333333333333,0.333333333333333,0.333333333333333,0.333333333333333,
0.333333333333333,0.333333333333333,0.333333333333333,0.333333333333333,
0.333333333333333,0.333333333333333,0.333333333333333,0.333333333333333,
0.333333333333333,0.333333333333333,0.333333333333333,0.333333333333333,
0.333333333333333,0.333333333333333,0.333333333333333,0.333333333333333,
0.333333333333333,0.333333333333333,0.333333333333333,0.333333333333333,
0.333333333333333,0.333333333333333,0.333333333333333,0.333333333333333,
0.333333333333333,0.333333333333333,0.333333333333333,0.333333333333333,
0.333333333333333,0.333333333333333,0.333333333333333,0.333333333333333,
0.333333333333333,0.333333333333333,0.333333333333333,0.333333333333333,
0.333333333333333,0.333333333333333,0.333333333333333,0.333333333333333,
0.333333333333333),(0.333333333333333,0.333333333333333,0.333333333333333,
0.333333333333333,0.333333333333333,0.333333333333333,0.333333333333333,
0.333333333333333,0.333333333333333,0.333333333333333,0.333333333333333,
0.333333333333333,0.333333333333333,0.333333333333333,0.333333333333333,
0.333333333333333,0.333333333333333,0.333333333333333,0.333333333333333,
0.333333333333333,0.333333333333333,0.333333333333333,0.333333333333333,
0.333333333333333,0.333333333333333,0.333333333333333,0.333333333333333,
0.333333333333333,0.333333333333333,0.333333333333333,0.333333333333333,
0.333333333333333,0.333333333333333,0.333333333333333,0.333333333333333,
0.333333333333333,0.333333333333333,0.333333333333333,0.333333333333333,
0.333333333333333,0.333333333333333,0.333333333333333,0.333333333333333,
0.333333333333333,0.333333333333333,0.333333333333333,0.333333333333333,
0.333333333333333,0.333333333333333,0.333333333333333,0.333333333333333,
0.333333333333333,0.333333333333333,0.333333333333333,0.333333333333333,
0.333333333333333,0.333333333333333,0.333333333333333,0.333333333333333,
0.333333333333333,0.333333333333333,0.333333333333333,0.333333333333333,
0.333333333333333,0.333333333333333,0.333333333333333,0.333333333333333,
0.333333333333333,0.333333333333333,0.333333333333333,0.333333333333333,
0.333333333333333,0.333333333333333,0.333333333333333,0.333333333333333,
0.333333333333333,0.333333333333333,0.333333333333333,0.333333333333333,
0.333333333333333,0.333333333333333,0.333333333333333,0.333333333333333,
0.333333333333333,0.333333333333333,0.333333333333333,0.333333333333333,
0.333333333333333,0.333333333333333,0.333333333333333,0.333333333333333,
0.333333333333333,0.333333333333333,0.333333333333333,0.333333333333333,
0.333333333333333,0.333333333333333,0.333333333333333,0.333333333333333,
0.333333333333333,0.333333333333333,0.333333333333333,0.333333333333333,
0.333333333333333,0.333333333333333,0.333333333333333,0.333333333333333,
0.333333333333333,0.333333333333333,0.333333333333333,0.333333333333333,
0.333333333333333,0.333333333333333,0.333333333333333,0.333333333333333,
0.333333333333333,0.333333333333333,0.333333333333333,0.333333333333333,
0.333333333333333,0.333333333333333,0.333333333333333,0.333333333333333,
0.333333333333333,0.333333333333333,0.333333333333333,0.333333333333333,
0.333333333333333,0.333333333333333,0.333333333333333,0.333333333333333,
0.333333333333333,0.333333333333333,0.333333333333333,0.333333333333333,
0.333333333333333,0.333333333333333,0.333333333333333,0.333333333333333,
0.333333333333333,0.333333333333333,0.333333333333333,0.333333333333333,
0.333333333333333,0.333333333333333,0.333333333333333,0.333333333333333,
0.333333333333333,0.333333333333333,0.333333333333333,0.333333333333333,
0.333333333333333,0.333333333333333,0.333333333333333,0.333333333333333,
0.333333333333333,0.333333333333333,0.333333333333333,0.333333333333333,
0.333333333333333,0.333333333333333,0.333333333333333,0.333333333333333,
0.333333333333333,0.333333333333333,0.333333333333333,0.333333333333333,
0.333333333333333),(1.,1.,1.,1.,1.,1.,1.,1.,1.,1.,1.,1.,1.,1.,1.,1.,1.,
1.,1.,1.,1.,1.,1.,1.,1.,1.,1.,1.,1.,1.,1.,1.,1.,1.,1.,1.,1.,1.,1.,1.,1.,
1.,1.,1.,1.,1.,1.,1.,1.,1.,1.,1.,1.,1.,1.,1.,1.,1.,1.,1.,1.,1.,1.,1.,1.,
1.,1.,1.,1.,1.,1.,1.,1.,1.,1.,1.,1.,1.,1.,1.,1.,1.,1.,1.,1.,1.,1.,1.,1.,
1.,1.,1.,1.,1.,1.,1.,1.,1.,1.,1.,1.,1.,1.,1.,1.,1.,1.,1.,1.,1.,1.,1.,1.,
1.,1.,1.,1.,1.,1.,1.,1.,1.,1.,1.,1.,1.,1.,1.,1.,1.,1.,1.,1.,1.,1.,1.,1.,
1.,1.,1.,1.,1.,1.,1.,1.,1.,1.,1.,1.,1.,1.,1.,1.,1.,1.,1.,1.,1.,1.,1.,1.,
1.,1.,1.,1.,1.,1.,1.),(0.333333333333333,0.333333333333333,0.333333333333333,
0.333333333333333,0.333333333333333,0.333333333333333,0.333333333333333,
0.333333333333333,0.333333333333333,0.333333333333333,0.333333333333333,
0.333333333333333,0.333333333333333,0.333333333333333,0.333333333333333,
0.333333333333333,0.333333333333333,0.333333333333333,0.333333333333333,
0.333333333333333,0.333333333333333,0.333333333333333,0.333333333333333,
0.333333333333333,0.333333333333333,0.333333333333333,0.333333333333333,
0.333333333333333,0.333333333333333,0.333333333333333,0.333333333333333,
0.333333333333333,0.333333333333333,0.333333333333333,0.333333333333333,
0.333333333333333,0.333333333333333,0.333333333333333,0.333333333333333,
0.333333333333333,0.333333333333333,0.333333333333333,0.333333333333333,
0.333333333333333,0.333333333333333,0.333333333333333,0.333333333333333,
0.333333333333333,0.333333333333333,0.333333333333333,0.333333333333333,
0.333333333333333,0.333333333333333,0.333333333333333,0.333333333333333,
0.333333333333333,0.333333333333333,0.333333333333333,0.333333333333333,
0.333333333333333,0.333333333333333,0.333333333333333,0.333333333333333,
0.333333333333333,0.333333333333333,0.333333333333333,0.333333333333333,
0.333333333333333,0.333333333333333,0.333333333333333,0.333333333333333,
0.333333333333333,0.333333333333333,0.333333333333333,0.333333333333333,
0.333333333333333,0.333333333333333,0.333333333333333,0.333333333333333,
0.333333333333333,0.333333333333333,0.333333333333333,0.333333333333333,
0.333333333333333,0.333333333333333,0.333333333333333,0.333333333333333,
0.333333333333333,0.333333333333333,0.333333333333333,0.333333333333333,
0.333333333333333,0.333333333333333,0.333333333333333,0.333333333333333,
0.333333333333333,0.333333333333333,0.333333333333333,0.333333333333333,
0.333333333333333,0.333333333333333,0.333333333333333,0.333333333333333,
0.333333333333333,0.333333333333333,0.333333333333333,0.333333333333333,
0.333333333333333,0.333333333333333,0.333333333333333,0.333333333333333,
0.333333333333333,0.333333333333333,0.333333333333333,0.333333333333333,
0.333333333333333,0.333333333333333,0.333333333333333,0.333333333333333,
0.333333333333333,0.333333333333333,0.333333333333333,0.333333333333333,
0.333333333333333,0.333333333333333,0.333333333333333,0.333333333333333,
0.333333333333333,0.333333333333333,0.333333333333333,0.333333333333333,
0.333333333333333,0.333333333333333,0.333333333333333,0.333333333333333,
0.333333333333333,0.333333333333333,0.333333333333333,0.333333333333333,
0.333333333333333,0.333333333333333,0.333333333333333,0.333333333333333,
0.333333333333333,0.333333333333333,0.333333333333333,0.333333333333333,
0.333333333333333,0.333333333333333,0.333333333333333,0.333333333333333,
0.333333333333333,0.333333333333333,0.333333333333333,0.333333333333333,
0.333333333333333,0.333333333333333,0.333333333333333,0.333333333333333,
0.333333333333333,0.333333333333333,0.333333333333333,0.333333333333333,
0.333333333333333,0.333333333333333,0.333333333333333,0.333333333333333,
0.333333333333333),(0.333333333333333,0.333333333333333,0.333333333333333,
0.333333333333333,0.333333333333333,0.333333333333333,0.333333333333333,
0.333333333333333,0.333333333333333,0.333333333333333,0.333333333333333,
0.333333333333333,0.333333333333333,0.333333333333333,0.333333333333333,
0.333333333333333,0.333333333333333,0.333333333333333,0.333333333333333,
0.333333333333333,0.333333333333333,0.333333333333333,0.333333333333333,
0.333333333333333,0.333333333333333,0.333333333333333,0.333333333333333,
0.333333333333333,0.333333333333333,0.333333333333333,0.333333333333333,
0.333333333333333,0.333333333333333,0.333333333333333,0.333333333333333,
0.333333333333333,0.333333333333333,0.333333333333333,0.333333333333333,
0.333333333333333,0.333333333333333,0.333333333333333,0.333333333333333,
0.333333333333333,0.333333333333333,0.333333333333333,0.333333333333333,
0.333333333333333,0.333333333333333,0.333333333333333,0.333333333333333,
0.333333333333333,0.333333333333333,0.333333333333333,0.333333333333333,
0.333333333333333,0.333333333333333,0.333333333333333,0.333333333333333,
0.333333333333333,0.333333333333333,0.333333333333333,0.333333333333333,
0.333333333333333,0.333333333333333,0.333333333333333,0.333333333333333,
0.333333333333333,0.333333333333333,0.333333333333333,0.333333333333333,
0.333333333333333,0.333333333333333,0.333333333333333,0.333333333333333,
0.333333333333333,0.333333333333333,0.333333333333333,0.333333333333333,
0.333333333333333,0.333333333333333,0.333333333333333,0.333333333333333,
0.333333333333333,0.333333333333333,0.333333333333333,0.333333333333333,
0.333333333333333,0.333333333333333,0.333333333333333,0.333333333333333,
0.333333333333333,0.333333333333333,0.333333333333333,0.333333333333333,
0.333333333333333,0.333333333333333,0.333333333333333,0.333333333333333,
0.333333333333333,0.333333333333333,0.333333333333333,0.333333333333333,
0.333333333333333,0.333333333333333,0.333333333333333,0.333333333333333,
0.333333333333333,0.333333333333333,0.333333333333333,0.333333333333333,
0.333333333333333,0.333333333333333,0.333333333333333,0.333333333333333,
0.333333333333333,0.333333333333333,0.333333333333333,0.333333333333333,
0.333333333333333,0.333333333333333,0.333333333333333,0.333333333333333,
0.333333333333333,0.333333333333333,0.333333333333333,0.333333333333333,
0.333333333333333,0.333333333333333,0.333333333333333,0.333333333333333,
0.333333333333333,0.333333333333333,0.333333333333333,0.333333333333333,
0.333333333333333,0.333333333333333,0.333333333333333,0.333333333333333,
0.333333333333333,0.333333333333333,0.333333333333333,0.333333333333333,
0.333333333333333,0.333333333333333,0.333333333333333,0.333333333333333,
0.333333333333333,0.333333333333333,0.333333333333333,0.333333333333333,
0.333333333333333,0.333333333333333,0.333333333333333,0.333333333333333,
0.333333333333333,0.333333333333333,0.333333333333333,0.333333333333333,
0.333333333333333,0.333333333333333,0.333333333333333,0.333333333333333,
0.333333333333333,0.333333333333333,0.333333333333333,0.333333333333333,
0.333333333333333),(1.,1.,1.,1.,1.,1.,1.,1.,1.,1.,1.,1.,1.,1.,1.,1.,1.,
1.,1.,1.,1.,1.,1.,1.,1.,1.,1.,1.,1.,1.,1.,1.,1.,1.,1.,1.,1.,1.,1.,1.,1.,
1.,1.,1.,1.,1.,1.,1.,1.,1.,1.,1.,1.,1.,1.,1.,1.,1.,1.,1.,1.,1.,1.,1.,1.,
1.,1.,1.,1.,1.,1.,1.,1.,1.,1.,1.,1.,1.,1.,1.,1.,1.,1.,1.,1.,1.,1.,1.,1.,
1.,1.,1.,1.,1.,1.,1.,1.,1.,1.,1.,1.,1.,1.,1.,1.,1.,1.,1.,1.,1.,1.,1.,1.,
1.,1.,1.,1.,1.,1.,1.,1.,1.,1.,1.,1.,1.,1.,1.,1.,1.,1.,1.,1.,1.,1.,1.,1.,
1.,1.,1.,1.,1.,1.,1.,1.,1.,1.,1.,1.,1.,1.,1.,1.,1.,1.,1.,1.,1.,1.,1.,1.,
1.,1.,1.,1.,1.,1.,1.)))
REPRESENTATION_ITEM('')
SURFACE()
);
#528=(
BOUNDED_SURFACE()
B_SPLINE_SURFACE(3,3,((#14000,#14001,#14002,#14003,#14004,#14005,#14006,
#14007,#14008,#14009,#14010,#14011,#14012,#14013,#14014,#14015,#14016,#14017,
#14018,#14019),(#14020,#14021,#14022,#14023,#14024,#14025,#14026,#14027,
#14028,#14029,#14030,#14031,#14032,#14033,#14034,#14035,#14036,#14037,#14038,
#14039),(#14040,#14041,#14042,#14043,#14044,#14045,#14046,#14047,#14048,
#14049,#14050,#14051,#14052,#14053,#14054,#14055,#14056,#14057,#14058,#14059),
(#14060,#14061,#14062,#14063,#14064,#14065,#14066,#14067,#14068,#14069,
#14070,#14071,#14072,#14073,#14074,#14075,#14076,#14077,#14078,#14079),
(#14080,#14081,#14082,#14083,#14084,#14085,#14086,#14087,#14088,#14089,
#14090,#14091,#14092,#14093,#14094,#14095,#14096,#14097,#14098,#14099),
(#14100,#14101,#14102,#14103,#14104,#14105,#14106,#14107,#14108,#14109,
#14110,#14111,#14112,#14113,#14114,#14115,#14116,#14117,#14118,#14119),
(#14120,#14121,#14122,#14123,#14124,#14125,#14126,#14127,#14128,#14129,
#14130,#14131,#14132,#14133,#14134,#14135,#14136,#14137,#14138,#14139)),
 .UNSPECIFIED.,.T.,.F.,.F.)
B_SPLINE_SURFACE_WITH_KNOTS((4,3,4),(4,2,2,2,2,2,2,2,2,4),(0.,0.5,1.),(0.0618954463697512,
0.0653601604005303,0.0688248744313094,0.0757543024928677,0.0792190165236468,
0.0809513735390363,0.0826837305544259,0.086148444585205,0.0878808016005946,
0.0896131586159842),.UNSPECIFIED.)
GEOMETRIC_REPRESENTATION_ITEM()
RATIONAL_B_SPLINE_SURFACE(((1.,1.,1.,1.,1.,1.,1.,1.,1.,1.,1.,1.,1.,1.,1.,
1.,1.,1.,1.,1.),(0.333333333333333,0.333333333333333,0.333333333333333,
0.333333333333333,0.333333333333333,0.333333333333333,0.333333333333333,
0.333333333333333,0.333333333333333,0.333333333333333,0.333333333333333,
0.333333333333333,0.333333333333333,0.333333333333333,0.333333333333333,
0.333333333333333,0.333333333333333,0.333333333333333,0.333333333333333,
0.333333333333333),(0.333333333333333,0.333333333333333,0.333333333333333,
0.333333333333333,0.333333333333333,0.333333333333333,0.333333333333333,
0.333333333333333,0.333333333333333,0.333333333333333,0.333333333333333,
0.333333333333333,0.333333333333333,0.333333333333333,0.333333333333333,
0.333333333333333,0.333333333333333,0.333333333333333,0.333333333333333,
0.333333333333333),(1.,1.,1.,1.,1.,1.,1.,1.,1.,1.,1.,1.,1.,1.,1.,1.,1.,
1.,1.,1.),(0.333333333333333,0.333333333333333,0.333333333333333,0.333333333333333,
0.333333333333333,0.333333333333333,0.333333333333333,0.333333333333333,
0.333333333333333,0.333333333333333,0.333333333333333,0.333333333333333,
0.333333333333333,0.333333333333333,0.333333333333333,0.333333333333333,
0.333333333333333,0.333333333333333,0.333333333333333,0.333333333333333),
(0.333333333333333,0.333333333333333,0.333333333333333,0.333333333333333,
0.333333333333333,0.333333333333333,0.333333333333333,0.333333333333333,
0.333333333333333,0.333333333333333,0.333333333333333,0.333333333333333,
0.333333333333333,0.333333333333333,0.333333333333333,0.333333333333333,
0.333333333333333,0.333333333333333,0.333333333333333,0.333333333333333),
(1.,1.,1.,1.,1.,1.,1.,1.,1.,1.,1.,1.,1.,1.,1.,1.,1.,1.,1.,1.)))
REPRESENTATION_ITEM('')
SURFACE()
);
#529=(
BOUNDED_SURFACE()
B_SPLINE_SURFACE(3,3,((#14186,#14187,#14188,#14189,#14190,#14191,#14192,
#14193,#14194,#14195,#14196,#14197,#14198,#14199,#14200,#14201,#14202,#14203,
#14204,#14205,#14206,#14207,#14208,#14209),(#14210,#14211,#14212,#14213,
#14214,#14215,#14216,#14217,#14218,#14219,#14220,#14221,#14222,#14223,#14224,
#14225,#14226,#14227,#14228,#14229,#14230,#14231,#14232,#14233),(#14234,
#14235,#14236,#14237,#14238,#14239,#14240,#14241,#14242,#14243,#14244,#14245,
#14246,#14247,#14248,#14249,#14250,#14251,#14252,#14253,#14254,#14255,#14256,
#14257),(#14258,#14259,#14260,#14261,#14262,#14263,#14264,#14265,#14266,
#14267,#14268,#14269,#14270,#14271,#14272,#14273,#14274,#14275,#14276,#14277,
#14278,#14279,#14280,#14281),(#14282,#14283,#14284,#14285,#14286,#14287,
#14288,#14289,#14290,#14291,#14292,#14293,#14294,#14295,#14296,#14297,#14298,
#14299,#14300,#14301,#14302,#14303,#14304,#14305),(#14306,#14307,#14308,
#14309,#14310,#14311,#14312,#14313,#14314,#14315,#14316,#14317,#14318,#14319,
#14320,#14321,#14322,#14323,#14324,#14325,#14326,#14327,#14328,#14329),
(#14330,#14331,#14332,#14333,#14334,#14335,#14336,#14337,#14338,#14339,
#14340,#14341,#14342,#14343,#14344,#14345,#14346,#14347,#14348,#14349,#14350,
#14351,#14352,#14353)),.UNSPECIFIED.,.T.,.F.,.F.)
B_SPLINE_SURFACE_WITH_KNOTS((4,3,4),(4,2,2,2,2,2,2,2,2,2,2,4),(0.,0.5,1.),
(0.916063809045508,0.917441355582055,0.918818902118601,0.921573995191693,
0.924329088264786,0.925706634801332,0.927084181337879,0.932594367484064,
0.935349460557156,0.936727007093702,0.937415780361976,0.938104553630249),
 .UNSPECIFIED.)
GEOMETRIC_REPRESENTATION_ITEM()
RATIONAL_B_SPLINE_SURFACE(((1.,1.,1.,1.,1.,1.,1.,1.,1.,1.,1.,1.,1.,1.,1.,
1.,1.,1.,1.,1.,1.,1.,1.,1.),(0.333333333333333,0.333333333333333,0.333333333333333,
0.333333333333333,0.333333333333333,0.333333333333333,0.333333333333333,
0.333333333333333,0.333333333333333,0.333333333333333,0.333333333333333,
0.333333333333333,0.333333333333333,0.333333333333333,0.333333333333333,
0.333333333333333,0.333333333333333,0.333333333333333,0.333333333333333,
0.333333333333333,0.333333333333333,0.333333333333333,0.333333333333333,
0.333333333333333),(0.333333333333333,0.333333333333333,0.333333333333333,
0.333333333333333,0.333333333333333,0.333333333333333,0.333333333333333,
0.333333333333333,0.333333333333333,0.333333333333333,0.333333333333333,
0.333333333333333,0.333333333333333,0.333333333333333,0.333333333333333,
0.333333333333333,0.333333333333333,0.333333333333333,0.333333333333333,
0.333333333333333,0.333333333333333,0.333333333333333,0.333333333333333,
0.333333333333333),(1.,1.,1.,1.,1.,1.,1.,1.,1.,1.,1.,1.,1.,1.,1.,1.,1.,
1.,1.,1.,1.,1.,1.,1.),(0.333333333333333,0.333333333333333,0.333333333333333,
0.333333333333333,0.333333333333333,0.333333333333333,0.333333333333333,
0.333333333333333,0.333333333333333,0.333333333333333,0.333333333333333,
0.333333333333333,0.333333333333333,0.333333333333333,0.333333333333333,
0.333333333333333,0.333333333333333,0.333333333333333,0.333333333333333,
0.333333333333333,0.333333333333333,0.333333333333333,0.333333333333333,
0.333333333333333),(0.333333333333333,0.333333333333333,0.333333333333333,
0.333333333333333,0.333333333333333,0.333333333333333,0.333333333333333,
0.333333333333333,0.333333333333333,0.333333333333333,0.333333333333333,
0.333333333333333,0.333333333333333,0.333333333333333,0.333333333333333,
0.333333333333333,0.333333333333333,0.333333333333333,0.333333333333333,
0.333333333333333,0.333333333333333,0.333333333333333,0.333333333333333,
0.333333333333333),(1.,1.,1.,1.,1.,1.,1.,1.,1.,1.,1.,1.,1.,1.,1.,1.,1.,
1.,1.,1.,1.,1.,1.,1.)))
REPRESENTATION_ITEM('')
SURFACE()
);
#530=(
BOUNDED_SURFACE()
B_SPLINE_SURFACE(3,3,((#14355,#14356,#14357,#14358,#14359,#14360,#14361,
#14362,#14363,#14364,#14365,#14366,#14367,#14368,#14369,#14370,#14371,#14372,
#14373,#14374,#14375,#14376,#14377,#14378,#14379,#14380,#14381,#14382,#14383,
#14384,#14385,#14386,#14387,#14388,#14389,#14390,#14391,#14392,#14393,#14394,
#14395,#14396,#14397,#14398,#14399,#14400,#14401,#14402,#14403,#14404,#14405,
#14406,#14407,#14408,#14409,#14410,#14411,#14412,#14413,#14414,#14415,#14416,
#14417,#14418,#14419,#14420,#14421,#14422,#14423,#14424,#14425,#14426,#14427,
#14428,#14429,#14430,#14431,#14432,#14433,#14434,#14435,#14436,#14437,#14438,
#14439,#14440,#14441,#14442,#14443,#14444,#14445,#14446,#14447,#14448,#14449,
#14450,#14451,#14452,#14453,#14454,#14455,#14456,#14457,#14458,#14459,#14460,
#14461,#14462,#14463,#14464,#14465,#14466,#14467,#14468,#14469,#14470,#14471,
#14472,#14473,#14474,#14475,#14476,#14477,#14478,#14479,#14480,#14481,#14482,
#14483,#14484,#14485,#14486,#14487,#14488,#14489,#14490,#14491,#14492,#14493,
#14494,#14495,#14496,#14497,#14498,#14499,#14500,#14501,#14502,#14503,#14504,
#14505,#14506,#14507,#14508,#14509,#14510,#14511,#14512,#14513,#14514,#14515,
#14516,#14517,#14518,#14519,#14520,#14521,#14522),(#14523,#14524,#14525,
#14526,#14527,#14528,#14529,#14530,#14531,#14532,#14533,#14534,#14535,#14536,
#14537,#14538,#14539,#14540,#14541,#14542,#14543,#14544,#14545,#14546,#14547,
#14548,#14549,#14550,#14551,#14552,#14553,#14554,#14555,#14556,#14557,#14558,
#14559,#14560,#14561,#14562,#14563,#14564,#14565,#14566,#14567,#14568,#14569,
#14570,#14571,#14572,#14573,#14574,#14575,#14576,#14577,#14578,#14579,#14580,
#14581,#14582,#14583,#14584,#14585,#14586,#14587,#14588,#14589,#14590,#14591,
#14592,#14593,#14594,#14595,#14596,#14597,#14598,#14599,#14600,#14601,#14602,
#14603,#14604,#14605,#14606,#14607,#14608,#14609,#14610,#14611,#14612,#14613,
#14614,#14615,#14616,#14617,#14618,#14619,#14620,#14621,#14622,#14623,#14624,
#14625,#14626,#14627,#14628,#14629,#14630,#14631,#14632,#14633,#14634,#14635,
#14636,#14637,#14638,#14639,#14640,#14641,#14642,#14643,#14644,#14645,#14646,
#14647,#14648,#14649,#14650,#14651,#14652,#14653,#14654,#14655,#14656,#14657,
#14658,#14659,#14660,#14661,#14662,#14663,#14664,#14665,#14666,#14667,#14668,
#14669,#14670,#14671,#14672,#14673,#14674,#14675,#14676,#14677,#14678,#14679,
#14680,#14681,#14682,#14683,#14684,#14685,#14686,#14687,#14688,#14689,#14690),
(#14691,#14692,#14693,#14694,#14695,#14696,#14697,#14698,#14699,#14700,
#14701,#14702,#14703,#14704,#14705,#14706,#14707,#14708,#14709,#14710,#14711,
#14712,#14713,#14714,#14715,#14716,#14717,#14718,#14719,#14720,#14721,#14722,
#14723,#14724,#14725,#14726,#14727,#14728,#14729,#14730,#14731,#14732,#14733,
#14734,#14735,#14736,#14737,#14738,#14739,#14740,#14741,#14742,#14743,#14744,
#14745,#14746,#14747,#14748,#14749,#14750,#14751,#14752,#14753,#14754,#14755,
#14756,#14757,#14758,#14759,#14760,#14761,#14762,#14763,#14764,#14765,#14766,
#14767,#14768,#14769,#14770,#14771,#14772,#14773,#14774,#14775,#14776,#14777,
#14778,#14779,#14780,#14781,#14782,#14783,#14784,#14785,#14786,#14787,#14788,
#14789,#14790,#14791,#14792,#14793,#14794,#14795,#14796,#14797,#14798,#14799,
#14800,#14801,#14802,#14803,#14804,#14805,#14806,#14807,#14808,#14809,#14810,
#14811,#14812,#14813,#14814,#14815,#14816,#14817,#14818,#14819,#14820,#14821,
#14822,#14823,#14824,#14825,#14826,#14827,#14828,#14829,#14830,#14831,#14832,
#14833,#14834,#14835,#14836,#14837,#14838,#14839,#14840,#14841,#14842,#14843,
#14844,#14845,#14846,#14847,#14848,#14849,#14850,#14851,#14852,#14853,#14854,
#14855,#14856,#14857,#14858),(#14859,#14860,#14861,#14862,#14863,#14864,
#14865,#14866,#14867,#14868,#14869,#14870,#14871,#14872,#14873,#14874,#14875,
#14876,#14877,#14878,#14879,#14880,#14881,#14882,#14883,#14884,#14885,#14886,
#14887,#14888,#14889,#14890,#14891,#14892,#14893,#14894,#14895,#14896,#14897,
#14898,#14899,#14900,#14901,#14902,#14903,#14904,#14905,#14906,#14907,#14908,
#14909,#14910,#14911,#14912,#14913,#14914,#14915,#14916,#14917,#14918,#14919,
#14920,#14921,#14922,#14923,#14924,#14925,#14926,#14927,#14928,#14929,#14930,
#14931,#14932,#14933,#14934,#14935,#14936,#14937,#14938,#14939,#14940,#14941,
#14942,#14943,#14944,#14945,#14946,#14947,#14948,#14949,#14950,#14951,#14952,
#14953,#14954,#14955,#14956,#14957,#14958,#14959,#14960,#14961,#14962,#14963,
#14964,#14965,#14966,#14967,#14968,#14969,#14970,#14971,#14972,#14973,#14974,
#14975,#14976,#14977,#14978,#14979,#14980,#14981,#14982,#14983,#14984,#14985,
#14986,#14987,#14988,#14989,#14990,#14991,#14992,#14993,#14994,#14995,#14996,
#14997,#14998,#14999,#15000,#15001,#15002,#15003,#15004,#15005,#15006,#15007,
#15008,#15009,#15010,#15011,#15012,#15013,#15014,#15015,#15016,#15017,#15018,
#15019,#15020,#15021,#15022,#15023,#15024,#15025,#15026),(#15027,#15028,
#15029,#15030,#15031,#15032,#15033,#15034,#15035,#15036,#15037,#15038,#15039,
#15040,#15041,#15042,#15043,#15044,#15045,#15046,#15047,#15048,#15049,#15050,
#15051,#15052,#15053,#15054,#15055,#15056,#15057,#15058,#15059,#15060,#15061,
#15062,#15063,#15064,#15065,#15066,#15067,#15068,#15069,#15070,#15071,#15072,
#15073,#15074,#15075,#15076,#15077,#15078,#15079,#15080,#15081,#15082,#15083,
#15084,#15085,#15086,#15087,#15088,#15089,#15090,#15091,#15092,#15093,#15094,
#15095,#15096,#15097,#15098,#15099,#15100,#15101,#15102,#15103,#15104,#15105,
#15106,#15107,#15108,#15109,#15110,#15111,#15112,#15113,#15114,#15115,#15116,
#15117,#15118,#15119,#15120,#15121,#15122,#15123,#15124,#15125,#15126,#15127,
#15128,#15129,#15130,#15131,#15132,#15133,#15134,#15135,#15136,#15137,#15138,
#15139,#15140,#15141,#15142,#15143,#15144,#15145,#15146,#15147,#15148,#15149,
#15150,#15151,#15152,#15153,#15154,#15155,#15156,#15157,#15158,#15159,#15160,
#15161,#15162,#15163,#15164,#15165,#15166,#15167,#15168,#15169,#15170,#15171,
#15172,#15173,#15174,#15175,#15176,#15177,#15178,#15179,#15180,#15181,#15182,
#15183,#15184,#15185,#15186,#15187,#15188,#15189,#15190,#15191,#15192,#15193,
#15194),(#15195,#15196,#15197,#15198,#15199,#15200,#15201,#15202,#15203,
#15204,#15205,#15206,#15207,#15208,#15209,#15210,#15211,#15212,#15213,#15214,
#15215,#15216,#15217,#15218,#15219,#15220,#15221,#15222,#15223,#15224,#15225,
#15226,#15227,#15228,#15229,#15230,#15231,#15232,#15233,#15234,#15235,#15236,
#15237,#15238,#15239,#15240,#15241,#15242,#15243,#15244,#15245,#15246,#15247,
#15248,#15249,#15250,#15251,#15252,#15253,#15254,#15255,#15256,#15257,#15258,
#15259,#15260,#15261,#15262,#15263,#15264,#15265,#15266,#15267,#15268,#15269,
#15270,#15271,#15272,#15273,#15274,#15275,#15276,#15277,#15278,#15279,#15280,
#15281,#15282,#15283,#15284,#15285,#15286,#15287,#15288,#15289,#15290,#15291,
#15292,#15293,#15294,#15295,#15296,#15297,#15298,#15299,#15300,#15301,#15302,
#15303,#15304,#15305,#15306,#15307,#15308,#15309,#15310,#15311,#15312,#15313,
#15314,#15315,#15316,#15317,#15318,#15319,#15320,#15321,#15322,#15323,#15324,
#15325,#15326,#15327,#15328,#15329,#15330,#15331,#15332,#15333,#15334,#15335,
#15336,#15337,#15338,#15339,#15340,#15341,#15342,#15343,#15344,#15345,#15346,
#15347,#15348,#15349,#15350,#15351,#15352,#15353,#15354,#15355,#15356,#15357,
#15358,#15359,#15360,#15361,#15362),(#15363,#15364,#15365,#15366,#15367,
#15368,#15369,#15370,#15371,#15372,#15373,#15374,#15375,#15376,#15377,#15378,
#15379,#15380,#15381,#15382,#15383,#15384,#15385,#15386,#15387,#15388,#15389,
#15390,#15391,#15392,#15393,#15394,#15395,#15396,#15397,#15398,#15399,#15400,
#15401,#15402,#15403,#15404,#15405,#15406,#15407,#15408,#15409,#15410,#15411,
#15412,#15413,#15414,#15415,#15416,#15417,#15418,#15419,#15420,#15421,#15422,
#15423,#15424,#15425,#15426,#15427,#15428,#15429,#15430,#15431,#15432,#15433,
#15434,#15435,#15436,#15437,#15438,#15439,#15440,#15441,#15442,#15443,#15444,
#15445,#15446,#15447,#15448,#15449,#15450,#15451,#15452,#15453,#15454,#15455,
#15456,#15457,#15458,#15459,#15460,#15461,#15462,#15463,#15464,#15465,#15466,
#15467,#15468,#15469,#15470,#15471,#15472,#15473,#15474,#15475,#15476,#15477,
#15478,#15479,#15480,#15481,#15482,#15483,#15484,#15485,#15486,#15487,#15488,
#15489,#15490,#15491,#15492,#15493,#15494,#15495,#15496,#15497,#15498,#15499,
#15500,#15501,#15502,#15503,#15504,#15505,#15506,#15507,#15508,#15509,#15510,
#15511,#15512,#15513,#15514,#15515,#15516,#15517,#15518,#15519,#15520,#15521,
#15522,#15523,#15524,#15525,#15526,#15527,#15528,#15529,#15530)),
 .UNSPECIFIED.,.T.,.F.,.F.)
B_SPLINE_SURFACE_WITH_KNOTS((4,3,4),(4,2,2,2,2,2,2,2,2,2,2,2,2,2,2,2,2,
2,2,2,2,2,2,2,2,2,2,2,2,2,2,2,2,2,2,2,2,2,2,2,2,2,2,2,2,2,2,2,2,2,2,2,2,
2,2,2,2,2,2,2,2,2,2,2,2,2,2,2,2,2,2,2,2,2,2,2,2,2,2,2,2,2,2,4),(0.,0.5,
1.),(0.0896131586159842,0.0909349273058256,0.092256695995667,0.09490023337535,
0.100187308134716,0.110761457653447,0.121335607172179,0.131909756690911,
0.142406945548381,0.152904134405852,0.163401323263323,0.173898512120793,
0.184326267064866,0.194754022008939,0.205181776953011,0.215609531897084,
0.225968774255778,0.236328016614473,0.246687258973167,0.257046501331861,
0.268365392558388,0.279684283784914,0.29100317501144,0.302322066237966,
0.313563979866736,0.324805893495506,0.336047807124276,0.347289720753047,
0.358457560536344,0.369625400319641,0.380793240102939,0.391961079886236,
0.403057648451734,0.414154217017233,0.425250785582731,0.43634735414823,
0.447375242283774,0.458403130419317,0.469431018554861,0.480458906690405,
0.491420626849432,0.50238234700846,0.513344067167488,0.524305787326516,
0.535203741266554,0.546101695206592,0.55699964914663,0.567897603086667,
0.578734005374906,0.589570407663145,0.600406809951383,0.611243212239622,
0.62202044333232,0.632797674425018,0.643574905517716,0.654352136610414,
0.665072195325672,0.675792254040929,0.686512312756186,0.697232371471444,
0.707897173370898,0.718561975270352,0.729226777169807,0.739891579069261,
0.750503305564763,0.761115032060264,0.771726758555766,0.782338485051267,
0.79289871583597,0.803458946620673,0.814019177405375,0.824579408190078,
0.835090233536042,0.845601058882007,0.856111884227971,0.866622709573936,
0.877085607262584,0.887548504951232,0.89801140263988,0.908474300328528,
0.912269054687018,0.914166431866263,0.915115120455886,0.916063809045508),
 .UNSPECIFIED.)
GEOMETRIC_REPRESENTATION_ITEM()
RATIONAL_B_SPLINE_SURFACE(((1.,1.,1.,1.,1.,1.,1.,1.,1.,1.,1.,1.,1.,1.,1.,
1.,1.,1.,1.,1.,1.,1.,1.,1.,1.,1.,1.,1.,1.,1.,1.,1.,1.,1.,1.,1.,1.,1.,1.,
1.,1.,1.,1.,1.,1.,1.,1.,1.,1.,1.,1.,1.,1.,1.,1.,1.,1.,1.,1.,1.,1.,1.,1.,
1.,1.,1.,1.,1.,1.,1.,1.,1.,1.,1.,1.,1.,1.,1.,1.,1.,1.,1.,1.,1.,1.,1.,1.,
1.,1.,1.,1.,1.,1.,1.,1.,1.,1.,1.,1.,1.,1.,1.,1.,1.,1.,1.,1.,1.,1.,1.,1.,
1.,1.,1.,1.,1.,1.,1.,1.,1.,1.,1.,1.,1.,1.,1.,1.,1.,1.,1.,1.,1.,1.,1.,1.,
1.,1.,1.,1.,1.,1.,1.,1.,1.,1.,1.,1.,1.,1.,1.,1.,1.,1.,1.,1.,1.,1.,1.,1.,
1.,1.,1.,1.,1.,1.,1.,1.,1.),(0.333333333333333,0.333333333333333,0.333333333333333,
0.333333333333333,0.333333333333333,0.333333333333333,0.333333333333333,
0.333333333333333,0.333333333333333,0.333333333333333,0.333333333333333,
0.333333333333333,0.333333333333333,0.333333333333333,0.333333333333333,
0.333333333333333,0.333333333333333,0.333333333333333,0.333333333333333,
0.333333333333333,0.333333333333333,0.333333333333333,0.333333333333333,
0.333333333333333,0.333333333333333,0.333333333333333,0.333333333333333,
0.333333333333333,0.333333333333333,0.333333333333333,0.333333333333333,
0.333333333333333,0.333333333333333,0.333333333333333,0.333333333333333,
0.333333333333333,0.333333333333333,0.333333333333333,0.333333333333333,
0.333333333333333,0.333333333333333,0.333333333333333,0.333333333333333,
0.333333333333333,0.333333333333333,0.333333333333333,0.333333333333333,
0.333333333333333,0.333333333333333,0.333333333333333,0.333333333333333,
0.333333333333333,0.333333333333333,0.333333333333333,0.333333333333333,
0.333333333333333,0.333333333333333,0.333333333333333,0.333333333333333,
0.333333333333333,0.333333333333333,0.333333333333333,0.333333333333333,
0.333333333333333,0.333333333333333,0.333333333333333,0.333333333333333,
0.333333333333333,0.333333333333333,0.333333333333333,0.333333333333333,
0.333333333333333,0.333333333333333,0.333333333333333,0.333333333333333,
0.333333333333333,0.333333333333333,0.333333333333333,0.333333333333333,
0.333333333333333,0.333333333333333,0.333333333333333,0.333333333333333,
0.333333333333333,0.333333333333333,0.333333333333333,0.333333333333333,
0.333333333333333,0.333333333333333,0.333333333333333,0.333333333333333,
0.333333333333333,0.333333333333333,0.333333333333333,0.333333333333333,
0.333333333333333,0.333333333333333,0.333333333333333,0.333333333333333,
0.333333333333333,0.333333333333333,0.333333333333333,0.333333333333333,
0.333333333333333,0.333333333333333,0.333333333333333,0.333333333333333,
0.333333333333333,0.333333333333333,0.333333333333333,0.333333333333333,
0.333333333333333,0.333333333333333,0.333333333333333,0.333333333333333,
0.333333333333333,0.333333333333333,0.333333333333333,0.333333333333333,
0.333333333333333,0.333333333333333,0.333333333333333,0.333333333333333,
0.333333333333333,0.333333333333333,0.333333333333333,0.333333333333333,
0.333333333333333,0.333333333333333,0.333333333333333,0.333333333333333,
0.333333333333333,0.333333333333333,0.333333333333333,0.333333333333333,
0.333333333333333,0.333333333333333,0.333333333333333,0.333333333333333,
0.333333333333333,0.333333333333333,0.333333333333333,0.333333333333333,
0.333333333333333,0.333333333333333,0.333333333333333,0.333333333333333,
0.333333333333333,0.333333333333333,0.333333333333333,0.333333333333333,
0.333333333333333,0.333333333333333,0.333333333333333,0.333333333333333,
0.333333333333333,0.333333333333333,0.333333333333333,0.333333333333333,
0.333333333333333,0.333333333333333,0.333333333333333,0.333333333333333,
0.333333333333333,0.333333333333333,0.333333333333333,0.333333333333333,
0.333333333333333),(0.333333333333333,0.333333333333333,0.333333333333333,
0.333333333333333,0.333333333333333,0.333333333333333,0.333333333333333,
0.333333333333333,0.333333333333333,0.333333333333333,0.333333333333333,
0.333333333333333,0.333333333333333,0.333333333333333,0.333333333333333,
0.333333333333333,0.333333333333333,0.333333333333333,0.333333333333333,
0.333333333333333,0.333333333333333,0.333333333333333,0.333333333333333,
0.333333333333333,0.333333333333333,0.333333333333333,0.333333333333333,
0.333333333333333,0.333333333333333,0.333333333333333,0.333333333333333,
0.333333333333333,0.333333333333333,0.333333333333333,0.333333333333333,
0.333333333333333,0.333333333333333,0.333333333333333,0.333333333333333,
0.333333333333333,0.333333333333333,0.333333333333333,0.333333333333333,
0.333333333333333,0.333333333333333,0.333333333333333,0.333333333333333,
0.333333333333333,0.333333333333333,0.333333333333333,0.333333333333333,
0.333333333333333,0.333333333333333,0.333333333333333,0.333333333333333,
0.333333333333333,0.333333333333333,0.333333333333333,0.333333333333333,
0.333333333333333,0.333333333333333,0.333333333333333,0.333333333333333,
0.333333333333333,0.333333333333333,0.333333333333333,0.333333333333333,
0.333333333333333,0.333333333333333,0.333333333333333,0.333333333333333,
0.333333333333333,0.333333333333333,0.333333333333333,0.333333333333333,
0.333333333333333,0.333333333333333,0.333333333333333,0.333333333333333,
0.333333333333333,0.333333333333333,0.333333333333333,0.333333333333333,
0.333333333333333,0.333333333333333,0.333333333333333,0.333333333333333,
0.333333333333333,0.333333333333333,0.333333333333333,0.333333333333333,
0.333333333333333,0.333333333333333,0.333333333333333,0.333333333333333,
0.333333333333333,0.333333333333333,0.333333333333333,0.333333333333333,
0.333333333333333,0.333333333333333,0.333333333333333,0.333333333333333,
0.333333333333333,0.333333333333333,0.333333333333333,0.333333333333333,
0.333333333333333,0.333333333333333,0.333333333333333,0.333333333333333,
0.333333333333333,0.333333333333333,0.333333333333333,0.333333333333333,
0.333333333333333,0.333333333333333,0.333333333333333,0.333333333333333,
0.333333333333333,0.333333333333333,0.333333333333333,0.333333333333333,
0.333333333333333,0.333333333333333,0.333333333333333,0.333333333333333,
0.333333333333333,0.333333333333333,0.333333333333333,0.333333333333333,
0.333333333333333,0.333333333333333,0.333333333333333,0.333333333333333,
0.333333333333333,0.333333333333333,0.333333333333333,0.333333333333333,
0.333333333333333,0.333333333333333,0.333333333333333,0.333333333333333,
0.333333333333333,0.333333333333333,0.333333333333333,0.333333333333333,
0.333333333333333,0.333333333333333,0.333333333333333,0.333333333333333,
0.333333333333333,0.333333333333333,0.333333333333333,0.333333333333333,
0.333333333333333,0.333333333333333,0.333333333333333,0.333333333333333,
0.333333333333333,0.333333333333333,0.333333333333333,0.333333333333333,
0.333333333333333,0.333333333333333,0.333333333333333,0.333333333333333,
0.333333333333333),(1.,1.,1.,1.,1.,1.,1.,1.,1.,1.,1.,1.,1.,1.,1.,1.,1.,
1.,1.,1.,1.,1.,1.,1.,1.,1.,1.,1.,1.,1.,1.,1.,1.,1.,1.,1.,1.,1.,1.,1.,1.,
1.,1.,1.,1.,1.,1.,1.,1.,1.,1.,1.,1.,1.,1.,1.,1.,1.,1.,1.,1.,1.,1.,1.,1.,
1.,1.,1.,1.,1.,1.,1.,1.,1.,1.,1.,1.,1.,1.,1.,1.,1.,1.,1.,1.,1.,1.,1.,1.,
1.,1.,1.,1.,1.,1.,1.,1.,1.,1.,1.,1.,1.,1.,1.,1.,1.,1.,1.,1.,1.,1.,1.,1.,
1.,1.,1.,1.,1.,1.,1.,1.,1.,1.,1.,1.,1.,1.,1.,1.,1.,1.,1.,1.,1.,1.,1.,1.,
1.,1.,1.,1.,1.,1.,1.,1.,1.,1.,1.,1.,1.,1.,1.,1.,1.,1.,1.,1.,1.,1.,1.,1.,
1.,1.,1.,1.,1.,1.,1.),(0.333333333333333,0.333333333333333,0.333333333333333,
0.333333333333333,0.333333333333333,0.333333333333333,0.333333333333333,
0.333333333333333,0.333333333333333,0.333333333333333,0.333333333333333,
0.333333333333333,0.333333333333333,0.333333333333333,0.333333333333333,
0.333333333333333,0.333333333333333,0.333333333333333,0.333333333333333,
0.333333333333333,0.333333333333333,0.333333333333333,0.333333333333333,
0.333333333333333,0.333333333333333,0.333333333333333,0.333333333333333,
0.333333333333333,0.333333333333333,0.333333333333333,0.333333333333333,
0.333333333333333,0.333333333333333,0.333333333333333,0.333333333333333,
0.333333333333333,0.333333333333333,0.333333333333333,0.333333333333333,
0.333333333333333,0.333333333333333,0.333333333333333,0.333333333333333,
0.333333333333333,0.333333333333333,0.333333333333333,0.333333333333333,
0.333333333333333,0.333333333333333,0.333333333333333,0.333333333333333,
0.333333333333333,0.333333333333333,0.333333333333333,0.333333333333333,
0.333333333333333,0.333333333333333,0.333333333333333,0.333333333333333,
0.333333333333333,0.333333333333333,0.333333333333333,0.333333333333333,
0.333333333333333,0.333333333333333,0.333333333333333,0.333333333333333,
0.333333333333333,0.333333333333333,0.333333333333333,0.333333333333333,
0.333333333333333,0.333333333333333,0.333333333333333,0.333333333333333,
0.333333333333333,0.333333333333333,0.333333333333333,0.333333333333333,
0.333333333333333,0.333333333333333,0.333333333333333,0.333333333333333,
0.333333333333333,0.333333333333333,0.333333333333333,0.333333333333333,
0.333333333333333,0.333333333333333,0.333333333333333,0.333333333333333,
0.333333333333333,0.333333333333333,0.333333333333333,0.333333333333333,
0.333333333333333,0.333333333333333,0.333333333333333,0.333333333333333,
0.333333333333333,0.333333333333333,0.333333333333333,0.333333333333333,
0.333333333333333,0.333333333333333,0.333333333333333,0.333333333333333,
0.333333333333333,0.333333333333333,0.333333333333333,0.333333333333333,
0.333333333333333,0.333333333333333,0.333333333333333,0.333333333333333,
0.333333333333333,0.333333333333333,0.333333333333333,0.333333333333333,
0.333333333333333,0.333333333333333,0.333333333333333,0.333333333333333,
0.333333333333333,0.333333333333333,0.333333333333333,0.333333333333333,
0.333333333333333,0.333333333333333,0.333333333333333,0.333333333333333,
0.333333333333333,0.333333333333333,0.333333333333333,0.333333333333333,
0.333333333333333,0.333333333333333,0.333333333333333,0.333333333333333,
0.333333333333333,0.333333333333333,0.333333333333333,0.333333333333333,
0.333333333333333,0.333333333333333,0.333333333333333,0.333333333333333,
0.333333333333333,0.333333333333333,0.333333333333333,0.333333333333333,
0.333333333333333,0.333333333333333,0.333333333333333,0.333333333333333,
0.333333333333333,0.333333333333333,0.333333333333333,0.333333333333333,
0.333333333333333,0.333333333333333,0.333333333333333,0.333333333333333,
0.333333333333333,0.333333333333333,0.333333333333333,0.333333333333333,
0.333333333333333),(0.333333333333333,0.333333333333333,0.333333333333333,
0.333333333333333,0.333333333333333,0.333333333333333,0.333333333333333,
0.333333333333333,0.333333333333333,0.333333333333333,0.333333333333333,
0.333333333333333,0.333333333333333,0.333333333333333,0.333333333333333,
0.333333333333333,0.333333333333333,0.333333333333333,0.333333333333333,
0.333333333333333,0.333333333333333,0.333333333333333,0.333333333333333,
0.333333333333333,0.333333333333333,0.333333333333333,0.333333333333333,
0.333333333333333,0.333333333333333,0.333333333333333,0.333333333333333,
0.333333333333333,0.333333333333333,0.333333333333333,0.333333333333333,
0.333333333333333,0.333333333333333,0.333333333333333,0.333333333333333,
0.333333333333333,0.333333333333333,0.333333333333333,0.333333333333333,
0.333333333333333,0.333333333333333,0.333333333333333,0.333333333333333,
0.333333333333333,0.333333333333333,0.333333333333333,0.333333333333333,
0.333333333333333,0.333333333333333,0.333333333333333,0.333333333333333,
0.333333333333333,0.333333333333333,0.333333333333333,0.333333333333333,
0.333333333333333,0.333333333333333,0.333333333333333,0.333333333333333,
0.333333333333333,0.333333333333333,0.333333333333333,0.333333333333333,
0.333333333333333,0.333333333333333,0.333333333333333,0.333333333333333,
0.333333333333333,0.333333333333333,0.333333333333333,0.333333333333333,
0.333333333333333,0.333333333333333,0.333333333333333,0.333333333333333,
0.333333333333333,0.333333333333333,0.333333333333333,0.333333333333333,
0.333333333333333,0.333333333333333,0.333333333333333,0.333333333333333,
0.333333333333333,0.333333333333333,0.333333333333333,0.333333333333333,
0.333333333333333,0.333333333333333,0.333333333333333,0.333333333333333,
0.333333333333333,0.333333333333333,0.333333333333333,0.333333333333333,
0.333333333333333,0.333333333333333,0.333333333333333,0.333333333333333,
0.333333333333333,0.333333333333333,0.333333333333333,0.333333333333333,
0.333333333333333,0.333333333333333,0.333333333333333,0.333333333333333,
0.333333333333333,0.333333333333333,0.333333333333333,0.333333333333333,
0.333333333333333,0.333333333333333,0.333333333333333,0.333333333333333,
0.333333333333333,0.333333333333333,0.333333333333333,0.333333333333333,
0.333333333333333,0.333333333333333,0.333333333333333,0.333333333333333,
0.333333333333333,0.333333333333333,0.333333333333333,0.333333333333333,
0.333333333333333,0.333333333333333,0.333333333333333,0.333333333333333,
0.333333333333333,0.333333333333333,0.333333333333333,0.333333333333333,
0.333333333333333,0.333333333333333,0.333333333333333,0.333333333333333,
0.333333333333333,0.333333333333333,0.333333333333333,0.333333333333333,
0.333333333333333,0.333333333333333,0.333333333333333,0.333333333333333,
0.333333333333333,0.333333333333333,0.333333333333333,0.333333333333333,
0.333333333333333,0.333333333333333,0.333333333333333,0.333333333333333,
0.333333333333333,0.333333333333333,0.333333333333333,0.333333333333333,
0.333333333333333,0.333333333333333,0.333333333333333,0.333333333333333,
0.333333333333333),(1.,1.,1.,1.,1.,1.,1.,1.,1.,1.,1.,1.,1.,1.,1.,1.,1.,
1.,1.,1.,1.,1.,1.,1.,1.,1.,1.,1.,1.,1.,1.,1.,1.,1.,1.,1.,1.,1.,1.,1.,1.,
1.,1.,1.,1.,1.,1.,1.,1.,1.,1.,1.,1.,1.,1.,1.,1.,1.,1.,1.,1.,1.,1.,1.,1.,
1.,1.,1.,1.,1.,1.,1.,1.,1.,1.,1.,1.,1.,1.,1.,1.,1.,1.,1.,1.,1.,1.,1.,1.,
1.,1.,1.,1.,1.,1.,1.,1.,1.,1.,1.,1.,1.,1.,1.,1.,1.,1.,1.,1.,1.,1.,1.,1.,
1.,1.,1.,1.,1.,1.,1.,1.,1.,1.,1.,1.,1.,1.,1.,1.,1.,1.,1.,1.,1.,1.,1.,1.,
1.,1.,1.,1.,1.,1.,1.,1.,1.,1.,1.,1.,1.,1.,1.,1.,1.,1.,1.,1.,1.,1.,1.,1.,
1.,1.,1.,1.,1.,1.,1.)))
REPRESENTATION_ITEM('')
SURFACE()
);
#531=(
BOUNDED_SURFACE()
B_SPLINE_SURFACE(3,3,((#15532,#15533,#15534,#15535,#15536,#15537,#15538,
#15539,#15540,#15541,#15542,#15543,#15544,#15545,#15546,#15547,#15548,#15549,
#15550,#15551),(#15552,#15553,#15554,#15555,#15556,#15557,#15558,#15559,
#15560,#15561,#15562,#15563,#15564,#15565,#15566,#15567,#15568,#15569,#15570,
#15571),(#15572,#15573,#15574,#15575,#15576,#15577,#15578,#15579,#15580,
#15581,#15582,#15583,#15584,#15585,#15586,#15587,#15588,#15589,#15590,#15591),
(#15592,#15593,#15594,#15595,#15596,#15597,#15598,#15599,#15600,#15601,
#15602,#15603,#15604,#15605,#15606,#15607,#15608,#15609,#15610,#15611),
(#15612,#15613,#15614,#15615,#15616,#15617,#15618,#15619,#15620,#15621,
#15622,#15623,#15624,#15625,#15626,#15627,#15628,#15629,#15630,#15631),
(#15632,#15633,#15634,#15635,#15636,#15637,#15638,#15639,#15640,#15641,
#15642,#15643,#15644,#15645,#15646,#15647,#15648,#15649,#15650,#15651),
(#15652,#15653,#15654,#15655,#15656,#15657,#15658,#15659,#15660,#15661,
#15662,#15663,#15664,#15665,#15666,#15667,#15668,#15669,#15670,#15671)),
 .UNSPECIFIED.,.T.,.F.,.F.)
B_SPLINE_SURFACE_WITH_KNOTS((4,3,4),(4,2,2,2,2,2,2,2,2,4),(0.,0.5,1.),(0.0618954463697512,
0.0653601604005303,0.0688248744313094,0.0757543024928677,0.0792190165236468,
0.0809513735390363,0.0826837305544259,0.086148444585205,0.0878808016005946,
0.0896131586159842),.UNSPECIFIED.)
GEOMETRIC_REPRESENTATION_ITEM()
RATIONAL_B_SPLINE_SURFACE(((1.,1.,1.,1.,1.,1.,1.,1.,1.,1.,1.,1.,1.,1.,1.,
1.,1.,1.,1.,1.),(0.333333333333333,0.333333333333333,0.333333333333333,
0.333333333333333,0.333333333333333,0.333333333333333,0.333333333333333,
0.333333333333333,0.333333333333333,0.333333333333333,0.333333333333333,
0.333333333333333,0.333333333333333,0.333333333333333,0.333333333333333,
0.333333333333333,0.333333333333333,0.333333333333333,0.333333333333333,
0.333333333333333),(0.333333333333333,0.333333333333333,0.333333333333333,
0.333333333333333,0.333333333333333,0.333333333333333,0.333333333333333,
0.333333333333333,0.333333333333333,0.333333333333333,0.333333333333333,
0.333333333333333,0.333333333333333,0.333333333333333,0.333333333333333,
0.333333333333333,0.333333333333333,0.333333333333333,0.333333333333333,
0.333333333333333),(1.,1.,1.,1.,1.,1.,1.,1.,1.,1.,1.,1.,1.,1.,1.,1.,1.,
1.,1.,1.),(0.333333333333333,0.333333333333333,0.333333333333333,0.333333333333333,
0.333333333333333,0.333333333333333,0.333333333333333,0.333333333333333,
0.333333333333333,0.333333333333333,0.333333333333333,0.333333333333333,
0.333333333333333,0.333333333333333,0.333333333333333,0.333333333333333,
0.333333333333333,0.333333333333333,0.333333333333333,0.333333333333333),
(0.333333333333333,0.333333333333333,0.333333333333333,0.333333333333333,
0.333333333333333,0.333333333333333,0.333333333333333,0.333333333333333,
0.333333333333333,0.333333333333333,0.333333333333333,0.333333333333333,
0.333333333333333,0.333333333333333,0.333333333333333,0.333333333333333,
0.333333333333333,0.333333333333333,0.333333333333333,0.333333333333333),
(1.,1.,1.,1.,1.,1.,1.,1.,1.,1.,1.,1.,1.,1.,1.,1.,1.,1.,1.,1.)))
REPRESENTATION_ITEM('')
SURFACE()
);
#532=(
BOUNDED_SURFACE()
B_SPLINE_SURFACE(3,2,((#17291,#17292,#17293),(#17294,#17295,#17296),(#17297,
#17298,#17299),(#17300,#17301,#17302)),.UNSPECIFIED.,.F.,.F.,.F.)
B_SPLINE_SURFACE_WITH_KNOTS((4,4),(3,3),(0.0596721496079926,0.060305624008707),
(0.0470793423724159,1.),.UNSPECIFIED.)
GEOMETRIC_REPRESENTATION_ITEM()
RATIONAL_B_SPLINE_SURFACE(((0.973719934576668,0.720896001313625,1.),(0.973719934576668,
0.720896001313625,1.),(0.973719934576668,0.720896001313625,1.),(0.973719934576668,
0.720896001313625,1.)))
REPRESENTATION_ITEM('')
SURFACE()
);
#533=(
BOUNDED_SURFACE()
B_SPLINE_SURFACE(3,2,((#17337,#17338,#17339),(#17340,#17341,#17342),(#17343,
#17344,#17345),(#17346,#17347,#17348)),.UNSPECIFIED.,.F.,.F.,.F.)
B_SPLINE_SURFACE_WITH_KNOTS((4,4),(3,3),(0.0581736933140078,0.0588009183988192),
(0.0549949072393295,1.),.UNSPECIFIED.)
GEOMETRIC_REPRESENTATION_ITEM()
RATIONAL_B_SPLINE_SURFACE(((0.969556405029951,0.723214416586222,1.),(0.969556405029951,
0.723214416586222,1.),(0.969556405029951,0.723214416586222,1.),(0.969556405029951,
0.723214416586222,1.)))
REPRESENTATION_ITEM('')
SURFACE()
);
#534=(
BOUNDED_SURFACE()
B_SPLINE_SURFACE(3,2,((#17383,#17384,#17385),(#17386,#17387,#17388),(#17389,
#17390,#17391),(#17392,#17393,#17394)),.UNSPECIFIED.,.F.,.F.,.F.)
B_SPLINE_SURFACE_WITH_KNOTS((4,4),(3,3),(0.0566744883899997,0.0572968072375656),
(0.0615688709473457,1.),.UNSPECIFIED.)
GEOMETRIC_REPRESENTATION_ITEM()
RATIONAL_B_SPLINE_SURFACE(((0.966154346222294,0.725139885977026,1.),(0.966154346222294,
0.725139885977026,1.),(0.966154346222294,0.725139885977026,1.),(0.966154346222294,
0.725139885977026,1.)))
REPRESENTATION_ITEM('')
SURFACE()
);
#535=(
BOUNDED_SURFACE()
B_SPLINE_SURFACE(3,2,((#17427,#17428,#17429),(#17430,#17431,#17432),(#17433,
#17434,#17435),(#17436,#17437,#17438)),.UNSPECIFIED.,.F.,.F.,.F.)
B_SPLINE_SURFACE_WITH_KNOTS((4,4),(3,3),(0.0551745403883536,0.0557932703572333),
(0.066777420683245,1.),.UNSPECIFIED.)
GEOMETRIC_REPRESENTATION_ITEM()
RATIONAL_B_SPLINE_SURFACE(((0.963494845514688,0.726665434874523,1.),(0.963494845514688,
0.726665434874523,1.),(0.963494845514688,0.726665434874523,1.),(0.963494845514688,
0.726665434874523,1.)))
REPRESENTATION_ITEM('')
SURFACE()
);
#536=(
BOUNDED_SURFACE()
B_SPLINE_SURFACE(3,2,((#17471,#17472,#17473),(#17474,#17475,#17476),(#17477,
#17478,#17479),(#17480,#17481,#17482)),.UNSPECIFIED.,.F.,.F.,.F.)
B_SPLINE_SURFACE_WITH_KNOTS((4,4),(3,3),(0.0536738567287748,0.0542902895645969),
(0.0706052509682322,1.),.UNSPECIFIED.)
GEOMETRIC_REPRESENTATION_ITEM()
RATIONAL_B_SPLINE_SURFACE(((0.961560606385539,0.727786580407766,1.),(0.961560606385539,
0.727786580407766,1.),(0.961560606385539,0.727786580407765,1.),(0.961560606385539,
0.727786580407765,1.)))
REPRESENTATION_ITEM('')
SURFACE()
);
#537=(
BOUNDED_SURFACE()
B_SPLINE_SURFACE(3,2,((#17515,#17516,#17517),(#17518,#17519,#17520),(#17521,
#17522,#17523),(#17524,#17525,#17526)),.UNSPECIFIED.,.F.,.F.,.F.)
B_SPLINE_SURFACE_WITH_KNOTS((4,4),(3,3),(0.0521724469311448,0.0527878485478844),
(0.073047320944285,1.),.UNSPECIFIED.)
GEOMETRIC_REPRESENTATION_ITEM()
RATIONAL_B_SPLINE_SURFACE(((0.960335574438944,0.728501846143617,1.),(0.960335574438944,
0.728501846143617,1.),(0.960335574438944,0.728501846143619,1.),(0.960335574438944,
0.728501846143619,1.)))
REPRESENTATION_ITEM('')
SURFACE()
);
#538=(
BOUNDED_SURFACE()
B_SPLINE_SURFACE(3,2,((#17557,#17558,#17559),(#17560,#17561,#17562),(#17563,
#17564,#17565),(#17566,#17567,#17568)),.UNSPECIFIED.,.F.,.F.,.F.)
B_SPLINE_SURFACE_WITH_KNOTS((4,4),(3,3),(0.15547618557744,0.156093772145324),
(0.073524259555501,1.),.UNSPECIFIED.)
GEOMETRIC_REPRESENTATION_ITEM()
RATIONAL_B_SPLINE_SURFACE(((0.960097140048281,0.728641538228635,1.),(0.960097140048281,
0.728641538228635,1.),(0.960097140048281,0.728641538228634,1.),(0.960097140048281,
0.728641538228634,1.)))
REPRESENTATION_ITEM('')
SURFACE()
);
#539=(
BOUNDED_SURFACE()
B_SPLINE_SURFACE(3,2,((#17602,#17603,#17604),(#17605,#17606,#17607),(#17608,
#17609,#17610),(#17611,#17612,#17613)),.UNSPECIFIED.,.F.,.F.,.F.)
B_SPLINE_SURFACE_WITH_KNOTS((4,4),(3,3),(0.153971233644507,0.154591580945739),
(0.0715119122999407,1.),.UNSPECIFIED.)
GEOMETRIC_REPRESENTATION_ITEM()
RATIONAL_B_SPLINE_SURFACE(((0.961104976307929,0.728052135363584,1.),(0.961104976307929,
0.728052135363584,1.),(0.961104976307929,0.728052135363584,1.),(0.961104976307929,
0.728052135363584,1.)))
REPRESENTATION_ITEM('')
SURFACE()
);
#540=(
BOUNDED_SURFACE()
B_SPLINE_SURFACE(3,2,((#17647,#17648,#17649),(#17650,#17651,#17652),(#17653,
#17654,#17655),(#17656,#17657,#17658)),.UNSPECIFIED.,.F.,.F.,.F.)
B_SPLINE_SURFACE_WITH_KNOTS((4,4),(3,3),(0.152465422311365,0.153089822150018),
(0.0681150405736641,1.),.UNSPECIFIED.)
GEOMETRIC_REPRESENTATION_ITEM()
RATIONAL_B_SPLINE_SURFACE(((0.962816982205886,0.727057214669775,1.),(0.962816982205886,
0.727057214669775,1.),(0.962816982205886,0.727057214669777,1.),(0.962816982205886,
0.727057214669777,1.)))
REPRESENTATION_ITEM('')
SURFACE()
);
#541=(
BOUNDED_SURFACE()
B_SPLINE_SURFACE(3,2,((#17694,#17695,#17696),(#17697,#17698,#17699),(#17700,
#17701,#17702),(#17703,#17704,#17705)),.UNSPECIFIED.,.F.,.F.,.F.)
B_SPLINE_SURFACE_WITH_KNOTS((4,4),(3,3),(0.150958741315287,0.151588591705843),
(0.0633354277393988,1.),.UNSPECIFIED.)
GEOMETRIC_REPRESENTATION_ITEM()
RATIONAL_B_SPLINE_SURFACE(((0.965248775304359,0.725657298482067,1.),(0.965248775304359,
0.725657298482067,1.),(0.965248775304359,0.725657298482067,1.),(0.965248775304359,
0.725657298482067,1.)))
REPRESENTATION_ITEM('')
SURFACE()
);
#542=(
BOUNDED_SURFACE()
B_SPLINE_SURFACE(3,2,((#17743,#17744,#17745),(#17746,#17747,#17748),(#17749,
#17750,#17751),(#17752,#17753,#17754)),.UNSPECIFIED.,.F.,.F.,.F.)
B_SPLINE_SURFACE_WITH_KNOTS((4,4),(3,3),(0.149451183265075,0.150087942103155),
(0.0571854695619357,1.),.UNSPECIFIED.)
GEOMETRIC_REPRESENTATION_ITEM()
RATIONAL_B_SPLINE_SURFACE(((0.968417153380738,0.723856017435902,1.),(0.968417153380738,
0.723856017435902,1.),(0.968417153380738,0.723856017435903,1.),(0.968417153380738,
0.723856017435903,1.)))
REPRESENTATION_ITEM('')
SURFACE()
);
#543=(
BOUNDED_SURFACE()
B_SPLINE_SURFACE(3,2,((#17792,#17793,#17794),(#17795,#17796,#17797),(#17798,
#17799,#17800),(#17801,#17802,#17803)),.UNSPECIFIED.,.F.,.F.,.F.)
B_SPLINE_SURFACE_WITH_KNOTS((4,4),(3,3),(0.147942744613282,0.148587704815656),
(0.0496865592693353,1.),.UNSPECIFIED.)
GEOMETRIC_REPRESENTATION_ITEM()
RATIONAL_B_SPLINE_SURFACE(((0.972340450159485,0.721659637462709,1.),(0.972340450159485,
0.721659637462709,1.),(0.972340450159485,0.721659637462709,1.),(0.972340450159485,
0.721659637462709,1.)))
REPRESENTATION_ITEM('')
SURFACE()
);
#544=(
BOUNDED_SURFACE()
B_SPLINE_SURFACE(3,2,((#18074,#18075,#18076),(#18077,#18078,#18079),(#18080,
#18081,#18082),(#18083,#18084,#18085),(#18086,#18087,#18088),(#18089,#18090,
#18091),(#18092,#18093,#18094),(#18095,#18096,#18097),(#18098,#18099,#18100),
(#18101,#18102,#18103),(#18104,#18105,#18106),(#18107,#18108,#18109),(#18110,
#18111,#18112),(#18113,#18114,#18115),(#18116,#18117,#18118),(#18119,#18120,
#18121),(#18122,#18123,#18124),(#18125,#18126,#18127),(#18128,#18129,#18130),
(#18131,#18132,#18133),(#18134,#18135,#18136),(#18137,#18138,#18139),(#18140,
#18141,#18142),(#18143,#18144,#18145),(#18146,#18147,#18148),(#18149,#18150,
#18151)),.UNSPECIFIED.,.F.,.F.,.F.)
B_SPLINE_SURFACE_WITH_KNOTS((4,2,2,2,2,2,2,2,2,2,2,2,4),(3,3),(0.0852283172250545,
0.098258593834224,0.111288870443393,0.124319147052563,0.137349423661732,
0.143864561966317,0.150379700270902,0.156894838575487,0.163409976880071,
0.169925115184656,0.176440253489241,0.182955391793825,0.18947053009841),
(0.,1.),.UNSPECIFIED.)
GEOMETRIC_REPRESENTATION_ITEM()
RATIONAL_B_SPLINE_SURFACE(((1.,0.707106781186546,1.),(1.,0.707106781186546,
1.),(1.,0.707106781186546,1.),(1.,0.707106781186546,1.),(1.,0.707106781186548,
1.),(1.,0.707106781186548,1.),(1.,0.707106781186548,1.),(1.,0.707106781186548,
1.),(1.,0.707106781186548,1.),(1.,0.707106781186548,1.),(1.,0.707106781186547,
1.),(1.,0.707106781186547,1.),(1.,0.707106781186548,1.),(1.,0.707106781186548,
1.),(1.,0.707106781186548,1.),(1.,0.707106781186548,1.),(1.,0.707106781186548,
1.),(1.,0.707106781186548,1.),(1.,0.707106781186547,1.),(1.,0.707106781186547,
1.),(1.,0.707106781186548,1.),(1.,0.707106781186548,1.),(1.,0.707106781186548,
1.),(1.,0.707106781186548,1.),(1.,0.707106781186548,1.),(1.,0.707106781186548,
1.)))
REPRESENTATION_ITEM('')
SURFACE()
);
#545=(
BOUNDED_SURFACE()
B_SPLINE_SURFACE(3,2,((#18238,#18239,#18240),(#18241,#18242,#18243),(#18244,
#18245,#18246),(#18247,#18248,#18249),(#18250,#18251,#18252),(#18253,#18254,
#18255),(#18256,#18257,#18258),(#18259,#18260,#18261),(#18262,#18263,#18264),
(#18265,#18266,#18267),(#18268,#18269,#18270),(#18271,#18272,#18273),(#18274,
#18275,#18276),(#18277,#18278,#18279),(#18280,#18281,#18282),(#18283,#18284,
#18285),(#18286,#18287,#18288),(#18289,#18290,#18291),(#18292,#18293,#18294),
(#18295,#18296,#18297),(#18298,#18299,#18300),(#18301,#18302,#18303),(#18304,
#18305,#18306),(#18307,#18308,#18309),(#18310,#18311,#18312),(#18313,#18314,
#18315),(#18316,#18317,#18318),(#18319,#18320,#18321)),.UNSPECIFIED.,.F.,
 .F.,.F.)
B_SPLINE_SURFACE_WITH_KNOTS((4,2,2,2,2,2,2,2,2,2,2,2,2,4),(3,3),(0.0184185986382119,
0.0249387797460936,0.0281988703000345,0.0314589608539753,0.037979141961857,
0.0444993230697387,0.0510195041776203,0.057539685285502,0.0640598663933837,
0.0705800475012654,0.0836204097170287,0.0966607719327921,0.109701134148555,
0.122741496364319),(0.,1.),.UNSPECIFIED.)
GEOMETRIC_REPRESENTATION_ITEM()
RATIONAL_B_SPLINE_SURFACE(((1.,0.707106781186548,1.),(1.,0.707106781186548,
1.),(1.,0.707106781186548,1.),(1.,0.707106781186548,1.),(1.,0.707106781186547,
1.),(1.,0.707106781186547,1.),(1.,0.707106781186548,1.),(1.,0.707106781186548,
1.),(1.,0.707106781186548,1.),(1.,0.707106781186548,1.),(1.,0.707106781186548,
1.),(1.,0.707106781186548,1.),(1.,0.707106781186548,1.),(1.,0.707106781186548,
1.),(1.,0.707106781186547,1.),(1.,0.707106781186547,1.),(1.,0.707106781186548,
1.),(1.,0.707106781186548,1.),(1.,0.707106781186548,1.),(1.,0.707106781186548,
1.),(1.,0.707106781186548,1.),(1.,0.707106781186548,1.),(1.,0.707106781186548,
1.),(1.,0.707106781186548,1.),(1.,0.707106781186548,1.),(1.,0.707106781186548,
1.),(1.,0.707106781186548,1.),(1.,0.707106781186548,1.)))
REPRESENTATION_ITEM('')
SURFACE()
);
#546=(
BOUNDED_SURFACE()
B_SPLINE_SURFACE(3,2,((#18776,#18777,#18778),(#18779,#18780,#18781),(#18782,
#18783,#18784),(#18785,#18786,#18787),(#18788,#18789,#18790),(#18791,#18792,
#18793),(#18794,#18795,#18796),(#18797,#18798,#18799),(#18800,#18801,#18802),
(#18803,#18804,#18805),(#18806,#18807,#18808),(#18809,#18810,#18811),(#18812,
#18813,#18814),(#18815,#18816,#18817),(#18818,#18819,#18820),(#18821,#18822,
#18823),(#18824,#18825,#18826),(#18827,#18828,#18829),(#18830,#18831,#18832),
(#18833,#18834,#18835),(#18836,#18837,#18838),(#18839,#18840,#18841),(#18842,
#18843,#18844),(#18845,#18846,#18847),(#18848,#18849,#18850),(#18851,#18852,
#18853),(#18854,#18855,#18856),(#18857,#18858,#18859),(#18860,#18861,#18862),
(#18863,#18864,#18865),(#18866,#18867,#18868),(#18869,#18870,#18871)),
 .UNSPECIFIED.,.F.,.F.,.F.)
B_SPLINE_SURFACE_WITH_KNOTS((4,2,2,2,2,2,2,2,2,2,2,2,2,2,2,4),(3,3),(0.0508378190163745,
0.0688435419383206,0.0868492648602666,0.104854987782213,0.122860710704159,
0.131863572165132,0.140866433626105,0.149869295087078,0.158872156548051,
0.167875018009024,0.176877879469997,0.18588074093097,0.190382171661456,
0.1926328870267,0.193758244709321,0.194883602391943),(0.,1.),
 .UNSPECIFIED.)
GEOMETRIC_REPRESENTATION_ITEM()
RATIONAL_B_SPLINE_SURFACE(((1.,0.707106781186548,1.),(1.,0.707106781186548,
1.),(1.,0.707106781186545,1.),(1.,0.707106781186545,1.),(1.,0.707106781186548,
1.),(1.,0.707106781186548,1.),(1.,0.707106781186548,1.),(1.,0.707106781186548,
1.),(1.,0.707106781186548,1.),(1.,0.707106781186548,1.),(1.,0.707106781186548,
1.),(1.,0.707106781186548,1.),(1.,0.707106781186548,1.),(1.,0.707106781186548,
1.),(1.,0.707106781186548,1.),(1.,0.707106781186548,1.),(1.,0.707106781186548,
1.),(1.,0.707106781186548,1.),(1.,0.707106781186548,1.),(1.,0.707106781186548,
1.),(1.,0.707106781186548,1.),(1.,0.707106781186548,1.),(1.,0.707106781186548,
1.),(1.,0.707106781186548,1.),(1.,0.707106781186547,1.),(1.,0.707106781186547,
1.),(1.,0.707106781186548,1.),(1.,0.707106781186548,1.),(1.,0.707106781186548,
1.),(1.,0.707106781186548,1.),(1.,0.707106781186548,1.),(1.,0.707106781186548,
1.)))
REPRESENTATION_ITEM('')
SURFACE()
);
#547=(
BOUNDED_SURFACE()
B_SPLINE_SURFACE(3,2,((#18939,#18940,#18941),(#18942,#18943,#18944),(#18945,
#18946,#18947),(#18948,#18949,#18950),(#18951,#18952,#18953),(#18954,#18955,
#18956),(#18957,#18958,#18959),(#18960,#18961,#18962),(#18963,#18964,#18965),
(#18966,#18967,#18968),(#18969,#18970,#18971),(#18972,#18973,#18974),(#18975,
#18976,#18977),(#18978,#18979,#18980),(#18981,#18982,#18983),(#18984,#18985,
#18986),(#18987,#18988,#18989),(#18990,#18991,#18992),(#18993,#18994,#18995),
(#18996,#18997,#18998),(#18999,#19000,#19001),(#19002,#19003,#19004),(#19005,
#19006,#19007),(#19008,#19009,#19010),(#19011,#19012,#19013),(#19014,#19015,
#19016),(#19017,#19018,#19019),(#19020,#19021,#19022),(#19023,#19024,#19025),
(#19026,#19027,#19028),(#19029,#19030,#19031),(#19032,#19033,#19034),(#19035,
#19036,#19037),(#19038,#19039,#19040),(#19041,#19042,#19043),(#19044,#19045,
#19046)),.UNSPECIFIED.,.F.,.F.,.F.)
B_SPLINE_SURFACE_WITH_KNOTS((4,2,2,2,2,2,2,2,2,2,2,2,2,2,2,2,2,4),(3,3),
(0.0129986978937602,0.0141248636966938,0.0152510294996274,0.0175033611054947,
0.0220080243172292,0.0265126875289637,0.0310173507406982,0.0400266771641672,
0.0490360035876362,0.0580453300111053,0.0670546564345743,0.0760639828580433,
0.0850733092815123,0.10309196212845,0.121110614975388,0.130119941398857,
0.139129267822326,0.157147920669264),(0.,1.),.UNSPECIFIED.)
GEOMETRIC_REPRESENTATION_ITEM()
RATIONAL_B_SPLINE_SURFACE(((1.,0.707106781186547,1.),(1.,0.707106781186547,
1.),(1.,0.707106781186548,1.),(1.,0.707106781186548,1.),(1.,0.707106781186548,
1.),(1.,0.707106781186548,1.),(1.,0.707106781186548,1.),(1.,0.707106781186548,
1.),(1.,0.707106781186548,1.),(1.,0.707106781186548,1.),(1.,0.707106781186548,
1.),(1.,0.707106781186548,1.),(1.,0.707106781186548,1.),(1.,0.707106781186548,
1.),(1.,0.707106781186548,1.),(1.,0.707106781186548,1.),(1.,0.707106781186548,
1.),(1.,0.707106781186548,1.),(1.,0.707106781186548,1.),(1.,0.707106781186548,
1.),(1.,0.707106781186548,1.),(1.,0.707106781186548,1.),(1.,0.707106781186548,
1.),(1.,0.707106781186548,1.),(1.,0.707106781186548,1.),(1.,0.707106781186548,
1.),(1.,0.707106781186548,1.),(1.,0.707106781186548,1.),(1.,0.707106781186549,
1.),(1.,0.707106781186549,1.),(1.,0.70710678118655,1.),(1.,0.70710678118655,
1.),(1.,0.707106781186551,1.),(1.,0.707106781186551,1.),(1.,0.707106781186548,
1.),(1.,0.707106781186548,1.)))
REPRESENTATION_ITEM('')
SURFACE()
);
#548=(
BOUNDED_SURFACE()
B_SPLINE_SURFACE(3,2,((#19271,#19272,#19273),(#19274,#19275,#19276),(#19277,
#19278,#19279),(#19280,#19281,#19282)),.UNSPECIFIED.,.F.,.F.,.F.)
B_SPLINE_SURFACE_WITH_KNOTS((4,4),(3,3),(0.0508378190163745,0.0512849497020778),
(0.0741100254049076,1.),.UNSPECIFIED.)
GEOMETRIC_REPRESENTATION_ITEM()
RATIONAL_B_SPLINE_SURFACE(((0.959804664655073,0.728813105073738,1.),(0.959804664655073,
0.728813105073738,1.),(0.959804664655073,0.728813105073736,1.),(0.959804664655073,
0.728813105073736,1.)))
REPRESENTATION_ITEM('')
SURFACE()
);
#549=(
BOUNDED_SURFACE()
B_SPLINE_SURFACE(3,2,((#19857,#19858,#19859),(#19860,#19861,#19862),(#19863,
#19864,#19865),(#19866,#19867,#19868)),.UNSPECIFIED.,.F.,.F.,.F.)
B_SPLINE_SURFACE_WITH_KNOTS((4,4),(3,3),(1.47451495458029E-17,6.21085125745449E-5),
(0.,1.),.UNSPECIFIED.)
GEOMETRIC_REPRESENTATION_ITEM()
RATIONAL_B_SPLINE_SURFACE(((1.,0.707106781186542,1.),(1.,0.710100066656328,
1.),(1.,0.713076333427087,1.),(1.,0.716036186282139,1.)))
REPRESENTATION_ITEM('')
SURFACE()
);
#550=(
BOUNDED_SURFACE()
B_SPLINE_SURFACE(3,2,((#19870,#19871,#19872),(#19873,#19874,#19875),(#19876,
#19877,#19878),(#19879,#19880,#19881),(#19882,#19883,#19884),(#19885,#19886,
#19887),(#19888,#19889,#19890),(#19891,#19892,#19893)),.UNSPECIFIED.,.F.,
 .F.,.F.)
B_SPLINE_SURFACE_WITH_KNOTS((4,2,2,4),(3,3),(0.00527160002528868,0.00580803552825251,
0.00634447103121634,0.00741734203714401),(0.,1.),.UNSPECIFIED.)
GEOMETRIC_REPRESENTATION_ITEM()
RATIONAL_B_SPLINE_SURFACE(((1.,0.951613498173813,1.),(1.,0.937509881703587,
1.),(1.,0.921891319389384,1.),(1.,0.887932805313032,1.),(1.,0.869471948377235,
1.),(1.,0.810569928220315,1.),(1.,0.766682605321705,1.),(1.,0.716036186282147,
1.)))
REPRESENTATION_ITEM('')
SURFACE()
);
#551=(
BOUNDED_SURFACE()
B_SPLINE_SURFACE(3,2,((#19895,#19896,#19897),(#19898,#19899,#19900),(#19901,
#19902,#19903),(#19904,#19905,#19906),(#19907,#19908,#19909),(#19910,#19911,
#19912)),.UNSPECIFIED.,.F.,.F.,.F.)
B_SPLINE_SURFACE_WITH_KNOTS((4,2,4),(3,3),(-2.60208521396521E-17,0.00181589083224653,
0.00363178166449308),(0.,1.),.UNSPECIFIED.)
GEOMETRIC_REPRESENTATION_ITEM()
RATIONAL_B_SPLINE_SURFACE(((1.,0.951613498173813,1.),(1.,0.954339600494346,
1.),(1.,0.956942012490788,1.),(1.,0.961426637855616,1.),(1.,0.963309297483902,
1.),(1.,0.964515574250421,1.)))
REPRESENTATION_ITEM('')
SURFACE()
);
#552=(
BOUNDED_SURFACE()
B_SPLINE_SURFACE(3,2,((#19913,#19914,#19915),(#19916,#19917,#19918),(#19919,
#19920,#19921),(#19922,#19923,#19924)),.UNSPECIFIED.,.F.,.F.,.F.)
B_SPLINE_SURFACE_WITH_KNOTS((4,4),(3,3),(1.24954300378954E-17,6.21085125745808E-5),
(0.,1.),.UNSPECIFIED.)
GEOMETRIC_REPRESENTATION_ITEM()
RATIONAL_B_SPLINE_SURFACE(((1.,0.707106781186542,1.),(1.,0.710100066656337,
1.),(1.,0.713076333427082,1.),(1.,0.716036186282145,1.)))
REPRESENTATION_ITEM('')
SURFACE()
);
#553=(
BOUNDED_SURFACE()
B_SPLINE_SURFACE(3,2,((#19926,#19927,#19928),(#19929,#19930,#19931),(#19932,
#19933,#19934),(#19935,#19936,#19937),(#19938,#19939,#19940),(#19941,#19942,
#19943),(#19944,#19945,#19946),(#19947,#19948,#19949)),.UNSPECIFIED.,.F.,
 .F.,.F.)
B_SPLINE_SURFACE_WITH_KNOTS((4,2,2,4),(3,3),(0.00527160002528845,0.00580803552825226,
0.00634447103121607,0.00741734203714369),(0.,1.),.UNSPECIFIED.)
GEOMETRIC_REPRESENTATION_ITEM()
RATIONAL_B_SPLINE_SURFACE(((1.,0.951613498173813,1.),(1.,0.937509881703887,
1.),(1.,0.921891319388982,1.),(1.,0.887932805313441,1.),(1.,0.869471948377343,
1.),(1.,0.810569928220099,1.),(1.,0.766682605321886,1.),(1.,0.716036186282151,
1.)))
REPRESENTATION_ITEM('')
SURFACE()
);
#554=(
BOUNDED_SURFACE()
B_SPLINE_SURFACE(3,2,((#19951,#19952,#19953),(#19954,#19955,#19956),(#19957,
#19958,#19959),(#19960,#19961,#19962),(#19963,#19964,#19965),(#19966,#19967,
#19968)),.UNSPECIFIED.,.F.,.F.,.F.)
B_SPLINE_SURFACE_WITH_KNOTS((4,2,4),(3,3),(-8.67361737988404E-18,0.00181589083224649,
0.00363178166449298),(0.,1.),.UNSPECIFIED.)
GEOMETRIC_REPRESENTATION_ITEM()
RATIONAL_B_SPLINE_SURFACE(((1.,0.951613498173814,1.),(1.,0.954339600494444,
1.),(1.,0.956942012490655,1.),(1.,0.961426637855752,1.),(1.,0.963309297483799,
1.),(1.,0.96451557425042,1.)))
REPRESENTATION_ITEM('')
SURFACE()
);
#555=(
BOUNDED_SURFACE()
B_SPLINE_SURFACE(3,2,((#20003,#20004,#20005),(#20006,#20007,#20008),(#20009,
#20010,#20011),(#20012,#20013,#20014),(#20015,#20016,#20017),(#20018,#20019,
#20020),(#20021,#20022,#20023),(#20024,#20025,#20026),(#20027,#20028,#20029),
(#20030,#20031,#20032),(#20033,#20034,#20035),(#20036,#20037,#20038),(#20039,
#20040,#20041),(#20042,#20043,#20044),(#20045,#20046,#20047),(#20048,#20049,
#20050)),.UNSPECIFIED.,.F.,.F.,.F.)
B_SPLINE_SURFACE_WITH_KNOTS((4,2,2,2,2,2,2,4),(3,3),(-9.54097911787244E-18,
0.000696349442505511,0.00139269888501103,0.00208904832751655,0.00278539777002207,
0.00348174721252759,0.00417809665503312,0.00557079554004416),(0.,1.),
 .UNSPECIFIED.)
GEOMETRIC_REPRESENTATION_ITEM()
RATIONAL_B_SPLINE_SURFACE(((1.,0.607054112111757,1.),(1.,0.607056484530443,
1.),(1.,0.607765985148788,1.),(1.,0.610539233834522,1.),(1.,0.612638008520617,
1.),(1.,0.618035047876937,1.),(1.,0.621317782228222,1.),(1.,0.628996523516187,
1.),(1.,0.633392405889998,1.),(1.,0.642875366219237,1.),(1.,0.648018732602713,
1.),(1.,0.658994978794232,1.),(1.,0.664685207841264,1.),(1.,0.682298653549566,
1.),(1.,0.69487665462171,1.),(1.,0.707106781186348,1.)))
REPRESENTATION_ITEM('')
SURFACE()
);
#556=(
BOUNDED_SURFACE()
B_SPLINE_SURFACE(3,2,((#20054,#20055,#20056),(#20057,#20058,#20059),(#20060,
#20061,#20062),(#20063,#20064,#20065),(#20066,#20067,#20068),(#20069,#20070,
#20071),(#20072,#20073,#20074),(#20075,#20076,#20077),(#20078,#20079,#20080),
(#20081,#20082,#20083),(#20084,#20085,#20086),(#20087,#20088,#20089),(#20090,
#20091,#20092),(#20093,#20094,#20095),(#20096,#20097,#20098),(#20099,#20100,
#20101),(#20102,#20103,#20104),(#20105,#20106,#20107)),.UNSPECIFIED.,.F.,
 .F.,.F.)
B_SPLINE_SURFACE_WITH_KNOTS((4,2,2,2,2,2,2,2,4),(3,3),(4.55364912443912E-18,
0.000696359701744999,0.00139271940348999,0.00208907910523499,0.00278543880697998,
0.00348179850872497,0.00417815821046997,0.00487451791221496,0.00557087761395996),
(0.,1.),.UNSPECIFIED.)
GEOMETRIC_REPRESENTATION_ITEM()
RATIONAL_B_SPLINE_SURFACE(((1.,0.707106781186528,1.),(1.,0.700938621263621,
1.),(1.,0.694814107318537,1.),(1.,0.682647727308077,1.),(1.,0.676551634194648,
1.),(1.,0.664717932169144,1.),(1.,0.659039302098822,1.),(1.,0.648178638212686,
1.),(1.,0.642945691912101,1.),(1.,0.633426835507387,1.),(1.,0.629110758092159,
1.),(1.,0.621426182814592,1.),(1.,0.618064223074675,1.),(1.,0.612677785681965,
1.),(1.,0.61060178483004,1.),(1.,0.607773091248028,1.),(1.,0.607052269837757,
1.),(1.,0.607054112111752,1.)))
REPRESENTATION_ITEM('')
SURFACE()
);
#557=(
BOUNDED_SURFACE()
B_SPLINE_SURFACE(1,2,((#20118,#20119,#20120,#20121,#20122,#20123,#20124,
#20125,#20126,#20127,#20128,#20129,#20130,#20131,#20132,#20133,#20134,#20135,
#20136,#20137,#20138,#20139,#20140,#20141,#20142,#20143,#20144,#20145,#20146,
#20147,#20148,#20149,#20150,#20151,#20152,#20153,#20154,#20155,#20156,#20157,
#20158,#20159,#20160,#20161,#20162,#20163,#20164,#20165,#20166,#20167,#20168,
#20169,#20170,#20171,#20172,#20173,#20174,#20175,#20176,#20177,#20178,#20179,
#20180,#20181,#20182,#20183,#20184,#20185,#20186,#20187,#20188,#20189,#20190,
#20191,#20192,#20193,#20194,#20195,#20196,#20197,#20198,#20199,#20200,#20201,
#20202,#20203,#20204,#20205,#20206,#20207,#20208,#20209,#20210,#20211,#20212,
#20213,#20214,#20215,#20216,#20217,#20218,#20219,#20220,#20221,#20222,#20223,
#20224,#20225,#20226,#20227,#20228,#20229,#20230,#20231,#20232,#20233,#20234,
#20235,#20236,#20237,#20238,#20239,#20240,#20241,#20242,#20243,#20244,#20245,
#20246,#20247,#20248,#20249,#20250,#20251,#20252,#20253,#20254,#20255,#20256,
#20257,#20258,#20259,#20260,#20261,#20262,#20263,#20264,#20265,#20266,#20267,
#20268,#20269,#20270,#20271,#20272,#20273,#20274,#20275,#20276,#20277,#20278),
(#20279,#20280,#20281,#20282,#20283,#20284,#20285,#20286,#20287,#20288,
#20289,#20290,#20291,#20292,#20293,#20294,#20295,#20296,#20297,#20298,#20299,
#20300,#20301,#20302,#20303,#20304,#20305,#20306,#20307,#20308,#20309,#20310,
#20311,#20312,#20313,#20314,#20315,#20316,#20317,#20318,#20319,#20320,#20321,
#20322,#20323,#20324,#20325,#20326,#20327,#20328,#20329,#20330,#20331,#20332,
#20333,#20334,#20335,#20336,#20337,#20338,#20339,#20340,#20341,#20342,#20343,
#20344,#20345,#20346,#20347,#20348,#20349,#20350,#20351,#20352,#20353,#20354,
#20355,#20356,#20357,#20358,#20359,#20360,#20361,#20362,#20363,#20364,#20365,
#20366,#20367,#20368,#20369,#20370,#20371,#20372,#20373,#20374,#20375,#20376,
#20377,#20378,#20379,#20380,#20381,#20382,#20383,#20384,#20385,#20386,#20387,
#20388,#20389,#20390,#20391,#20392,#20393,#20394,#20395,#20396,#20397,#20398,
#20399,#20400,#20401,#20402,#20403,#20404,#20405,#20406,#20407,#20408,#20409,
#20410,#20411,#20412,#20413,#20414,#20415,#20416,#20417,#20418,#20419,#20420,
#20421,#20422,#20423,#20424,#20425,#20426,#20427,#20428,#20429,#20430,#20431,
#20432,#20433,#20434,#20435,#20436,#20437,#20438,#20439)),.UNSPECIFIED.,
 .F.,.F.,.F.)
B_SPLINE_SURFACE_WITH_KNOTS((2,2),(3,2,2,2,2,2,2,2,2,2,2,2,2,2,2,2,2,2,
2,2,2,2,2,2,2,2,2,2,2,2,2,2,2,2,2,2,2,2,2,2,2,2,2,2,2,2,2,2,2,2,2,2,2,2,
2,2,2,2,2,2,2,2,2,2,2,2,2,2,2,2,2,2,2,2,2,2,2,2,2,2,3),(0.,1.),(0.,0.0125,
0.025,0.0375,0.05,0.0625,0.075,0.0875,0.1,0.1125,0.125,0.1375,0.15,0.1625,
0.175,0.1875,0.2,0.2125,0.225,0.2375,0.25,0.2625,0.275,0.2875,0.3,0.3125,
0.325,0.3375,0.35,0.3625,0.375,0.3875,0.4,0.4125,0.425,0.4375,0.45,0.4625,
0.475,0.4875,0.5,0.5125,0.525,0.5375,0.55,0.5625,0.575,0.5875,0.6,0.6125,
0.625,0.6375,0.65,0.6625,0.675,0.6875,0.7,0.7125,0.725,0.7375,0.75,0.7625,
0.775,0.7875,0.8,0.8125,0.825,0.8375,0.85,0.8625,0.875,0.8875,0.9,0.9125,
0.925,0.9375,0.95,0.9625,0.975,0.9875,1.),.UNSPECIFIED.)
GEOMETRIC_REPRESENTATION_ITEM()
RATIONAL_B_SPLINE_SURFACE(((1.,0.923879532511287,1.,0.923879532511287,1.,
0.923879532511287,1.,0.923879532511287,1.,0.923879532511287,1.,0.923879532511287,
1.,0.923879532511287,1.,0.923879532511287,1.,0.923879532511287,1.,0.923879532511287,
1.,0.923879532511287,1.,0.923879532511287,1.,0.923879532511287,1.,0.923879532511287,
1.,0.923879532511287,1.,0.923879532511287,1.,0.923879532511287,1.,0.923879532511287,
1.,0.923879532511287,1.,0.923879532511287,1.,0.923879532511287,1.,0.923879532511287,
1.,0.923879532511287,1.,0.923879532511287,1.,0.923879532511287,1.,0.923879532511287,
1.,0.923879532511287,1.,0.923879532511287,1.,0.923879532511287,1.,0.923879532511287,
1.,0.923879532511287,1.,0.923879532511287,1.,0.923879532511287,1.,0.923879532511287,
1.,0.923879532511287,1.,0.923879532511287,1.,0.923879532511287,1.,0.923879532511287,
1.,0.923879532511287,1.,0.923879532511287,1.,0.923879532511287,1.,0.923879532511287,
1.,0.923879532511287,1.,0.923879532511287,1.,0.923879532511287,1.,0.923879532511287,
1.,0.923879532511287,1.,0.923879532511287,1.,0.923879532511287,1.,0.923879532511287,
1.,0.923879532511287,1.,0.923879532511287,1.,0.923879532511287,1.,0.923879532511287,
1.,0.923879532511287,1.,0.923879532511287,1.,0.923879532511287,1.,0.923879532511287,
1.,0.923879532511287,1.,0.923879532511287,1.,0.923879532511287,1.,0.923879532511287,
1.,0.923879532511287,1.,0.923879532511287,1.,0.923879532511287,1.,0.923879532511287,
1.,0.923879532511287,1.,0.923879532511287,1.,0.923879532511287,1.,0.923879532511287,
1.,0.923879532511287,1.,0.923879532511287,1.,0.923879532511287,1.,0.923879532511287,
1.,0.923879532511287,1.,0.923879532511287,1.,0.923879532511287,1.,0.923879532511287,
1.,0.923879532511287,1.,0.923879532511287,1.),(1.,0.923879532511287,1.,
0.923879532511287,1.,0.923879532511287,1.,0.923879532511287,1.,0.923879532511287,
1.,0.923879532511287,1.,0.923879532511287,1.,0.923879532511287,1.,0.923879532511287,
1.,0.923879532511287,1.,0.923879532511287,1.,0.923879532511287,1.,0.923879532511287,
1.,0.923879532511287,1.,0.923879532511287,1.,0.923879532511287,1.,0.923879532511287,
1.,0.923879532511287,1.,0.923879532511287,1.,0.923879532511287,1.,0.923879532511287,
1.,0.923879532511287,1.,0.923879532511287,1.,0.923879532511287,1.,0.923879532511287,
1.,0.923879532511287,1.,0.923879532511287,1.,0.923879532511287,1.,0.923879532511287,
1.,0.923879532511287,1.,0.923879532511287,1.,0.923879532511287,1.,0.923879532511287,
1.,0.923879532511287,1.,0.923879532511287,1.,0.923879532511287,1.,0.923879532511287,
1.,0.923879532511287,1.,0.923879532511287,1.,0.923879532511287,1.,0.923879532511287,
1.,0.923879532511287,1.,0.923879532511287,1.,0.923879532511287,1.,0.923879532511287,
1.,0.923879532511287,1.,0.923879532511287,1.,0.923879532511287,1.,0.923879532511287,
1.,0.923879532511287,1.,0.923879532511287,1.,0.923879532511287,1.,0.923879532511287,
1.,0.923879532511287,1.,0.923879532511287,1.,0.923879532511287,1.,0.923879532511287,
1.,0.923879532511287,1.,0.923879532511287,1.,0.923879532511287,1.,0.923879532511287,
1.,0.923879532511287,1.,0.923879532511287,1.,0.923879532511287,1.,0.923879532511287,
1.,0.923879532511287,1.,0.923879532511287,1.,0.923879532511287,1.,0.923879532511287,
1.,0.923879532511287,1.,0.923879532511287,1.,0.923879532511287,1.,0.923879532511287,
1.,0.923879532511287,1.,0.923879532511287,1.,0.923879532511287,1.,0.923879532511287,
1.,0.923879532511287,1.,0.923879532511287,1.,0.923879532511287,1.)))
REPRESENTATION_ITEM('')
SURFACE()
);
#558=(
BOUNDED_SURFACE()
B_SPLINE_SURFACE(1,2,((#20455,#20456,#20457,#20458,#20459,#20460,#20461,
#20462,#20463,#20464,#20465,#20466,#20467,#20468,#20469,#20470,#20471,#20472,
#20473,#20474,#20475,#20476,#20477,#20478,#20479,#20480,#20481,#20482,#20483,
#20484,#20485,#20486,#20487,#20488,#20489,#20490,#20491,#20492,#20493,#20494,
#20495,#20496,#20497,#20498,#20499,#20500,#20501,#20502,#20503,#20504,#20505,
#20506,#20507,#20508,#20509,#20510,#20511,#20512,#20513,#20514,#20515,#20516,
#20517,#20518,#20519,#20520,#20521,#20522,#20523,#20524,#20525,#20526,#20527,
#20528,#20529,#20530,#20531,#20532,#20533,#20534,#20535,#20536,#20537,#20538,
#20539,#20540,#20541,#20542,#20543,#20544,#20545,#20546,#20547,#20548,#20549,
#20550,#20551,#20552,#20553,#20554,#20555,#20556,#20557,#20558,#20559,#20560,
#20561,#20562,#20563,#20564,#20565,#20566,#20567,#20568,#20569,#20570,#20571,
#20572,#20573,#20574,#20575,#20576,#20577,#20578,#20579,#20580,#20581,#20582,
#20583,#20584,#20585,#20586,#20587,#20588,#20589,#20590,#20591,#20592,#20593,
#20594,#20595,#20596,#20597,#20598,#20599,#20600,#20601,#20602,#20603,#20604,
#20605,#20606,#20607,#20608,#20609,#20610,#20611,#20612,#20613,#20614,#20615),
(#20616,#20617,#20618,#20619,#20620,#20621,#20622,#20623,#20624,#20625,
#20626,#20627,#20628,#20629,#20630,#20631,#20632,#20633,#20634,#20635,#20636,
#20637,#20638,#20639,#20640,#20641,#20642,#20643,#20644,#20645,#20646,#20647,
#20648,#20649,#20650,#20651,#20652,#20653,#20654,#20655,#20656,#20657,#20658,
#20659,#20660,#20661,#20662,#20663,#20664,#20665,#20666,#20667,#20668,#20669,
#20670,#20671,#20672,#20673,#20674,#20675,#20676,#20677,#20678,#20679,#20680,
#20681,#20682,#20683,#20684,#20685,#20686,#20687,#20688,#20689,#20690,#20691,
#20692,#20693,#20694,#20695,#20696,#20697,#20698,#20699,#20700,#20701,#20702,
#20703,#20704,#20705,#20706,#20707,#20708,#20709,#20710,#20711,#20712,#20713,
#20714,#20715,#20716,#20717,#20718,#20719,#20720,#20721,#20722,#20723,#20724,
#20725,#20726,#20727,#20728,#20729,#20730,#20731,#20732,#20733,#20734,#20735,
#20736,#20737,#20738,#20739,#20740,#20741,#20742,#20743,#20744,#20745,#20746,
#20747,#20748,#20749,#20750,#20751,#20752,#20753,#20754,#20755,#20756,#20757,
#20758,#20759,#20760,#20761,#20762,#20763,#20764,#20765,#20766,#20767,#20768,
#20769,#20770,#20771,#20772,#20773,#20774,#20775,#20776)),.UNSPECIFIED.,
 .F.,.F.,.F.)
B_SPLINE_SURFACE_WITH_KNOTS((2,2),(3,2,2,2,2,2,2,2,2,2,2,2,2,2,2,2,2,2,
2,2,2,2,2,2,2,2,2,2,2,2,2,2,2,2,2,2,2,2,2,2,2,2,2,2,2,2,2,2,2,2,2,2,2,2,
2,2,2,2,2,2,2,2,2,2,2,2,2,2,2,2,2,2,2,2,2,2,2,2,2,2,3),(0.,1.),(0.,0.0125,
0.025,0.0375,0.05,0.0625,0.075,0.0875,0.1,0.1125,0.125,0.1375,0.15,0.1625,
0.175,0.1875,0.2,0.2125,0.225,0.2375,0.25,0.2625,0.275,0.2875,0.3,0.3125,
0.325,0.3375,0.35,0.3625,0.375,0.3875,0.4,0.4125,0.425,0.4375,0.45,0.4625,
0.475,0.4875,0.5,0.5125,0.525,0.5375,0.55,0.5625,0.575,0.5875,0.6,0.6125,
0.625,0.6375,0.65,0.6625,0.675,0.6875,0.7,0.7125,0.725,0.7375,0.75,0.7625,
0.775,0.7875,0.8,0.8125,0.825,0.8375,0.85,0.8625,0.875,0.8875,0.9,0.9125,
0.925,0.9375,0.95,0.9625,0.975,0.9875,1.),.UNSPECIFIED.)
GEOMETRIC_REPRESENTATION_ITEM()
RATIONAL_B_SPLINE_SURFACE(((1.,0.923879532511287,1.,0.923879532511287,1.,
0.923879532511287,1.,0.923879532511287,1.,0.923879532511287,1.,0.923879532511287,
1.,0.923879532511287,1.,0.923879532511287,1.,0.923879532511287,1.,0.923879532511287,
1.,0.923879532511287,1.,0.923879532511287,1.,0.923879532511287,1.,0.923879532511287,
1.,0.923879532511287,1.,0.923879532511287,1.,0.923879532511287,1.,0.923879532511287,
1.,0.923879532511287,1.,0.923879532511287,1.,0.923879532511287,1.,0.923879532511287,
1.,0.923879532511287,1.,0.923879532511287,1.,0.923879532511287,1.,0.923879532511287,
1.,0.923879532511287,1.,0.923879532511287,1.,0.923879532511287,1.,0.923879532511287,
1.,0.923879532511287,1.,0.923879532511287,1.,0.923879532511287,1.,0.923879532511287,
1.,0.923879532511287,1.,0.923879532511287,1.,0.923879532511287,1.,0.923879532511287,
1.,0.923879532511287,1.,0.923879532511287,1.,0.923879532511287,1.,0.923879532511287,
1.,0.923879532511287,1.,0.923879532511287,1.,0.923879532511287,1.,0.923879532511287,
1.,0.923879532511287,1.,0.923879532511287,1.,0.923879532511287,1.,0.923879532511287,
1.,0.923879532511287,1.,0.923879532511287,1.,0.923879532511287,1.,0.923879532511287,
1.,0.923879532511287,1.,0.923879532511287,1.,0.923879532511287,1.,0.923879532511287,
1.,0.923879532511287,1.,0.923879532511287,1.,0.923879532511287,1.,0.923879532511287,
1.,0.923879532511287,1.,0.923879532511287,1.,0.923879532511287,1.,0.923879532511287,
1.,0.923879532511287,1.,0.923879532511287,1.,0.923879532511287,1.,0.923879532511287,
1.,0.923879532511287,1.,0.923879532511287,1.,0.923879532511287,1.,0.923879532511287,
1.,0.923879532511287,1.,0.923879532511287,1.,0.923879532511287,1.,0.923879532511287,
1.,0.923879532511287,1.,0.923879532511287,1.),(1.,0.923879532511287,1.,
0.923879532511287,1.,0.923879532511287,1.,0.923879532511287,1.,0.923879532511287,
1.,0.923879532511287,1.,0.923879532511287,1.,0.923879532511287,1.,0.923879532511287,
1.,0.923879532511287,1.,0.923879532511287,1.,0.923879532511287,1.,0.923879532511287,
1.,0.923879532511287,1.,0.923879532511287,1.,0.923879532511287,1.,0.923879532511287,
1.,0.923879532511287,1.,0.923879532511287,1.,0.923879532511287,1.,0.923879532511287,
1.,0.923879532511287,1.,0.923879532511287,1.,0.923879532511287,1.,0.923879532511287,
1.,0.923879532511287,1.,0.923879532511287,1.,0.923879532511287,1.,0.923879532511287,
1.,0.923879532511287,1.,0.923879532511287,1.,0.923879532511287,1.,0.923879532511287,
1.,0.923879532511287,1.,0.923879532511287,1.,0.923879532511287,1.,0.923879532511287,
1.,0.923879532511287,1.,0.923879532511287,1.,0.923879532511287,1.,0.923879532511287,
1.,0.923879532511287,1.,0.923879532511287,1.,0.923879532511287,1.,0.923879532511287,
1.,0.923879532511287,1.,0.923879532511287,1.,0.923879532511287,1.,0.923879532511287,
1.,0.923879532511287,1.,0.923879532511287,1.,0.923879532511287,1.,0.923879532511287,
1.,0.923879532511287,1.,0.923879532511287,1.,0.923879532511287,1.,0.923879532511287,
1.,0.923879532511287,1.,0.923879532511287,1.,0.923879532511287,1.,0.923879532511287,
1.,0.923879532511287,1.,0.923879532511287,1.,0.923879532511287,1.,0.923879532511287,
1.,0.923879532511287,1.,0.923879532511287,1.,0.923879532511287,1.,0.923879532511287,
1.,0.923879532511287,1.,0.923879532511287,1.,0.923879532511287,1.,0.923879532511287,
1.,0.923879532511287,1.,0.923879532511287,1.,0.923879532511287,1.,0.923879532511287,
1.,0.923879532511287,1.,0.923879532511287,1.,0.923879532511287,1.)))
REPRESENTATION_ITEM('')
SURFACE()
);
#559=(
BOUNDED_SURFACE()
B_SPLINE_SURFACE(3,2,((#20786,#20787,#20788,#20789,#20790,#20791,#20792,
#20793,#20794,#20795,#20796,#20797,#20798,#20799,#20800,#20801,#20802,#20803,
#20804,#20805,#20806,#20807,#20808,#20809,#20810,#20811,#20812,#20813,#20814,
#20815,#20816,#20817,#20818,#20819,#20820,#20821,#20822,#20823,#20824,#20825,
#20826,#20827,#20828,#20829,#20830,#20831,#20832,#20833,#20834,#20835,#20836,
#20837,#20838,#20839,#20840,#20841,#20842,#20843,#20844,#20845,#20846,#20847,
#20848,#20849,#20850,#20851,#20852,#20853,#20854,#20855,#20856,#20857,#20858,
#20859,#20860,#20861,#20862,#20863,#20864,#20865,#20866,#20867,#20868,#20869,
#20870,#20871,#20872,#20873,#20874,#20875,#20876,#20877,#20878,#20879,#20880,
#20881,#20882,#20883,#20884,#20885,#20886,#20887,#20888,#20889,#20890,#20891,
#20892,#20893,#20894,#20895,#20896,#20897,#20898,#20899,#20900,#20901,#20902,
#20903,#20904,#20905,#20906,#20907,#20908,#20909,#20910,#20911,#20912,#20913,
#20914,#20915,#20916,#20917,#20918,#20919,#20920,#20921,#20922,#20923,#20924,
#20925,#20926,#20927,#20928,#20929,#20930,#20931,#20932,#20933,#20934,#20935,
#20936,#20937,#20938,#20939,#20940,#20941,#20942,#20943,#20944,#20945,#20946),
(#20947,#20948,#20949,#20950,#20951,#20952,#20953,#20954,#20955,#20956,
#20957,#20958,#20959,#20960,#20961,#20962,#20963,#20964,#20965,#20966,#20967,
#20968,#20969,#20970,#20971,#20972,#20973,#20974,#20975,#20976,#20977,#20978,
#20979,#20980,#20981,#20982,#20983,#20984,#20985,#20986,#20987,#20988,#20989,
#20990,#20991,#20992,#20993,#20994,#20995,#20996,#20997,#20998,#20999,#21000,
#21001,#21002,#21003,#21004,#21005,#21006,#21007,#21008,#21009,#21010,#21011,
#21012,#21013,#21014,#21015,#21016,#21017,#21018,#21019,#21020,#21021,#21022,
#21023,#21024,#21025,#21026,#21027,#21028,#21029,#21030,#21031,#21032,#21033,
#21034,#21035,#21036,#21037,#21038,#21039,#21040,#21041,#21042,#21043,#21044,
#21045,#21046,#21047,#21048,#21049,#21050,#21051,#21052,#21053,#21054,#21055,
#21056,#21057,#21058,#21059,#21060,#21061,#21062,#21063,#21064,#21065,#21066,
#21067,#21068,#21069,#21070,#21071,#21072,#21073,#21074,#21075,#21076,#21077,
#21078,#21079,#21080,#21081,#21082,#21083,#21084,#21085,#21086,#21087,#21088,
#21089,#21090,#21091,#21092,#21093,#21094,#21095,#21096,#21097,#21098,#21099,
#21100,#21101,#21102,#21103,#21104,#21105,#21106,#21107),(#21108,#21109,
#21110,#21111,#21112,#21113,#21114,#21115,#21116,#21117,#21118,#21119,#21120,
#21121,#21122,#21123,#21124,#21125,#21126,#21127,#21128,#21129,#21130,#21131,
#21132,#21133,#21134,#21135,#21136,#21137,#21138,#21139,#21140,#21141,#21142,
#21143,#21144,#21145,#21146,#21147,#21148,#21149,#21150,#21151,#21152,#21153,
#21154,#21155,#21156,#21157,#21158,#21159,#21160,#21161,#21162,#21163,#21164,
#21165,#21166,#21167,#21168,#21169,#21170,#21171,#21172,#21173,#21174,#21175,
#21176,#21177,#21178,#21179,#21180,#21181,#21182,#21183,#21184,#21185,#21186,
#21187,#21188,#21189,#21190,#21191,#21192,#21193,#21194,#21195,#21196,#21197,
#21198,#21199,#21200,#21201,#21202,#21203,#21204,#21205,#21206,#21207,#21208,
#21209,#21210,#21211,#21212,#21213,#21214,#21215,#21216,#21217,#21218,#21219,
#21220,#21221,#21222,#21223,#21224,#21225,#21226,#21227,#21228,#21229,#21230,
#21231,#21232,#21233,#21234,#21235,#21236,#21237,#21238,#21239,#21240,#21241,
#21242,#21243,#21244,#21245,#21246,#21247,#21248,#21249,#21250,#21251,#21252,
#21253,#21254,#21255,#21256,#21257,#21258,#21259,#21260,#21261,#21262,#21263,
#21264,#21265,#21266,#21267,#21268),(#21269,#21270,#21271,#21272,#21273,
#21274,#21275,#21276,#21277,#21278,#21279,#21280,#21281,#21282,#21283,#21284,
#21285,#21286,#21287,#21288,#21289,#21290,#21291,#21292,#21293,#21294,#21295,
#21296,#21297,#21298,#21299,#21300,#21301,#21302,#21303,#21304,#21305,#21306,
#21307,#21308,#21309,#21310,#21311,#21312,#21313,#21314,#21315,#21316,#21317,
#21318,#21319,#21320,#21321,#21322,#21323,#21324,#21325,#21326,#21327,#21328,
#21329,#21330,#21331,#21332,#21333,#21334,#21335,#21336,#21337,#21338,#21339,
#21340,#21341,#21342,#21343,#21344,#21345,#21346,#21347,#21348,#21349,#21350,
#21351,#21352,#21353,#21354,#21355,#21356,#21357,#21358,#21359,#21360,#21361,
#21362,#21363,#21364,#21365,#21366,#21367,#21368,#21369,#21370,#21371,#21372,
#21373,#21374,#21375,#21376,#21377,#21378,#21379,#21380,#21381,#21382,#21383,
#21384,#21385,#21386,#21387,#21388,#21389,#21390,#21391,#21392,#21393,#21394,
#21395,#21396,#21397,#21398,#21399,#21400,#21401,#21402,#21403,#21404,#21405,
#21406,#21407,#21408,#21409,#21410,#21411,#21412,#21413,#21414,#21415,#21416,
#21417,#21418,#21419,#21420,#21421,#21422,#21423,#21424,#21425,#21426,#21427,
#21428,#21429)),.UNSPECIFIED.,.F.,.F.,.F.)
B_SPLINE_SURFACE_WITH_KNOTS((4,4),(3,2,2,2,2,2,2,2,2,2,2,2,2,2,2,2,2,2,
2,2,2,2,2,2,2,2,2,2,2,2,2,2,2,2,2,2,2,2,2,2,2,2,2,2,2,2,2,2,2,2,2,2,2,2,
2,2,2,2,2,2,2,2,2,2,2,2,2,2,2,2,2,2,2,2,2,2,2,2,2,2,3),(0.,1.),(0.,0.0125,
0.025,0.0375,0.05,0.0625,0.075,0.0875,0.1,0.1125,0.125,0.1375,0.15,0.1625,
0.175,0.1875,0.2,0.2125,0.225,0.2375,0.25,0.2625,0.275,0.2875,0.3,0.3125,
0.325,0.3375,0.35,0.3625,0.375,0.3875,0.4,0.4125,0.425,0.4375,0.45,0.4625,
0.475,0.4875,0.5,0.5125,0.525,0.5375,0.55,0.5625,0.575,0.5875,0.6,0.6125,
0.625,0.6375,0.65,0.6625,0.675,0.6875,0.7,0.7125,0.725,0.7375,0.75,0.7625,
0.775,0.7875,0.8,0.8125,0.825,0.8375,0.85,0.8625,0.875,0.8875,0.9,0.9125,
0.925,0.9375,0.95,0.9625,0.975,0.9875,1.),.UNSPECIFIED.)
GEOMETRIC_REPRESENTATION_ITEM()
RATIONAL_B_SPLINE_SURFACE(((1.,0.923879532511287,1.,0.923879532511287,1.,
0.923879532511287,1.,0.923879532511287,1.,0.923879532511287,1.,0.923879532511287,
1.,0.923879532511287,1.,0.923879532511287,1.,0.923879532511287,1.,0.923879532511287,
1.,0.923879532511287,1.,0.923879532511287,1.,0.923879532511287,1.,0.923879532511287,
1.,0.923879532511287,1.,0.923879532511287,1.,0.923879532511287,1.,0.923879532511287,
1.,0.923879532511287,1.,0.923879532511287,1.,0.923879532511287,1.,0.923879532511287,
1.,0.923879532511287,1.,0.923879532511287,1.,0.923879532511287,1.,0.923879532511287,
1.,0.923879532511287,1.,0.923879532511287,1.,0.923879532511287,1.,0.923879532511287,
1.,0.923879532511287,1.,0.923879532511287,1.,0.923879532511287,1.,0.923879532511287,
1.,0.923879532511287,1.,0.923879532511287,1.,0.923879532511287,1.,0.923879532511287,
1.,0.923879532511287,1.,0.923879532511287,1.,0.923879532511287,1.,0.923879532511287,
1.,0.923879532511287,1.,0.923879532511287,1.,0.923879532511287,1.,0.923879532511287,
1.,0.923879532511287,1.,0.923879532511287,1.,0.923879532511287,1.,0.923879532511287,
1.,0.923879532511287,1.,0.923879532511287,1.,0.923879532511287,1.,0.923879532511287,
1.,0.923879532511287,1.,0.923879532511287,1.,0.923879532511287,1.,0.923879532511287,
1.,0.923879532511287,1.,0.923879532511287,1.,0.923879532511287,1.,0.923879532511287,
1.,0.923879532511287,1.,0.923879532511287,1.,0.923879532511287,1.,0.923879532511287,
1.,0.923879532511287,1.,0.923879532511287,1.,0.923879532511287,1.,0.923879532511287,
1.,0.923879532511287,1.,0.923879532511287,1.,0.923879532511287,1.,0.923879532511287,
1.,0.923879532511287,1.,0.923879532511287,1.,0.923879532511287,1.,0.923879532511287,
1.,0.923879532511287,1.,0.923879532511287,1.),(0.998696642611305,0.922675387296324,
0.998696642611305,0.922675387296324,0.998696642611305,0.922675387296324,
0.998696642611305,0.922675387296324,0.998696642611305,0.922675387296324,
0.998696642611305,0.922675387296324,0.998696642611305,0.922675387296324,
0.998696642611305,0.922675387296324,0.998696642611305,0.922675387296324,
0.998696642611305,0.922675387296324,0.998696642611305,0.922675387296324,
0.998696642611305,0.922675387296324,0.998696642611305,0.922675387296324,
0.998696642611305,0.922675387296324,0.998696642611305,0.922675387296324,
0.998696642611305,0.922675387296324,0.998696642611305,0.922675387296324,
0.998696642611305,0.922675387296324,0.998696642611305,0.922675387296324,
0.998696642611305,0.922675387296324,0.998696642611305,0.922675387296324,
0.998696642611305,0.922675387296324,0.998696642611305,0.922675387296324,
0.998696642611305,0.922675387296324,0.998696642611305,0.922675387296324,
0.998696642611305,0.922675387296324,0.998696642611305,0.922675387296324,
0.998696642611305,0.922675387296324,0.998696642611305,0.922675387296324,
0.998696642611305,0.922675387296324,0.998696642611305,0.922675387296324,
0.998696642611305,0.922675387296324,0.998696642611305,0.922675387296324,
0.998696642611305,0.922675387296324,0.998696642611305,0.922675387296324,
0.998696642611305,0.922675387296324,0.998696642611305,0.922675387296324,
0.998696642611305,0.922675387296324,0.998696642611305,0.922675387296324,
0.998696642611305,0.922675387296324,0.998696642611305,0.922675387296324,
0.998696642611305,0.922675387296324,0.998696642611305,0.922675387296324,
0.998696642611305,0.922675387296324,0.998696642611305,0.922675387296324,
0.998696642611305,0.922675387296324,0.998696642611305,0.922675387296324,
0.998696642611305,0.922675387296324,0.998696642611305,0.922675387296324,
0.998696642611305,0.922675387296324,0.998696642611305,0.922675387296324,
0.998696642611305,0.922675387296324,0.998696642611305,0.922675387296324,
0.998696642611305,0.922675387296324,0.998696642611305,0.922675387296324,
0.998696642611305,0.922675387296324,0.998696642611305,0.922675387296324,
0.998696642611305,0.922675387296324,0.998696642611305,0.922675387296324,
0.998696642611305,0.922675387296324,0.998696642611305,0.922675387296324,
0.998696642611305,0.922675387296324,0.998696642611305,0.922675387296324,
0.998696642611305,0.922675387296324,0.998696642611305,0.922675387296324,
0.998696642611305,0.922675387296324,0.998696642611305,0.922675387296324,
0.998696642611305,0.922675387296324,0.998696642611305,0.922675387296324,
0.998696642611305,0.922675387296324,0.998696642611305,0.922675387296324,
0.998696642611305,0.922675387296324,0.998696642611305,0.922675387296324,
0.998696642611305,0.922675387296324,0.998696642611305,0.922675387296324,
0.998696642611305,0.922675387296324,0.998696642611305,0.922675387296324,
0.998696642611305,0.922675387296324,0.998696642611305,0.922675387296324,
0.998696642611305,0.922675387296324,0.998696642611305),(0.998696642611305,
0.922675387296324,0.998696642611305,0.922675387296324,0.998696642611305,
0.922675387296324,0.998696642611305,0.922675387296324,0.998696642611305,
0.922675387296324,0.998696642611305,0.922675387296324,0.998696642611305,
0.922675387296324,0.998696642611305,0.922675387296324,0.998696642611305,
0.922675387296324,0.998696642611305,0.922675387296324,0.998696642611305,
0.922675387296324,0.998696642611305,0.922675387296324,0.998696642611305,
0.922675387296324,0.998696642611305,0.922675387296324,0.998696642611305,
0.922675387296324,0.998696642611305,0.922675387296324,0.998696642611305,
0.922675387296324,0.998696642611305,0.922675387296324,0.998696642611305,
0.922675387296324,0.998696642611305,0.922675387296324,0.998696642611305,
0.922675387296324,0.998696642611305,0.922675387296324,0.998696642611305,
0.922675387296324,0.998696642611305,0.922675387296324,0.998696642611305,
0.922675387296324,0.998696642611305,0.922675387296324,0.998696642611305,
0.922675387296324,0.998696642611305,0.922675387296324,0.998696642611305,
0.922675387296324,0.998696642611305,0.922675387296324,0.998696642611305,
0.922675387296324,0.998696642611305,0.922675387296324,0.998696642611305,
0.922675387296324,0.998696642611305,0.922675387296324,0.998696642611305,
0.922675387296324,0.998696642611305,0.922675387296324,0.998696642611305,
0.922675387296324,0.998696642611305,0.922675387296324,0.998696642611305,
0.922675387296324,0.998696642611305,0.922675387296324,0.998696642611305,
0.922675387296324,0.998696642611305,0.922675387296324,0.998696642611305,
0.922675387296324,0.998696642611305,0.922675387296324,0.998696642611305,
0.922675387296324,0.998696642611305,0.922675387296324,0.998696642611305,
0.922675387296324,0.998696642611305,0.922675387296324,0.998696642611305,
0.922675387296324,0.998696642611305,0.922675387296324,0.998696642611305,
0.922675387296324,0.998696642611305,0.922675387296324,0.998696642611305,
0.922675387296324,0.998696642611305,0.922675387296324,0.998696642611305,
0.922675387296324,0.998696642611305,0.922675387296324,0.998696642611305,
0.922675387296324,0.998696642611305,0.922675387296324,0.998696642611305,
0.922675387296324,0.998696642611305,0.922675387296324,0.998696642611305,
0.922675387296324,0.998696642611305,0.922675387296324,0.998696642611305,
0.922675387296324,0.998696642611305,0.922675387296324,0.998696642611305,
0.922675387296324,0.998696642611305,0.922675387296324,0.998696642611305,
0.922675387296324,0.998696642611305,0.922675387296324,0.998696642611305,
0.922675387296324,0.998696642611305,0.922675387296324,0.998696642611305,
0.922675387296324,0.998696642611305,0.922675387296324,0.998696642611305,
0.922675387296324,0.998696642611305,0.922675387296324,0.998696642611305,
0.922675387296324,0.998696642611305,0.922675387296324,0.998696642611305,
0.922675387296324,0.998696642611305,0.922675387296324,0.998696642611305,
0.922675387296324,0.998696642611305,0.922675387296324,0.998696642611305),
(1.,0.923879532511287,1.,0.923879532511287,1.,0.923879532511287,1.,0.923879532511287,
1.,0.923879532511287,1.,0.923879532511287,1.,0.923879532511287,1.,0.923879532511287,
1.,0.923879532511287,1.,0.923879532511287,1.,0.923879532511287,1.,0.923879532511287,
1.,0.923879532511287,1.,0.923879532511287,1.,0.923879532511287,1.,0.923879532511287,
1.,0.923879532511287,1.,0.923879532511287,1.,0.923879532511287,1.,0.923879532511287,
1.,0.923879532511287,1.,0.923879532511287,1.,0.923879532511287,1.,0.923879532511287,
1.,0.923879532511287,1.,0.923879532511287,1.,0.923879532511287,1.,0.923879532511287,
1.,0.923879532511287,1.,0.923879532511287,1.,0.923879532511287,1.,0.923879532511287,
1.,0.923879532511287,1.,0.923879532511287,1.,0.923879532511287,1.,0.923879532511287,
1.,0.923879532511287,1.,0.923879532511287,1.,0.923879532511287,1.,0.923879532511287,
1.,0.923879532511287,1.,0.923879532511287,1.,0.923879532511287,1.,0.923879532511287,
1.,0.923879532511287,1.,0.923879532511287,1.,0.923879532511287,1.,0.923879532511287,
1.,0.923879532511287,1.,0.923879532511287,1.,0.923879532511287,1.,0.923879532511287,
1.,0.923879532511287,1.,0.923879532511287,1.,0.923879532511287,1.,0.923879532511287,
1.,0.923879532511287,1.,0.923879532511287,1.,0.923879532511287,1.,0.923879532511287,
1.,0.923879532511287,1.,0.923879532511287,1.,0.923879532511287,1.,0.923879532511287,
1.,0.923879532511287,1.,0.923879532511287,1.,0.923879532511287,1.,0.923879532511287,
1.,0.923879532511287,1.,0.923879532511287,1.,0.923879532511287,1.,0.923879532511287,
1.,0.923879532511287,1.,0.923879532511287,1.,0.923879532511287,1.,0.923879532511287,
1.,0.923879532511287,1.,0.923879532511287,1.,0.923879532511287,1.,0.923879532511287,
1.)))
REPRESENTATION_ITEM('')
SURFACE()
);
#560=(
BOUNDED_SURFACE()
B_SPLINE_SURFACE(3,2,((#21430,#21431,#21432,#21433,#21434,#21435,#21436,
#21437,#21438,#21439,#21440,#21441,#21442,#21443,#21444,#21445,#21446,#21447,
#21448,#21449,#21450,#21451,#21452,#21453,#21454,#21455,#21456,#21457,#21458,
#21459,#21460,#21461,#21462,#21463,#21464,#21465,#21466,#21467,#21468,#21469,
#21470,#21471,#21472,#21473,#21474,#21475,#21476,#21477,#21478,#21479,#21480,
#21481,#21482,#21483,#21484,#21485,#21486,#21487,#21488,#21489,#21490,#21491,
#21492,#21493,#21494,#21495,#21496,#21497,#21498,#21499,#21500,#21501,#21502,
#21503,#21504,#21505,#21506,#21507,#21508,#21509,#21510,#21511,#21512,#21513,
#21514,#21515,#21516,#21517,#21518,#21519,#21520,#21521,#21522,#21523,#21524,
#21525,#21526,#21527,#21528,#21529,#21530,#21531,#21532,#21533,#21534,#21535,
#21536,#21537,#21538,#21539,#21540,#21541,#21542,#21543,#21544,#21545,#21546,
#21547,#21548,#21549,#21550,#21551,#21552,#21553,#21554,#21555,#21556,#21557,
#21558,#21559,#21560,#21561,#21562,#21563,#21564,#21565,#21566,#21567,#21568,
#21569,#21570,#21571,#21572,#21573,#21574,#21575,#21576,#21577,#21578,#21579,
#21580,#21581,#21582,#21583,#21584,#21585,#21586,#21587,#21588,#21589,#21590),
(#21591,#21592,#21593,#21594,#21595,#21596,#21597,#21598,#21599,#21600,
#21601,#21602,#21603,#21604,#21605,#21606,#21607,#21608,#21609,#21610,#21611,
#21612,#21613,#21614,#21615,#21616,#21617,#21618,#21619,#21620,#21621,#21622,
#21623,#21624,#21625,#21626,#21627,#21628,#21629,#21630,#21631,#21632,#21633,
#21634,#21635,#21636,#21637,#21638,#21639,#21640,#21641,#21642,#21643,#21644,
#21645,#21646,#21647,#21648,#21649,#21650,#21651,#21652,#21653,#21654,#21655,
#21656,#21657,#21658,#21659,#21660,#21661,#21662,#21663,#21664,#21665,#21666,
#21667,#21668,#21669,#21670,#21671,#21672,#21673,#21674,#21675,#21676,#21677,
#21678,#21679,#21680,#21681,#21682,#21683,#21684,#21685,#21686,#21687,#21688,
#21689,#21690,#21691,#21692,#21693,#21694,#21695,#21696,#21697,#21698,#21699,
#21700,#21701,#21702,#21703,#21704,#21705,#21706,#21707,#21708,#21709,#21710,
#21711,#21712,#21713,#21714,#21715,#21716,#21717,#21718,#21719,#21720,#21721,
#21722,#21723,#21724,#21725,#21726,#21727,#21728,#21729,#21730,#21731,#21732,
#21733,#21734,#21735,#21736,#21737,#21738,#21739,#21740,#21741,#21742,#21743,
#21744,#21745,#21746,#21747,#21748,#21749,#21750,#21751),(#21752,#21753,
#21754,#21755,#21756,#21757,#21758,#21759,#21760,#21761,#21762,#21763,#21764,
#21765,#21766,#21767,#21768,#21769,#21770,#21771,#21772,#21773,#21774,#21775,
#21776,#21777,#21778,#21779,#21780,#21781,#21782,#21783,#21784,#21785,#21786,
#21787,#21788,#21789,#21790,#21791,#21792,#21793,#21794,#21795,#21796,#21797,
#21798,#21799,#21800,#21801,#21802,#21803,#21804,#21805,#21806,#21807,#21808,
#21809,#21810,#21811,#21812,#21813,#21814,#21815,#21816,#21817,#21818,#21819,
#21820,#21821,#21822,#21823,#21824,#21825,#21826,#21827,#21828,#21829,#21830,
#21831,#21832,#21833,#21834,#21835,#21836,#21837,#21838,#21839,#21840,#21841,
#21842,#21843,#21844,#21845,#21846,#21847,#21848,#21849,#21850,#21851,#21852,
#21853,#21854,#21855,#21856,#21857,#21858,#21859,#21860,#21861,#21862,#21863,
#21864,#21865,#21866,#21867,#21868,#21869,#21870,#21871,#21872,#21873,#21874,
#21875,#21876,#21877,#21878,#21879,#21880,#21881,#21882,#21883,#21884,#21885,
#21886,#21887,#21888,#21889,#21890,#21891,#21892,#21893,#21894,#21895,#21896,
#21897,#21898,#21899,#21900,#21901,#21902,#21903,#21904,#21905,#21906,#21907,
#21908,#21909,#21910,#21911,#21912),(#21913,#21914,#21915,#21916,#21917,
#21918,#21919,#21920,#21921,#21922,#21923,#21924,#21925,#21926,#21927,#21928,
#21929,#21930,#21931,#21932,#21933,#21934,#21935,#21936,#21937,#21938,#21939,
#21940,#21941,#21942,#21943,#21944,#21945,#21946,#21947,#21948,#21949,#21950,
#21951,#21952,#21953,#21954,#21955,#21956,#21957,#21958,#21959,#21960,#21961,
#21962,#21963,#21964,#21965,#21966,#21967,#21968,#21969,#21970,#21971,#21972,
#21973,#21974,#21975,#21976,#21977,#21978,#21979,#21980,#21981,#21982,#21983,
#21984,#21985,#21986,#21987,#21988,#21989,#21990,#21991,#21992,#21993,#21994,
#21995,#21996,#21997,#21998,#21999,#22000,#22001,#22002,#22003,#22004,#22005,
#22006,#22007,#22008,#22009,#22010,#22011,#22012,#22013,#22014,#22015,#22016,
#22017,#22018,#22019,#22020,#22021,#22022,#22023,#22024,#22025,#22026,#22027,
#22028,#22029,#22030,#22031,#22032,#22033,#22034,#22035,#22036,#22037,#22038,
#22039,#22040,#22041,#22042,#22043,#22044,#22045,#22046,#22047,#22048,#22049,
#22050,#22051,#22052,#22053,#22054,#22055,#22056,#22057,#22058,#22059,#22060,
#22061,#22062,#22063,#22064,#22065,#22066,#22067,#22068,#22069,#22070,#22071,
#22072,#22073)),.UNSPECIFIED.,.F.,.F.,.F.)
B_SPLINE_SURFACE_WITH_KNOTS((4,4),(3,2,2,2,2,2,2,2,2,2,2,2,2,2,2,2,2,2,
2,2,2,2,2,2,2,2,2,2,2,2,2,2,2,2,2,2,2,2,2,2,2,2,2,2,2,2,2,2,2,2,2,2,2,2,
2,2,2,2,2,2,2,2,2,2,2,2,2,2,2,2,2,2,2,2,2,2,2,2,2,2,3),(0.,1.00288579446161),
(0.,0.0125,0.025,0.0375,0.05,0.0625,0.075,0.0875,0.1,0.1125,0.125,0.1375,
0.15,0.1625,0.175,0.1875,0.2,0.2125,0.225,0.2375,0.25,0.2625,0.275,0.2875,
0.3,0.3125,0.325,0.3375,0.35,0.3625,0.375,0.3875,0.4,0.4125,0.425,0.4375,
0.45,0.4625,0.475,0.4875,0.5,0.5125,0.525,0.5375,0.55,0.5625,0.575,0.5875,
0.6,0.6125,0.625,0.6375,0.65,0.6625,0.675,0.6875,0.7,0.7125,0.725,0.7375,
0.75,0.7625,0.775,0.7875,0.8,0.8125,0.825,0.8375,0.85,0.8625,0.875,0.8875,
0.9,0.9125,0.925,0.9375,0.95,0.9625,0.975,0.9875,1.00288579446161),
 .UNSPECIFIED.)
GEOMETRIC_REPRESENTATION_ITEM()
RATIONAL_B_SPLINE_SURFACE(((1.,0.923879532511287,1.,0.923879532511287,1.,
0.923879532511287,1.,0.923879532511287,1.,0.923879532511287,1.,0.923879532511287,
1.,0.923879532511287,1.,0.923879532511287,1.,0.923879532511287,1.,0.923879532511287,
1.,0.923879532511287,1.,0.923879532511287,1.,0.923879532511287,1.,0.923879532511287,
1.,0.923879532511287,1.,0.923879532511287,1.,0.923879532511287,1.,0.923879532511287,
1.,0.923879532511287,1.,0.923879532511287,1.,0.923879532511287,1.,0.923879532511287,
1.,0.923879532511287,1.,0.923879532511287,1.,0.923879532511287,1.,0.923879532511287,
1.,0.923879532511287,1.,0.923879532511287,1.,0.923879532511287,1.,0.923879532511287,
1.,0.923879532511287,1.,0.923879532511287,1.,0.923879532511287,1.,0.923879532511287,
1.,0.923879532511287,1.,0.923879532511287,1.,0.923879532511287,1.,0.923879532511287,
1.,0.923879532511287,1.,0.923879532511287,1.,0.923879532511287,1.,0.923879532511287,
1.,0.923879532511287,1.,0.923879532511287,1.,0.923879532511287,1.,0.923879532511287,
1.,0.923879532511287,1.,0.923879532511287,1.,0.923879532511287,1.,0.923879532511287,
1.,0.923879532511287,1.,0.923879532511287,1.,0.923879532511287,1.,0.923879532511287,
1.,0.923879532511287,1.,0.923879532511287,1.,0.923879532511287,1.,0.923879532511287,
1.,0.923879532511287,1.,0.923879532511287,1.,0.923879532511287,1.,0.923879532511287,
1.,0.923879532511287,1.,0.923879532511287,1.,0.923879532511287,1.,0.923879532511287,
1.,0.923879532511287,1.,0.923879532511287,1.,0.923879532511287,1.,0.923879532511287,
1.,0.923879532511287,1.,0.923879532511287,1.,0.923879532511287,1.,0.923879532511287,
1.,0.923879532511287,1.,0.923879532511287,1.,0.923879532511287,1.,0.923879532511287,
1.,0.923879532511287,1.,0.90630609063176,1.04326101835863),(0.998692881389771,
0.922671912380731,0.998692881389771,0.922671912380731,0.998692881389771,
0.922671912380731,0.998692881389771,0.922671912380731,0.998692881389771,
0.922671912380731,0.998692881389771,0.922671912380731,0.998692881389771,
0.922671912380731,0.998692881389771,0.922671912380731,0.998692881389771,
0.922671912380731,0.998692881389771,0.922671912380731,0.998692881389771,
0.922671912380731,0.998692881389771,0.922671912380731,0.998692881389771,
0.922671912380731,0.998692881389771,0.922671912380731,0.998692881389771,
0.922671912380731,0.998692881389771,0.922671912380731,0.998692881389771,
0.922671912380731,0.998692881389771,0.922671912380731,0.998692881389771,
0.922671912380731,0.998692881389771,0.922671912380731,0.998692881389771,
0.922671912380731,0.998692881389771,0.922671912380731,0.998692881389771,
0.922671912380731,0.998692881389771,0.922671912380731,0.998692881389771,
0.922671912380731,0.998692881389771,0.922671912380731,0.998692881389771,
0.922671912380731,0.998692881389771,0.922671912380731,0.998692881389771,
0.922671912380731,0.998692881389771,0.922671912380731,0.998692881389771,
0.922671912380731,0.998692881389771,0.922671912380731,0.998692881389771,
0.922671912380731,0.998692881389771,0.922671912380731,0.998692881389771,
0.922671912380731,0.998692881389771,0.922671912380731,0.998692881389771,
0.922671912380731,0.998692881389771,0.922671912380731,0.998692881389771,
0.922671912380731,0.998692881389771,0.922671912380731,0.998692881389771,
0.922671912380731,0.998692881389771,0.922671912380731,0.998692881389771,
0.922671912380731,0.998692881389771,0.922671912380731,0.998692881389771,
0.922671912380731,0.998692881389771,0.922671912380731,0.998692881389771,
0.922671912380731,0.998692881389771,0.922671912380731,0.998692881389771,
0.922671912380731,0.998692881389771,0.922671912380731,0.998692881389771,
0.922671912380731,0.998692881389771,0.922671912380731,0.998692881389771,
0.922671912380731,0.998692881389771,0.922671912380731,0.998692881389771,
0.922671912380731,0.998692881389771,0.922671912380731,0.998692881389771,
0.922671912380731,0.998692881389771,0.922671912380731,0.998692881389771,
0.922671912380731,0.998692881389771,0.922671912380731,0.998692881389771,
0.922671912380731,0.998692881389771,0.922671912380731,0.998692881389771,
0.922671912380731,0.998692881389771,0.922671912380731,0.998692881389771,
0.922671912380731,0.998692881389771,0.922671912380731,0.998692881389771,
0.922671912380731,0.998692881389771,0.922671912380731,0.998692881389771,
0.922671912380731,0.998692881389771,0.922671912380731,0.998692881389771,
0.922671912380731,0.998692881389771,0.922671912380731,0.998692881389771,
0.922671912380731,0.998692881389771,0.922671912380731,0.998692881389771,
0.922671912380731,0.998692881389771,0.922671912380731,0.998692881389771,
0.922671912380731,0.998692881389771,0.922671912380731,0.998692881389771,
0.922671912380731,0.998692881389771,0.905121441074131,1.04189735246621),
(0.998696653465417,0.922675397324216,0.998696653465417,0.922675397324216,
0.998696653465417,0.922675397324216,0.998696653465417,0.922675397324216,
0.998696653465417,0.922675397324216,0.998696653465417,0.922675397324216,
0.998696653465417,0.922675397324216,0.998696653465417,0.922675397324216,
0.998696653465417,0.922675397324216,0.998696653465417,0.922675397324216,
0.998696653465417,0.922675397324216,0.998696653465417,0.922675397324216,
0.998696653465417,0.922675397324216,0.998696653465417,0.922675397324216,
0.998696653465417,0.922675397324216,0.998696653465417,0.922675397324216,
0.998696653465417,0.922675397324216,0.998696653465417,0.922675397324216,
0.998696653465417,0.922675397324216,0.998696653465417,0.922675397324216,
0.998696653465417,0.922675397324216,0.998696653465417,0.922675397324216,
0.998696653465417,0.922675397324216,0.998696653465417,0.922675397324216,
0.998696653465417,0.922675397324216,0.998696653465417,0.922675397324216,
0.998696653465417,0.922675397324216,0.998696653465417,0.922675397324216,
0.998696653465417,0.922675397324216,0.998696653465417,0.922675397324216,
0.998696653465417,0.922675397324216,0.998696653465417,0.922675397324216,
0.998696653465417,0.922675397324216,0.998696653465417,0.922675397324216,
0.998696653465417,0.922675397324216,0.998696653465417,0.922675397324216,
0.998696653465417,0.922675397324216,0.998696653465417,0.922675397324216,
0.998696653465417,0.922675397324216,0.998696653465417,0.922675397324216,
0.998696653465417,0.922675397324216,0.998696653465417,0.922675397324216,
0.998696653465417,0.922675397324216,0.998696653465417,0.922675397324216,
0.998696653465417,0.922675397324216,0.998696653465417,0.922675397324216,
0.998696653465417,0.922675397324216,0.998696653465417,0.922675397324216,
0.998696653465417,0.922675397324216,0.998696653465417,0.922675397324216,
0.998696653465417,0.922675397324216,0.998696653465417,0.922675397324216,
0.998696653465417,0.922675397324216,0.998696653465417,0.922675397324216,
0.998696653465417,0.922675397324216,0.998696653465417,0.922675397324216,
0.998696653465417,0.922675397324216,0.998696653465417,0.922675397324216,
0.998696653465417,0.922675397324216,0.998696653465417,0.922675397324216,
0.998696653465417,0.922675397324216,0.998696653465417,0.922675397324216,
0.998696653465417,0.922675397324216,0.998696653465417,0.922675397324216,
0.998696653465417,0.922675397324216,0.998696653465417,0.922675397324216,
0.998696653465417,0.922675397324216,0.998696653465417,0.922675397324216,
0.998696653465417,0.922675397324216,0.998696653465417,0.922675397324216,
0.998696653465417,0.922675397324216,0.998696653465417,0.922675397324216,
0.998696653465417,0.922675397324216,0.998696653465417,0.922675397324216,
0.998696653465417,0.922675397324216,0.998696653465417,0.922675397324216,
0.998696653465417,0.922675397324216,0.998696653465417,0.922675397324216,
0.998696653465417,0.922675397324216,0.998696653465417,0.905124859729264,
1.04190128772569),(1.00001131622694,0.92388998734174,1.00001131622694,0.92388998734174,
1.00001131622694,0.92388998734174,1.00001131622694,0.92388998734174,1.00001131622694,
0.92388998734174,1.00001131622694,0.92388998734174,1.00001131622694,0.92388998734174,
1.00001131622694,0.92388998734174,1.00001131622694,0.92388998734174,1.00001131622694,
0.92388998734174,1.00001131622694,0.92388998734174,1.00001131622694,0.92388998734174,
1.00001131622694,0.92388998734174,1.00001131622694,0.92388998734174,1.00001131622694,
0.92388998734174,1.00001131622694,0.92388998734174,1.00001131622694,0.92388998734174,
1.00001131622694,0.92388998734174,1.00001131622694,0.92388998734174,1.00001131622694,
0.92388998734174,1.00001131622694,0.92388998734174,1.00001131622694,0.92388998734174,
1.00001131622694,0.92388998734174,1.00001131622694,0.92388998734174,1.00001131622694,
0.92388998734174,1.00001131622694,0.92388998734174,1.00001131622694,0.92388998734174,
1.00001131622694,0.92388998734174,1.00001131622694,0.92388998734174,1.00001131622694,
0.92388998734174,1.00001131622694,0.92388998734174,1.00001131622694,0.92388998734174,
1.00001131622694,0.92388998734174,1.00001131622694,0.92388998734174,1.00001131622694,
0.92388998734174,1.00001131622694,0.92388998734174,1.00001131622694,0.92388998734174,
1.00001131622694,0.92388998734174,1.00001131622694,0.92388998734174,1.00001131622694,
0.92388998734174,1.00001131622694,0.92388998734174,1.00001131622694,0.92388998734174,
1.00001131622694,0.92388998734174,1.00001131622694,0.92388998734174,1.00001131622694,
0.92388998734174,1.00001131622694,0.92388998734174,1.00001131622694,0.92388998734174,
1.00001131622694,0.92388998734174,1.00001131622694,0.92388998734174,1.00001131622694,
0.92388998734174,1.00001131622694,0.92388998734174,1.00001131622694,0.92388998734174,
1.00001131622694,0.92388998734174,1.00001131622694,0.92388998734174,1.00001131622694,
0.92388998734174,1.00001131622694,0.92388998734174,1.00001131622694,0.92388998734174,
1.00001131622694,0.92388998734174,1.00001131622694,0.92388998734174,1.00001131622694,
0.92388998734174,1.00001131622694,0.92388998734174,1.00001131622694,0.92388998734174,
1.00001131622694,0.92388998734174,1.00001131622694,0.92388998734174,1.00001131622694,
0.92388998734174,1.00001131622694,0.92388998734174,1.00001131622694,0.92388998734174,
1.00001131622694,0.92388998734174,1.00001131622694,0.92388998734174,1.00001131622694,
0.92388998734174,1.00001131622694,0.92388998734174,1.00001131622694,0.92388998734174,
1.00001131622694,0.92388998734174,1.00001131622694,0.92388998734174,1.00001131622694,
0.92388998734174,1.00001131622694,0.92388998734174,1.00001131622694,0.92388998734174,
1.00001131622694,0.92388998734174,1.00001131622694,0.92388998734174,1.00001131622694,
0.906316346597157,1.04327282413707)))
REPRESENTATION_ITEM('')
SURFACE()
);
#561=(
BOUNDED_SURFACE()
B_SPLINE_SURFACE(3,2,((#22076,#22077,#22078,#22079,#22080,#22081,#22082,
#22083,#22084,#22085,#22086,#22087,#22088,#22089,#22090,#22091,#22092,#22093,
#22094,#22095,#22096,#22097,#22098,#22099,#22100,#22101,#22102,#22103,#22104,
#22105,#22106,#22107,#22108,#22109,#22110,#22111,#22112,#22113,#22114,#22115,
#22116,#22117,#22118,#22119,#22120,#22121,#22122,#22123,#22124,#22125,#22126,
#22127,#22128,#22129,#22130,#22131,#22132,#22133,#22134,#22135,#22136,#22137,
#22138,#22139,#22140,#22141,#22142,#22143,#22144,#22145,#22146,#22147,#22148,
#22149,#22150,#22151,#22152,#22153,#22154,#22155,#22156,#22157,#22158,#22159,
#22160,#22161,#22162,#22163,#22164,#22165,#22166,#22167,#22168,#22169,#22170,
#22171,#22172,#22173,#22174,#22175,#22176,#22177,#22178,#22179,#22180,#22181,
#22182,#22183,#22184,#22185,#22186,#22187,#22188,#22189,#22190,#22191,#22192,
#22193,#22194,#22195,#22196,#22197,#22198,#22199,#22200,#22201,#22202,#22203,
#22204,#22205,#22206,#22207,#22208,#22209,#22210,#22211,#22212,#22213,#22214,
#22215,#22216,#22217,#22218,#22219,#22220,#22221,#22222,#22223,#22224,#22225,
#22226,#22227,#22228,#22229,#22230,#22231,#22232,#22233,#22234,#22235,#22236),
(#22237,#22238,#22239,#22240,#22241,#22242,#22243,#22244,#22245,#22246,
#22247,#22248,#22249,#22250,#22251,#22252,#22253,#22254,#22255,#22256,#22257,
#22258,#22259,#22260,#22261,#22262,#22263,#22264,#22265,#22266,#22267,#22268,
#22269,#22270,#22271,#22272,#22273,#22274,#22275,#22276,#22277,#22278,#22279,
#22280,#22281,#22282,#22283,#22284,#22285,#22286,#22287,#22288,#22289,#22290,
#22291,#22292,#22293,#22294,#22295,#22296,#22297,#22298,#22299,#22300,#22301,
#22302,#22303,#22304,#22305,#22306,#22307,#22308,#22309,#22310,#22311,#22312,
#22313,#22314,#22315,#22316,#22317,#22318,#22319,#22320,#22321,#22322,#22323,
#22324,#22325,#22326,#22327,#22328,#22329,#22330,#22331,#22332,#22333,#22334,
#22335,#22336,#22337,#22338,#22339,#22340,#22341,#22342,#22343,#22344,#22345,
#22346,#22347,#22348,#22349,#22350,#22351,#22352,#22353,#22354,#22355,#22356,
#22357,#22358,#22359,#22360,#22361,#22362,#22363,#22364,#22365,#22366,#22367,
#22368,#22369,#22370,#22371,#22372,#22373,#22374,#22375,#22376,#22377,#22378,
#22379,#22380,#22381,#22382,#22383,#22384,#22385,#22386,#22387,#22388,#22389,
#22390,#22391,#22392,#22393,#22394,#22395,#22396,#22397),(#22398,#22399,
#22400,#22401,#22402,#22403,#22404,#22405,#22406,#22407,#22408,#22409,#22410,
#22411,#22412,#22413,#22414,#22415,#22416,#22417,#22418,#22419,#22420,#22421,
#22422,#22423,#22424,#22425,#22426,#22427,#22428,#22429,#22430,#22431,#22432,
#22433,#22434,#22435,#22436,#22437,#22438,#22439,#22440,#22441,#22442,#22443,
#22444,#22445,#22446,#22447,#22448,#22449,#22450,#22451,#22452,#22453,#22454,
#22455,#22456,#22457,#22458,#22459,#22460,#22461,#22462,#22463,#22464,#22465,
#22466,#22467,#22468,#22469,#22470,#22471,#22472,#22473,#22474,#22475,#22476,
#22477,#22478,#22479,#22480,#22481,#22482,#22483,#22484,#22485,#22486,#22487,
#22488,#22489,#22490,#22491,#22492,#22493,#22494,#22495,#22496,#22497,#22498,
#22499,#22500,#22501,#22502,#22503,#22504,#22505,#22506,#22507,#22508,#22509,
#22510,#22511,#22512,#22513,#22514,#22515,#22516,#22517,#22518,#22519,#22520,
#22521,#22522,#22523,#22524,#22525,#22526,#22527,#22528,#22529,#22530,#22531,
#22532,#22533,#22534,#22535,#22536,#22537,#22538,#22539,#22540,#22541,#22542,
#22543,#22544,#22545,#22546,#22547,#22548,#22549,#22550,#22551,#22552,#22553,
#22554,#22555,#22556,#22557,#22558),(#22559,#22560,#22561,#22562,#22563,
#22564,#22565,#22566,#22567,#22568,#22569,#22570,#22571,#22572,#22573,#22574,
#22575,#22576,#22577,#22578,#22579,#22580,#22581,#22582,#22583,#22584,#22585,
#22586,#22587,#22588,#22589,#22590,#22591,#22592,#22593,#22594,#22595,#22596,
#22597,#22598,#22599,#22600,#22601,#22602,#22603,#22604,#22605,#22606,#22607,
#22608,#22609,#22610,#22611,#22612,#22613,#22614,#22615,#22616,#22617,#22618,
#22619,#22620,#22621,#22622,#22623,#22624,#22625,#22626,#22627,#22628,#22629,
#22630,#22631,#22632,#22633,#22634,#22635,#22636,#22637,#22638,#22639,#22640,
#22641,#22642,#22643,#22644,#22645,#22646,#22647,#22648,#22649,#22650,#22651,
#22652,#22653,#22654,#22655,#22656,#22657,#22658,#22659,#22660,#22661,#22662,
#22663,#22664,#22665,#22666,#22667,#22668,#22669,#22670,#22671,#22672,#22673,
#22674,#22675,#22676,#22677,#22678,#22679,#22680,#22681,#22682,#22683,#22684,
#22685,#22686,#22687,#22688,#22689,#22690,#22691,#22692,#22693,#22694,#22695,
#22696,#22697,#22698,#22699,#22700,#22701,#22702,#22703,#22704,#22705,#22706,
#22707,#22708,#22709,#22710,#22711,#22712,#22713,#22714,#22715,#22716,#22717,
#22718,#22719)),.UNSPECIFIED.,.F.,.F.,.F.)
B_SPLINE_SURFACE_WITH_KNOTS((4,4),(3,2,2,2,2,2,2,2,2,2,2,2,2,2,2,2,2,2,
2,2,2,2,2,2,2,2,2,2,2,2,2,2,2,2,2,2,2,2,2,2,2,2,2,2,2,2,2,2,2,2,2,2,2,2,
2,2,2,2,2,2,2,2,2,2,2,2,2,2,2,2,2,2,2,2,2,2,2,2,2,2,3),(0.,1.),(0.,0.0125,
0.025,0.0375,0.05,0.0625,0.075,0.0875,0.1,0.1125,0.125,0.1375,0.15,0.1625,
0.175,0.1875,0.2,0.2125,0.225,0.2375,0.25,0.2625,0.275,0.2875,0.3,0.3125,
0.325,0.3375,0.35,0.3625,0.375,0.3875,0.4,0.4125,0.425,0.4375,0.45,0.4625,
0.475,0.4875,0.5,0.5125,0.525,0.5375,0.55,0.5625,0.575,0.5875,0.6,0.6125,
0.625,0.6375,0.65,0.6625,0.675,0.6875,0.7,0.7125,0.725,0.7375,0.75,0.7625,
0.775,0.7875,0.8,0.8125,0.825,0.8375,0.85,0.8625,0.875,0.8875,0.9,0.9125,
0.925,0.9375,0.95,0.9625,0.975,0.9875,1.),.UNSPECIFIED.)
GEOMETRIC_REPRESENTATION_ITEM()
RATIONAL_B_SPLINE_SURFACE(((1.,0.923879532511287,1.,0.923879532511287,1.,
0.923879532511287,1.,0.923879532511287,1.,0.923879532511287,1.,0.923879532511287,
1.,0.923879532511287,1.,0.923879532511287,1.,0.923879532511287,1.,0.923879532511287,
1.,0.923879532511287,1.,0.923879532511287,1.,0.923879532511287,1.,0.923879532511287,
1.,0.923879532511287,1.,0.923879532511287,1.,0.923879532511287,1.,0.923879532511287,
1.,0.923879532511287,1.,0.923879532511287,1.,0.923879532511287,1.,0.923879532511287,
1.,0.923879532511287,1.,0.923879532511287,1.,0.923879532511287,1.,0.923879532511287,
1.,0.923879532511287,1.,0.923879532511287,1.,0.923879532511287,1.,0.923879532511287,
1.,0.923879532511287,1.,0.923879532511287,1.,0.923879532511287,1.,0.923879532511287,
1.,0.923879532511287,1.,0.923879532511287,1.,0.923879532511287,1.,0.923879532511287,
1.,0.923879532511287,1.,0.923879532511287,1.,0.923879532511287,1.,0.923879532511287,
1.,0.923879532511287,1.,0.923879532511287,1.,0.923879532511287,1.,0.923879532511287,
1.,0.923879532511287,1.,0.923879532511287,1.,0.923879532511287,1.,0.923879532511287,
1.,0.923879532511287,1.,0.923879532511287,1.,0.923879532511287,1.,0.923879532511287,
1.,0.923879532511287,1.,0.923879532511287,1.,0.923879532511287,1.,0.923879532511287,
1.,0.923879532511287,1.,0.923879532511287,1.,0.923879532511287,1.,0.923879532511287,
1.,0.923879532511287,1.,0.923879532511287,1.,0.923879532511287,1.,0.923879532511287,
1.,0.923879532511287,1.,0.923879532511287,1.,0.923879532511287,1.,0.923879532511287,
1.,0.923879532511287,1.,0.923879532511287,1.,0.923879532511287,1.,0.923879532511287,
1.,0.923879532511287,1.,0.923879532511287,1.,0.923879532511287,1.,0.923879532511287,
1.,0.923879532511287,1.,0.923879532511287,1.),(0.998696642611305,0.922675387296324,
0.998696642611305,0.922675387296324,0.998696642611305,0.922675387296324,
0.998696642611305,0.922675387296324,0.998696642611305,0.922675387296324,
0.998696642611305,0.922675387296324,0.998696642611305,0.922675387296324,
0.998696642611305,0.922675387296324,0.998696642611305,0.922675387296324,
0.998696642611305,0.922675387296324,0.998696642611305,0.922675387296324,
0.998696642611305,0.922675387296324,0.998696642611305,0.922675387296324,
0.998696642611305,0.922675387296324,0.998696642611305,0.922675387296324,
0.998696642611305,0.922675387296324,0.998696642611305,0.922675387296324,
0.998696642611305,0.922675387296324,0.998696642611305,0.922675387296324,
0.998696642611305,0.922675387296324,0.998696642611305,0.922675387296324,
0.998696642611305,0.922675387296324,0.998696642611305,0.922675387296324,
0.998696642611305,0.922675387296324,0.998696642611305,0.922675387296324,
0.998696642611305,0.922675387296324,0.998696642611305,0.922675387296324,
0.998696642611305,0.922675387296324,0.998696642611305,0.922675387296324,
0.998696642611305,0.922675387296324,0.998696642611305,0.922675387296324,
0.998696642611305,0.922675387296324,0.998696642611305,0.922675387296324,
0.998696642611305,0.922675387296324,0.998696642611305,0.922675387296324,
0.998696642611305,0.922675387296324,0.998696642611305,0.922675387296324,
0.998696642611305,0.922675387296324,0.998696642611305,0.922675387296324,
0.998696642611305,0.922675387296324,0.998696642611305,0.922675387296324,
0.998696642611305,0.922675387296324,0.998696642611305,0.922675387296324,
0.998696642611305,0.922675387296324,0.998696642611305,0.922675387296324,
0.998696642611305,0.922675387296324,0.998696642611305,0.922675387296324,
0.998696642611305,0.922675387296324,0.998696642611305,0.922675387296324,
0.998696642611305,0.922675387296324,0.998696642611305,0.922675387296324,
0.998696642611305,0.922675387296324,0.998696642611305,0.922675387296324,
0.998696642611305,0.922675387296324,0.998696642611305,0.922675387296324,
0.998696642611305,0.922675387296324,0.998696642611305,0.922675387296324,
0.998696642611305,0.922675387296324,0.998696642611305,0.922675387296324,
0.998696642611305,0.922675387296324,0.998696642611305,0.922675387296324,
0.998696642611305,0.922675387296324,0.998696642611305,0.922675387296324,
0.998696642611305,0.922675387296324,0.998696642611305,0.922675387296324,
0.998696642611305,0.922675387296324,0.998696642611305,0.922675387296324,
0.998696642611305,0.922675387296324,0.998696642611305,0.922675387296324,
0.998696642611305,0.922675387296324,0.998696642611305,0.922675387296324,
0.998696642611305,0.922675387296324,0.998696642611305,0.922675387296324,
0.998696642611305,0.922675387296324,0.998696642611305,0.922675387296324,
0.998696642611305,0.922675387296324,0.998696642611305,0.922675387296324,
0.998696642611305,0.922675387296324,0.998696642611305,0.922675387296324,
0.998696642611305,0.922675387296324,0.998696642611305),(0.998696642611305,
0.922675387296324,0.998696642611305,0.922675387296324,0.998696642611305,
0.922675387296324,0.998696642611305,0.922675387296324,0.998696642611305,
0.922675387296324,0.998696642611305,0.922675387296324,0.998696642611305,
0.922675387296324,0.998696642611305,0.922675387296324,0.998696642611305,
0.922675387296324,0.998696642611305,0.922675387296324,0.998696642611305,
0.922675387296324,0.998696642611305,0.922675387296324,0.998696642611305,
0.922675387296324,0.998696642611305,0.922675387296324,0.998696642611305,
0.922675387296324,0.998696642611305,0.922675387296324,0.998696642611305,
0.922675387296324,0.998696642611305,0.922675387296324,0.998696642611305,
0.922675387296324,0.998696642611305,0.922675387296324,0.998696642611305,
0.922675387296324,0.998696642611305,0.922675387296324,0.998696642611305,
0.922675387296324,0.998696642611305,0.922675387296324,0.998696642611305,
0.922675387296324,0.998696642611305,0.922675387296324,0.998696642611305,
0.922675387296324,0.998696642611305,0.922675387296324,0.998696642611305,
0.922675387296324,0.998696642611305,0.922675387296324,0.998696642611305,
0.922675387296324,0.998696642611305,0.922675387296324,0.998696642611305,
0.922675387296324,0.998696642611305,0.922675387296324,0.998696642611305,
0.922675387296324,0.998696642611305,0.922675387296324,0.998696642611305,
0.922675387296324,0.998696642611305,0.922675387296324,0.998696642611305,
0.922675387296324,0.998696642611305,0.922675387296324,0.998696642611305,
0.922675387296324,0.998696642611305,0.922675387296324,0.998696642611305,
0.922675387296324,0.998696642611305,0.922675387296324,0.998696642611305,
0.922675387296324,0.998696642611305,0.922675387296324,0.998696642611305,
0.922675387296324,0.998696642611305,0.922675387296324,0.998696642611305,
0.922675387296324,0.998696642611305,0.922675387296324,0.998696642611305,
0.922675387296324,0.998696642611305,0.922675387296324,0.998696642611305,
0.922675387296324,0.998696642611305,0.922675387296324,0.998696642611305,
0.922675387296324,0.998696642611305,0.922675387296324,0.998696642611305,
0.922675387296324,0.998696642611305,0.922675387296324,0.998696642611305,
0.922675387296324,0.998696642611305,0.922675387296324,0.998696642611305,
0.922675387296324,0.998696642611305,0.922675387296324,0.998696642611305,
0.922675387296324,0.998696642611305,0.922675387296324,0.998696642611305,
0.922675387296324,0.998696642611305,0.922675387296324,0.998696642611305,
0.922675387296324,0.998696642611305,0.922675387296324,0.998696642611305,
0.922675387296324,0.998696642611305,0.922675387296324,0.998696642611305,
0.922675387296324,0.998696642611305,0.922675387296324,0.998696642611305,
0.922675387296324,0.998696642611305,0.922675387296324,0.998696642611305,
0.922675387296324,0.998696642611305,0.922675387296324,0.998696642611305,
0.922675387296324,0.998696642611305,0.922675387296324,0.998696642611305,
0.922675387296324,0.998696642611305,0.922675387296324,0.998696642611305),
(1.,0.923879532511287,1.,0.923879532511287,1.,0.923879532511287,1.,0.923879532511287,
1.,0.923879532511287,1.,0.923879532511287,1.,0.923879532511287,1.,0.923879532511287,
1.,0.923879532511287,1.,0.923879532511287,1.,0.923879532511287,1.,0.923879532511287,
1.,0.923879532511287,1.,0.923879532511287,1.,0.923879532511287,1.,0.923879532511287,
1.,0.923879532511287,1.,0.923879532511287,1.,0.923879532511287,1.,0.923879532511287,
1.,0.923879532511287,1.,0.923879532511287,1.,0.923879532511287,1.,0.923879532511287,
1.,0.923879532511287,1.,0.923879532511287,1.,0.923879532511287,1.,0.923879532511287,
1.,0.923879532511287,1.,0.923879532511287,1.,0.923879532511287,1.,0.923879532511287,
1.,0.923879532511287,1.,0.923879532511287,1.,0.923879532511287,1.,0.923879532511287,
1.,0.923879532511287,1.,0.923879532511287,1.,0.923879532511287,1.,0.923879532511287,
1.,0.923879532511287,1.,0.923879532511287,1.,0.923879532511287,1.,0.923879532511287,
1.,0.923879532511287,1.,0.923879532511287,1.,0.923879532511287,1.,0.923879532511287,
1.,0.923879532511287,1.,0.923879532511287,1.,0.923879532511287,1.,0.923879532511287,
1.,0.923879532511287,1.,0.923879532511287,1.,0.923879532511287,1.,0.923879532511287,
1.,0.923879532511287,1.,0.923879532511287,1.,0.923879532511287,1.,0.923879532511287,
1.,0.923879532511287,1.,0.923879532511287,1.,0.923879532511287,1.,0.923879532511287,
1.,0.923879532511287,1.,0.923879532511287,1.,0.923879532511287,1.,0.923879532511287,
1.,0.923879532511287,1.,0.923879532511287,1.,0.923879532511287,1.,0.923879532511287,
1.,0.923879532511287,1.,0.923879532511287,1.,0.923879532511287,1.,0.923879532511287,
1.,0.923879532511287,1.,0.923879532511287,1.,0.923879532511287,1.,0.923879532511287,
1.)))
REPRESENTATION_ITEM('')
SURFACE()
);
#562=(
BOUNDED_SURFACE()
B_SPLINE_SURFACE(3,2,((#22720,#22721,#22722,#22723,#22724,#22725,#22726,
#22727,#22728,#22729,#22730,#22731,#22732,#22733,#22734,#22735,#22736,#22737,
#22738,#22739,#22740,#22741,#22742,#22743,#22744,#22745,#22746,#22747,#22748,
#22749,#22750,#22751,#22752,#22753,#22754,#22755,#22756,#22757,#22758,#22759,
#22760,#22761,#22762,#22763,#22764,#22765,#22766,#22767,#22768,#22769,#22770,
#22771,#22772,#22773,#22774,#22775,#22776,#22777,#22778,#22779,#22780,#22781,
#22782,#22783,#22784,#22785,#22786,#22787,#22788,#22789,#22790,#22791,#22792,
#22793,#22794,#22795,#22796,#22797,#22798,#22799,#22800,#22801,#22802,#22803,
#22804,#22805,#22806,#22807,#22808,#22809,#22810,#22811,#22812,#22813,#22814,
#22815,#22816,#22817,#22818,#22819,#22820,#22821,#22822,#22823,#22824,#22825,
#22826,#22827,#22828,#22829,#22830,#22831,#22832,#22833,#22834,#22835,#22836,
#22837,#22838,#22839,#22840,#22841,#22842,#22843,#22844,#22845,#22846,#22847,
#22848,#22849,#22850,#22851,#22852,#22853,#22854,#22855,#22856,#22857,#22858,
#22859,#22860,#22861,#22862,#22863,#22864,#22865,#22866,#22867,#22868,#22869,
#22870,#22871,#22872,#22873,#22874,#22875,#22876,#22877,#22878,#22879,#22880),
(#22881,#22882,#22883,#22884,#22885,#22886,#22887,#22888,#22889,#22890,
#22891,#22892,#22893,#22894,#22895,#22896,#22897,#22898,#22899,#22900,#22901,
#22902,#22903,#22904,#22905,#22906,#22907,#22908,#22909,#22910,#22911,#22912,
#22913,#22914,#22915,#22916,#22917,#22918,#22919,#22920,#22921,#22922,#22923,
#22924,#22925,#22926,#22927,#22928,#22929,#22930,#22931,#22932,#22933,#22934,
#22935,#22936,#22937,#22938,#22939,#22940,#22941,#22942,#22943,#22944,#22945,
#22946,#22947,#22948,#22949,#22950,#22951,#22952,#22953,#22954,#22955,#22956,
#22957,#22958,#22959,#22960,#22961,#22962,#22963,#22964,#22965,#22966,#22967,
#22968,#22969,#22970,#22971,#22972,#22973,#22974,#22975,#22976,#22977,#22978,
#22979,#22980,#22981,#22982,#22983,#22984,#22985,#22986,#22987,#22988,#22989,
#22990,#22991,#22992,#22993,#22994,#22995,#22996,#22997,#22998,#22999,#23000,
#23001,#23002,#23003,#23004,#23005,#23006,#23007,#23008,#23009,#23010,#23011,
#23012,#23013,#23014,#23015,#23016,#23017,#23018,#23019,#23020,#23021,#23022,
#23023,#23024,#23025,#23026,#23027,#23028,#23029,#23030,#23031,#23032,#23033,
#23034,#23035,#23036,#23037,#23038,#23039,#23040,#23041),(#23042,#23043,
#23044,#23045,#23046,#23047,#23048,#23049,#23050,#23051,#23052,#23053,#23054,
#23055,#23056,#23057,#23058,#23059,#23060,#23061,#23062,#23063,#23064,#23065,
#23066,#23067,#23068,#23069,#23070,#23071,#23072,#23073,#23074,#23075,#23076,
#23077,#23078,#23079,#23080,#23081,#23082,#23083,#23084,#23085,#23086,#23087,
#23088,#23089,#23090,#23091,#23092,#23093,#23094,#23095,#23096,#23097,#23098,
#23099,#23100,#23101,#23102,#23103,#23104,#23105,#23106,#23107,#23108,#23109,
#23110,#23111,#23112,#23113,#23114,#23115,#23116,#23117,#23118,#23119,#23120,
#23121,#23122,#23123,#23124,#23125,#23126,#23127,#23128,#23129,#23130,#23131,
#23132,#23133,#23134,#23135,#23136,#23137,#23138,#23139,#23140,#23141,#23142,
#23143,#23144,#23145,#23146,#23147,#23148,#23149,#23150,#23151,#23152,#23153,
#23154,#23155,#23156,#23157,#23158,#23159,#23160,#23161,#23162,#23163,#23164,
#23165,#23166,#23167,#23168,#23169,#23170,#23171,#23172,#23173,#23174,#23175,
#23176,#23177,#23178,#23179,#23180,#23181,#23182,#23183,#23184,#23185,#23186,
#23187,#23188,#23189,#23190,#23191,#23192,#23193,#23194,#23195,#23196,#23197,
#23198,#23199,#23200,#23201,#23202),(#23203,#23204,#23205,#23206,#23207,
#23208,#23209,#23210,#23211,#23212,#23213,#23214,#23215,#23216,#23217,#23218,
#23219,#23220,#23221,#23222,#23223,#23224,#23225,#23226,#23227,#23228,#23229,
#23230,#23231,#23232,#23233,#23234,#23235,#23236,#23237,#23238,#23239,#23240,
#23241,#23242,#23243,#23244,#23245,#23246,#23247,#23248,#23249,#23250,#23251,
#23252,#23253,#23254,#23255,#23256,#23257,#23258,#23259,#23260,#23261,#23262,
#23263,#23264,#23265,#23266,#23267,#23268,#23269,#23270,#23271,#23272,#23273,
#23274,#23275,#23276,#23277,#23278,#23279,#23280,#23281,#23282,#23283,#23284,
#23285,#23286,#23287,#23288,#23289,#23290,#23291,#23292,#23293,#23294,#23295,
#23296,#23297,#23298,#23299,#23300,#23301,#23302,#23303,#23304,#23305,#23306,
#23307,#23308,#23309,#23310,#23311,#23312,#23313,#23314,#23315,#23316,#23317,
#23318,#23319,#23320,#23321,#23322,#23323,#23324,#23325,#23326,#23327,#23328,
#23329,#23330,#23331,#23332,#23333,#23334,#23335,#23336,#23337,#23338,#23339,
#23340,#23341,#23342,#23343,#23344,#23345,#23346,#23347,#23348,#23349,#23350,
#23351,#23352,#23353,#23354,#23355,#23356,#23357,#23358,#23359,#23360,#23361,
#23362,#23363)),.UNSPECIFIED.,.F.,.F.,.F.)
B_SPLINE_SURFACE_WITH_KNOTS((4,4),(3,2,2,2,2,2,2,2,2,2,2,2,2,2,2,2,2,2,
2,2,2,2,2,2,2,2,2,2,2,2,2,2,2,2,2,2,2,2,2,2,2,2,2,2,2,2,2,2,2,2,2,2,2,2,
2,2,2,2,2,2,2,2,2,2,2,2,2,2,2,2,2,2,2,2,2,2,2,2,2,2,3),(0.,1.),(0.,0.0125,
0.025,0.0375,0.05,0.0625,0.075,0.0875,0.1,0.1125,0.125,0.1375,0.15,0.1625,
0.175,0.1875,0.2,0.2125,0.225,0.2375,0.25,0.2625,0.275,0.2875,0.3,0.3125,
0.325,0.3375,0.35,0.3625,0.375,0.3875,0.4,0.4125,0.425,0.4375,0.45,0.4625,
0.475,0.4875,0.5,0.5125,0.525,0.5375,0.55,0.5625,0.575,0.5875,0.6,0.6125,
0.625,0.6375,0.65,0.6625,0.675,0.6875,0.7,0.7125,0.725,0.7375,0.75,0.7625,
0.775,0.7875,0.8,0.8125,0.825,0.8375,0.85,0.8625,0.875,0.8875,0.9,0.9125,
0.925,0.9375,0.95,0.9625,0.975,0.9875,1.),.UNSPECIFIED.)
GEOMETRIC_REPRESENTATION_ITEM()
RATIONAL_B_SPLINE_SURFACE(((1.,0.923879532511287,1.,0.923879532511287,1.,
0.923879532511287,1.,0.923879532511287,1.,0.923879532511287,1.,0.923879532511287,
1.,0.923879532511287,1.,0.923879532511287,1.,0.923879532511287,1.,0.923879532511287,
1.,0.923879532511287,1.,0.923879532511287,1.,0.923879532511287,1.,0.923879532511287,
1.,0.923879532511287,1.,0.923879532511287,1.,0.923879532511287,1.,0.923879532511287,
1.,0.923879532511287,1.,0.923879532511287,1.,0.923879532511287,1.,0.923879532511287,
1.,0.923879532511287,1.,0.923879532511287,1.,0.923879532511287,1.,0.923879532511287,
1.,0.923879532511287,1.,0.923879532511287,1.,0.923879532511287,1.,0.923879532511287,
1.,0.923879532511287,1.,0.923879532511287,1.,0.923879532511287,1.,0.923879532511287,
1.,0.923879532511287,1.,0.923879532511287,1.,0.923879532511287,1.,0.923879532511287,
1.,0.923879532511287,1.,0.923879532511287,1.,0.923879532511287,1.,0.923879532511287,
1.,0.923879532511287,1.,0.923879532511287,1.,0.923879532511287,1.,0.923879532511287,
1.,0.923879532511287,1.,0.923879532511287,1.,0.923879532511287,1.,0.923879532511287,
1.,0.923879532511287,1.,0.923879532511287,1.,0.923879532511287,1.,0.923879532511287,
1.,0.923879532511287,1.,0.923879532511287,1.,0.923879532511287,1.,0.923879532511287,
1.,0.923879532511287,1.,0.923879532511287,1.,0.923879532511287,1.,0.923879532511287,
1.,0.923879532511287,1.,0.923879532511287,1.,0.923879532511287,1.,0.923879532511287,
1.,0.923879532511287,1.,0.923879532511287,1.,0.923879532511287,1.,0.923879532511287,
1.,0.923879532511287,1.,0.923879532511287,1.,0.923879532511287,1.,0.923879532511287,
1.,0.923879532511287,1.,0.923879532511287,1.,0.923879532511287,1.,0.923879532511287,
1.,0.923879532511287,1.,0.923879532511287,1.),(0.998696642611305,0.922675387296324,
0.998696642611305,0.922675387296324,0.998696642611305,0.922675387296324,
0.998696642611305,0.922675387296324,0.998696642611305,0.922675387296324,
0.998696642611305,0.922675387296324,0.998696642611305,0.922675387296324,
0.998696642611305,0.922675387296324,0.998696642611305,0.922675387296324,
0.998696642611305,0.922675387296324,0.998696642611305,0.922675387296324,
0.998696642611305,0.922675387296324,0.998696642611305,0.922675387296324,
0.998696642611305,0.922675387296324,0.998696642611305,0.922675387296324,
0.998696642611305,0.922675387296324,0.998696642611305,0.922675387296324,
0.998696642611305,0.922675387296324,0.998696642611305,0.922675387296324,
0.998696642611305,0.922675387296324,0.998696642611305,0.922675387296324,
0.998696642611305,0.922675387296324,0.998696642611305,0.922675387296324,
0.998696642611305,0.922675387296324,0.998696642611305,0.922675387296324,
0.998696642611305,0.922675387296324,0.998696642611305,0.922675387296324,
0.998696642611305,0.922675387296324,0.998696642611305,0.922675387296324,
0.998696642611305,0.922675387296324,0.998696642611305,0.922675387296324,
0.998696642611305,0.922675387296324,0.998696642611305,0.922675387296324,
0.998696642611305,0.922675387296324,0.998696642611305,0.922675387296324,
0.998696642611305,0.922675387296324,0.998696642611305,0.922675387296324,
0.998696642611305,0.922675387296324,0.998696642611305,0.922675387296324,
0.998696642611305,0.922675387296324,0.998696642611305,0.922675387296324,
0.998696642611305,0.922675387296324,0.998696642611305,0.922675387296324,
0.998696642611305,0.922675387296324,0.998696642611305,0.922675387296324,
0.998696642611305,0.922675387296324,0.998696642611305,0.922675387296324,
0.998696642611305,0.922675387296324,0.998696642611305,0.922675387296324,
0.998696642611305,0.922675387296324,0.998696642611305,0.922675387296324,
0.998696642611305,0.922675387296324,0.998696642611305,0.922675387296324,
0.998696642611305,0.922675387296324,0.998696642611305,0.922675387296324,
0.998696642611305,0.922675387296324,0.998696642611305,0.922675387296324,
0.998696642611305,0.922675387296324,0.998696642611305,0.922675387296324,
0.998696642611305,0.922675387296324,0.998696642611305,0.922675387296324,
0.998696642611305,0.922675387296324,0.998696642611305,0.922675387296324,
0.998696642611305,0.922675387296324,0.998696642611305,0.922675387296324,
0.998696642611305,0.922675387296324,0.998696642611305,0.922675387296324,
0.998696642611305,0.922675387296324,0.998696642611305,0.922675387296324,
0.998696642611305,0.922675387296324,0.998696642611305,0.922675387296324,
0.998696642611305,0.922675387296324,0.998696642611305,0.922675387296324,
0.998696642611305,0.922675387296324,0.998696642611305,0.922675387296324,
0.998696642611305,0.922675387296324,0.998696642611305,0.922675387296324,
0.998696642611305,0.922675387296324,0.998696642611305,0.922675387296324,
0.998696642611305,0.922675387296324,0.998696642611305),(0.998696642611305,
0.922675387296324,0.998696642611305,0.922675387296324,0.998696642611305,
0.922675387296324,0.998696642611305,0.922675387296324,0.998696642611305,
0.922675387296324,0.998696642611305,0.922675387296324,0.998696642611305,
0.922675387296324,0.998696642611305,0.922675387296324,0.998696642611305,
0.922675387296324,0.998696642611305,0.922675387296324,0.998696642611305,
0.922675387296324,0.998696642611305,0.922675387296324,0.998696642611305,
0.922675387296324,0.998696642611305,0.922675387296324,0.998696642611305,
0.922675387296324,0.998696642611305,0.922675387296324,0.998696642611305,
0.922675387296324,0.998696642611305,0.922675387296324,0.998696642611305,
0.922675387296324,0.998696642611305,0.922675387296324,0.998696642611305,
0.922675387296324,0.998696642611305,0.922675387296324,0.998696642611305,
0.922675387296324,0.998696642611305,0.922675387296324,0.998696642611305,
0.922675387296324,0.998696642611305,0.922675387296324,0.998696642611305,
0.922675387296324,0.998696642611305,0.922675387296324,0.998696642611305,
0.922675387296324,0.998696642611305,0.922675387296324,0.998696642611305,
0.922675387296324,0.998696642611305,0.922675387296324,0.998696642611305,
0.922675387296324,0.998696642611305,0.922675387296324,0.998696642611305,
0.922675387296324,0.998696642611305,0.922675387296324,0.998696642611305,
0.922675387296324,0.998696642611305,0.922675387296324,0.998696642611305,
0.922675387296324,0.998696642611305,0.922675387296324,0.998696642611305,
0.922675387296324,0.998696642611305,0.922675387296324,0.998696642611305,
0.922675387296324,0.998696642611305,0.922675387296324,0.998696642611305,
0.922675387296324,0.998696642611305,0.922675387296324,0.998696642611305,
0.922675387296324,0.998696642611305,0.922675387296324,0.998696642611305,
0.922675387296324,0.998696642611305,0.922675387296324,0.998696642611305,
0.922675387296324,0.998696642611305,0.922675387296324,0.998696642611305,
0.922675387296324,0.998696642611305,0.922675387296324,0.998696642611305,
0.922675387296324,0.998696642611305,0.922675387296324,0.998696642611305,
0.922675387296324,0.998696642611305,0.922675387296324,0.998696642611305,
0.922675387296324,0.998696642611305,0.922675387296324,0.998696642611305,
0.922675387296324,0.998696642611305,0.922675387296324,0.998696642611305,
0.922675387296324,0.998696642611305,0.922675387296324,0.998696642611305,
0.922675387296324,0.998696642611305,0.922675387296324,0.998696642611305,
0.922675387296324,0.998696642611305,0.922675387296324,0.998696642611305,
0.922675387296324,0.998696642611305,0.922675387296324,0.998696642611305,
0.922675387296324,0.998696642611305,0.922675387296324,0.998696642611305,
0.922675387296324,0.998696642611305,0.922675387296324,0.998696642611305,
0.922675387296324,0.998696642611305,0.922675387296324,0.998696642611305,
0.922675387296324,0.998696642611305,0.922675387296324,0.998696642611305,
0.922675387296324,0.998696642611305,0.922675387296324,0.998696642611305),
(1.,0.923879532511287,1.,0.923879532511287,1.,0.923879532511287,1.,0.923879532511287,
1.,0.923879532511287,1.,0.923879532511287,1.,0.923879532511287,1.,0.923879532511287,
1.,0.923879532511287,1.,0.923879532511287,1.,0.923879532511287,1.,0.923879532511287,
1.,0.923879532511287,1.,0.923879532511287,1.,0.923879532511287,1.,0.923879532511287,
1.,0.923879532511287,1.,0.923879532511287,1.,0.923879532511287,1.,0.923879532511287,
1.,0.923879532511287,1.,0.923879532511287,1.,0.923879532511287,1.,0.923879532511287,
1.,0.923879532511287,1.,0.923879532511287,1.,0.923879532511287,1.,0.923879532511287,
1.,0.923879532511287,1.,0.923879532511287,1.,0.923879532511287,1.,0.923879532511287,
1.,0.923879532511287,1.,0.923879532511287,1.,0.923879532511287,1.,0.923879532511287,
1.,0.923879532511287,1.,0.923879532511287,1.,0.923879532511287,1.,0.923879532511287,
1.,0.923879532511287,1.,0.923879532511287,1.,0.923879532511287,1.,0.923879532511287,
1.,0.923879532511287,1.,0.923879532511287,1.,0.923879532511287,1.,0.923879532511287,
1.,0.923879532511287,1.,0.923879532511287,1.,0.923879532511287,1.,0.923879532511287,
1.,0.923879532511287,1.,0.923879532511287,1.,0.923879532511287,1.,0.923879532511287,
1.,0.923879532511287,1.,0.923879532511287,1.,0.923879532511287,1.,0.923879532511287,
1.,0.923879532511287,1.,0.923879532511287,1.,0.923879532511287,1.,0.923879532511287,
1.,0.923879532511287,1.,0.923879532511287,1.,0.923879532511287,1.,0.923879532511287,
1.,0.923879532511287,1.,0.923879532511287,1.,0.923879532511287,1.,0.923879532511287,
1.,0.923879532511287,1.,0.923879532511287,1.,0.923879532511287,1.,0.923879532511287,
1.,0.923879532511287,1.,0.923879532511287,1.,0.923879532511287,1.,0.923879532511287,
1.)))
REPRESENTATION_ITEM('')
SURFACE()
);
#563=(
BOUNDED_SURFACE()
B_SPLINE_SURFACE(1,2,((#23364,#23365,#23366,#23367,#23368,#23369,#23370,
#23371,#23372,#23373,#23374,#23375,#23376,#23377,#23378,#23379,#23380,#23381,
#23382,#23383,#23384,#23385,#23386,#23387,#23388,#23389,#23390,#23391,#23392,
#23393,#23394,#23395,#23396,#23397,#23398,#23399,#23400,#23401,#23402,#23403,
#23404,#23405,#23406,#23407,#23408,#23409,#23410,#23411,#23412,#23413,#23414,
#23415,#23416,#23417,#23418,#23419,#23420,#23421,#23422,#23423,#23424,#23425,
#23426,#23427,#23428,#23429,#23430,#23431,#23432,#23433,#23434,#23435,#23436,
#23437,#23438,#23439,#23440,#23441,#23442,#23443,#23444,#23445,#23446,#23447,
#23448,#23449,#23450,#23451,#23452,#23453,#23454,#23455,#23456,#23457,#23458,
#23459,#23460,#23461,#23462,#23463,#23464,#23465,#23466,#23467,#23468,#23469,
#23470,#23471,#23472,#23473,#23474,#23475,#23476,#23477,#23478,#23479,#23480,
#23481,#23482,#23483,#23484,#23485,#23486,#23487,#23488,#23489,#23490,#23491,
#23492,#23493,#23494,#23495,#23496,#23497,#23498,#23499,#23500,#23501,#23502,
#23503,#23504,#23505,#23506,#23507,#23508,#23509,#23510,#23511,#23512,#23513,
#23514,#23515,#23516,#23517,#23518,#23519,#23520,#23521,#23522,#23523,#23524),
(#23525,#23526,#23527,#23528,#23529,#23530,#23531,#23532,#23533,#23534,
#23535,#23536,#23537,#23538,#23539,#23540,#23541,#23542,#23543,#23544,#23545,
#23546,#23547,#23548,#23549,#23550,#23551,#23552,#23553,#23554,#23555,#23556,
#23557,#23558,#23559,#23560,#23561,#23562,#23563,#23564,#23565,#23566,#23567,
#23568,#23569,#23570,#23571,#23572,#23573,#23574,#23575,#23576,#23577,#23578,
#23579,#23580,#23581,#23582,#23583,#23584,#23585,#23586,#23587,#23588,#23589,
#23590,#23591,#23592,#23593,#23594,#23595,#23596,#23597,#23598,#23599,#23600,
#23601,#23602,#23603,#23604,#23605,#23606,#23607,#23608,#23609,#23610,#23611,
#23612,#23613,#23614,#23615,#23616,#23617,#23618,#23619,#23620,#23621,#23622,
#23623,#23624,#23625,#23626,#23627,#23628,#23629,#23630,#23631,#23632,#23633,
#23634,#23635,#23636,#23637,#23638,#23639,#23640,#23641,#23642,#23643,#23644,
#23645,#23646,#23647,#23648,#23649,#23650,#23651,#23652,#23653,#23654,#23655,
#23656,#23657,#23658,#23659,#23660,#23661,#23662,#23663,#23664,#23665,#23666,
#23667,#23668,#23669,#23670,#23671,#23672,#23673,#23674,#23675,#23676,#23677,
#23678,#23679,#23680,#23681,#23682,#23683,#23684,#23685)),.UNSPECIFIED.,
 .F.,.F.,.F.)
B_SPLINE_SURFACE_WITH_KNOTS((2,2),(3,2,2,2,2,2,2,2,2,2,2,2,2,2,2,2,2,2,
2,2,2,2,2,2,2,2,2,2,2,2,2,2,2,2,2,2,2,2,2,2,2,2,2,2,2,2,2,2,2,2,2,2,2,2,
2,2,2,2,2,2,2,2,2,2,2,2,2,2,2,2,2,2,2,2,2,2,2,2,2,2,3),(0.,1.),(0.,0.0125,
0.025,0.0375,0.05,0.0625,0.075,0.0875,0.1,0.1125,0.125,0.1375,0.15,0.1625,
0.175,0.1875,0.2,0.2125,0.225,0.2375,0.25,0.2625,0.275,0.2875,0.3,0.3125,
0.325,0.3375,0.35,0.3625,0.375,0.3875,0.4,0.4125,0.425,0.4375,0.45,0.4625,
0.475,0.4875,0.5,0.5125,0.525,0.5375,0.55,0.5625,0.575,0.5875,0.6,0.6125,
0.625,0.6375,0.65,0.6625,0.675,0.6875,0.7,0.7125,0.725,0.7375,0.75,0.7625,
0.775,0.7875,0.8,0.8125,0.825,0.8375,0.85,0.8625,0.875,0.8875,0.9,0.9125,
0.925,0.9375,0.95,0.9625,0.975,0.9875,1.),.UNSPECIFIED.)
GEOMETRIC_REPRESENTATION_ITEM()
RATIONAL_B_SPLINE_SURFACE(((1.,0.923879532511287,1.,0.923879532511287,1.,
0.923879532511287,1.,0.923879532511287,1.,0.923879532511287,1.,0.923879532511287,
1.,0.923879532511287,1.,0.923879532511287,1.,0.923879532511287,1.,0.923879532511287,
1.,0.923879532511287,1.,0.923879532511287,1.,0.923879532511287,1.,0.923879532511287,
1.,0.923879532511287,1.,0.923879532511287,1.,0.923879532511287,1.,0.923879532511287,
1.,0.923879532511287,1.,0.923879532511287,1.,0.923879532511287,1.,0.923879532511287,
1.,0.923879532511287,1.,0.923879532511287,1.,0.923879532511287,1.,0.923879532511287,
1.,0.923879532511287,1.,0.923879532511287,1.,0.923879532511287,1.,0.923879532511287,
1.,0.923879532511287,1.,0.923879532511287,1.,0.923879532511287,1.,0.923879532511287,
1.,0.923879532511287,1.,0.923879532511287,1.,0.923879532511287,1.,0.923879532511287,
1.,0.923879532511287,1.,0.923879532511287,1.,0.923879532511287,1.,0.923879532511287,
1.,0.923879532511287,1.,0.923879532511287,1.,0.923879532511287,1.,0.923879532511287,
1.,0.923879532511287,1.,0.923879532511287,1.,0.923879532511287,1.,0.923879532511287,
1.,0.923879532511287,1.,0.923879532511287,1.,0.923879532511287,1.,0.923879532511287,
1.,0.923879532511287,1.,0.923879532511287,1.,0.923879532511287,1.,0.923879532511287,
1.,0.923879532511287,1.,0.923879532511287,1.,0.923879532511287,1.,0.923879532511287,
1.,0.923879532511287,1.,0.923879532511287,1.,0.923879532511287,1.,0.923879532511287,
1.,0.923879532511287,1.,0.923879532511287,1.,0.923879532511287,1.,0.923879532511287,
1.,0.923879532511287,1.,0.923879532511287,1.,0.923879532511287,1.,0.923879532511287,
1.,0.923879532511287,1.,0.923879532511287,1.,0.923879532511287,1.,0.923879532511287,
1.,0.923879532511287,1.,0.923879532511287,1.),(1.,0.923879532511287,1.,
0.923879532511287,1.,0.923879532511287,1.,0.923879532511287,1.,0.923879532511287,
1.,0.923879532511287,1.,0.923879532511287,1.,0.923879532511287,1.,0.923879532511287,
1.,0.923879532511287,1.,0.923879532511287,1.,0.923879532511287,1.,0.923879532511287,
1.,0.923879532511287,1.,0.923879532511287,1.,0.923879532511287,1.,0.923879532511287,
1.,0.923879532511287,1.,0.923879532511287,1.,0.923879532511287,1.,0.923879532511287,
1.,0.923879532511287,1.,0.923879532511287,1.,0.923879532511287,1.,0.923879532511287,
1.,0.923879532511287,1.,0.923879532511287,1.,0.923879532511287,1.,0.923879532511287,
1.,0.923879532511287,1.,0.923879532511287,1.,0.923879532511287,1.,0.923879532511287,
1.,0.923879532511287,1.,0.923879532511287,1.,0.923879532511287,1.,0.923879532511287,
1.,0.923879532511287,1.,0.923879532511287,1.,0.923879532511287,1.,0.923879532511287,
1.,0.923879532511287,1.,0.923879532511287,1.,0.923879532511287,1.,0.923879532511287,
1.,0.923879532511287,1.,0.923879532511287,1.,0.923879532511287,1.,0.923879532511287,
1.,0.923879532511287,1.,0.923879532511287,1.,0.923879532511287,1.,0.923879532511287,
1.,0.923879532511287,1.,0.923879532511287,1.,0.923879532511287,1.,0.923879532511287,
1.,0.923879532511287,1.,0.923879532511287,1.,0.923879532511287,1.,0.923879532511287,
1.,0.923879532511287,1.,0.923879532511287,1.,0.923879532511287,1.,0.923879532511287,
1.,0.923879532511287,1.,0.923879532511287,1.,0.923879532511287,1.,0.923879532511287,
1.,0.923879532511287,1.,0.923879532511287,1.,0.923879532511287,1.,0.923879532511287,
1.,0.923879532511287,1.,0.923879532511287,1.,0.923879532511287,1.,0.923879532511287,
1.,0.923879532511287,1.,0.923879532511287,1.,0.923879532511287,1.)))
REPRESENTATION_ITEM('')
SURFACE()
);
#564=(
BOUNDED_SURFACE()
B_SPLINE_SURFACE(1,2,((#23703,#23704,#23705,#23706,#23707,#23708,#23709,
#23710,#23711,#23712,#23713,#23714,#23715,#23716,#23717,#23718,#23719,#23720,
#23721,#23722,#23723,#23724,#23725,#23726,#23727,#23728,#23729,#23730,#23731,
#23732,#23733,#23734,#23735,#23736,#23737,#23738,#23739,#23740,#23741,#23742,
#23743,#23744,#23745,#23746,#23747,#23748,#23749,#23750,#23751,#23752,#23753,
#23754,#23755,#23756,#23757,#23758,#23759,#23760,#23761,#23762,#23763,#23764,
#23765,#23766,#23767,#23768,#23769,#23770,#23771,#23772,#23773,#23774,#23775,
#23776,#23777,#23778,#23779,#23780,#23781,#23782,#23783,#23784,#23785,#23786,
#23787,#23788,#23789,#23790,#23791,#23792,#23793,#23794,#23795,#23796,#23797,
#23798,#23799,#23800,#23801,#23802,#23803,#23804,#23805,#23806,#23807,#23808,
#23809,#23810,#23811,#23812,#23813,#23814,#23815,#23816,#23817,#23818,#23819,
#23820,#23821,#23822,#23823,#23824,#23825,#23826,#23827,#23828,#23829,#23830,
#23831,#23832,#23833,#23834,#23835,#23836,#23837,#23838,#23839,#23840,#23841,
#23842,#23843,#23844,#23845,#23846,#23847,#23848,#23849,#23850,#23851,#23852,
#23853,#23854,#23855,#23856,#23857,#23858,#23859,#23860,#23861,#23862,#23863),
(#23864,#23865,#23866,#23867,#23868,#23869,#23870,#23871,#23872,#23873,
#23874,#23875,#23876,#23877,#23878,#23879,#23880,#23881,#23882,#23883,#23884,
#23885,#23886,#23887,#23888,#23889,#23890,#23891,#23892,#23893,#23894,#23895,
#23896,#23897,#23898,#23899,#23900,#23901,#23902,#23903,#23904,#23905,#23906,
#23907,#23908,#23909,#23910,#23911,#23912,#23913,#23914,#23915,#23916,#23917,
#23918,#23919,#23920,#23921,#23922,#23923,#23924,#23925,#23926,#23927,#23928,
#23929,#23930,#23931,#23932,#23933,#23934,#23935,#23936,#23937,#23938,#23939,
#23940,#23941,#23942,#23943,#23944,#23945,#23946,#23947,#23948,#23949,#23950,
#23951,#23952,#23953,#23954,#23955,#23956,#23957,#23958,#23959,#23960,#23961,
#23962,#23963,#23964,#23965,#23966,#23967,#23968,#23969,#23970,#23971,#23972,
#23973,#23974,#23975,#23976,#23977,#23978,#23979,#23980,#23981,#23982,#23983,
#23984,#23985,#23986,#23987,#23988,#23989,#23990,#23991,#23992,#23993,#23994,
#23995,#23996,#23997,#23998,#23999,#24000,#24001,#24002,#24003,#24004,#24005,
#24006,#24007,#24008,#24009,#24010,#24011,#24012,#24013,#24014,#24015,#24016,
#24017,#24018,#24019,#24020,#24021,#24022,#24023,#24024)),.UNSPECIFIED.,
 .F.,.F.,.F.)
B_SPLINE_SURFACE_WITH_KNOTS((2,2),(3,2,2,2,2,2,2,2,2,2,2,2,2,2,2,2,2,2,
2,2,2,2,2,2,2,2,2,2,2,2,2,2,2,2,2,2,2,2,2,2,2,2,2,2,2,2,2,2,2,2,2,2,2,2,
2,2,2,2,2,2,2,2,2,2,2,2,2,2,2,2,2,2,2,2,2,2,2,2,2,2,3),(0.,1.),(0.,0.0125,
0.025,0.0375,0.05,0.0625,0.075,0.0875,0.1,0.1125,0.125,0.1375,0.15,0.1625,
0.175,0.1875,0.2,0.2125,0.225,0.2375,0.25,0.2625,0.275,0.2875,0.3,0.3125,
0.325,0.3375,0.35,0.3625,0.375,0.3875,0.4,0.4125,0.425,0.4375,0.45,0.4625,
0.475,0.4875,0.5,0.5125,0.525,0.5375,0.55,0.5625,0.575,0.5875,0.6,0.6125,
0.625,0.6375,0.65,0.6625,0.675,0.6875,0.7,0.7125,0.725,0.7375,0.75,0.7625,
0.775,0.7875,0.8,0.8125,0.825,0.8375,0.85,0.8625,0.875,0.8875,0.9,0.9125,
0.925,0.9375,0.95,0.9625,0.975,0.9875,1.),.UNSPECIFIED.)
GEOMETRIC_REPRESENTATION_ITEM()
RATIONAL_B_SPLINE_SURFACE(((1.,0.923879532511287,1.,0.923879532511287,1.,
0.923879532511287,1.,0.923879532511287,1.,0.923879532511287,1.,0.923879532511287,
1.,0.923879532511287,1.,0.923879532511287,1.,0.923879532511287,1.,0.923879532511287,
1.,0.923879532511287,1.,0.923879532511287,1.,0.923879532511287,1.,0.923879532511287,
1.,0.923879532511287,1.,0.923879532511287,1.,0.923879532511287,1.,0.923879532511287,
1.,0.923879532511287,1.,0.923879532511287,1.,0.923879532511287,1.,0.923879532511287,
1.,0.923879532511287,1.,0.923879532511287,1.,0.923879532511287,1.,0.923879532511287,
1.,0.923879532511287,1.,0.923879532511287,1.,0.923879532511287,1.,0.923879532511287,
1.,0.923879532511287,1.,0.923879532511287,1.,0.923879532511287,1.,0.923879532511287,
1.,0.923879532511287,1.,0.923879532511287,1.,0.923879532511287,1.,0.923879532511287,
1.,0.923879532511287,1.,0.923879532511287,1.,0.923879532511287,1.,0.923879532511287,
1.,0.923879532511287,1.,0.923879532511287,1.,0.923879532511287,1.,0.923879532511287,
1.,0.923879532511287,1.,0.923879532511287,1.,0.923879532511287,1.,0.923879532511287,
1.,0.923879532511287,1.,0.923879532511287,1.,0.923879532511287,1.,0.923879532511287,
1.,0.923879532511287,1.,0.923879532511287,1.,0.923879532511287,1.,0.923879532511287,
1.,0.923879532511287,1.,0.923879532511287,1.,0.923879532511287,1.,0.923879532511287,
1.,0.923879532511287,1.,0.923879532511287,1.,0.923879532511287,1.,0.923879532511287,
1.,0.923879532511287,1.,0.923879532511287,1.,0.923879532511287,1.,0.923879532511287,
1.,0.923879532511287,1.,0.923879532511287,1.,0.923879532511287,1.,0.923879532511287,
1.,0.923879532511287,1.,0.923879532511287,1.,0.923879532511287,1.,0.923879532511287,
1.,0.923879532511287,1.,0.923879532511287,1.),(1.,0.923879532511287,1.,
0.923879532511287,1.,0.923879532511287,1.,0.923879532511287,1.,0.923879532511287,
1.,0.923879532511287,1.,0.923879532511287,1.,0.923879532511287,1.,0.923879532511287,
1.,0.923879532511287,1.,0.923879532511287,1.,0.923879532511287,1.,0.923879532511287,
1.,0.923879532511287,1.,0.923879532511287,1.,0.923879532511287,1.,0.923879532511287,
1.,0.923879532511287,1.,0.923879532511287,1.,0.923879532511287,1.,0.923879532511287,
1.,0.923879532511287,1.,0.923879532511287,1.,0.923879532511287,1.,0.923879532511287,
1.,0.923879532511287,1.,0.923879532511287,1.,0.923879532511287,1.,0.923879532511287,
1.,0.923879532511287,1.,0.923879532511287,1.,0.923879532511287,1.,0.923879532511287,
1.,0.923879532511287,1.,0.923879532511287,1.,0.923879532511287,1.,0.923879532511287,
1.,0.923879532511287,1.,0.923879532511287,1.,0.923879532511287,1.,0.923879532511287,
1.,0.923879532511287,1.,0.923879532511287,1.,0.923879532511287,1.,0.923879532511287,
1.,0.923879532511287,1.,0.923879532511287,1.,0.923879532511287,1.,0.923879532511287,
1.,0.923879532511287,1.,0.923879532511287,1.,0.923879532511287,1.,0.923879532511287,
1.,0.923879532511287,1.,0.923879532511287,1.,0.923879532511287,1.,0.923879532511287,
1.,0.923879532511287,1.,0.923879532511287,1.,0.923879532511287,1.,0.923879532511287,
1.,0.923879532511287,1.,0.923879532511287,1.,0.923879532511287,1.,0.923879532511287,
1.,0.923879532511287,1.,0.923879532511287,1.,0.923879532511287,1.,0.923879532511287,
1.,0.923879532511287,1.,0.923879532511287,1.,0.923879532511287,1.,0.923879532511287,
1.,0.923879532511287,1.,0.923879532511287,1.,0.923879532511287,1.,0.923879532511287,
1.,0.923879532511287,1.,0.923879532511287,1.,0.923879532511287,1.)))
REPRESENTATION_ITEM('')
SURFACE()
);
#565=(
BOUNDED_SURFACE()
B_SPLINE_SURFACE(3,2,((#24040,#24041,#24042,#24043,#24044,#24045,#24046,
#24047,#24048,#24049,#24050,#24051,#24052,#24053,#24054,#24055,#24056,#24057,
#24058,#24059,#24060,#24061,#24062,#24063,#24064,#24065,#24066,#24067,#24068,
#24069,#24070,#24071,#24072,#24073,#24074,#24075,#24076,#24077,#24078,#24079,
#24080,#24081,#24082,#24083,#24084,#24085,#24086,#24087,#24088,#24089,#24090,
#24091,#24092,#24093,#24094,#24095,#24096,#24097,#24098,#24099,#24100,#24101,
#24102,#24103,#24104,#24105,#24106,#24107,#24108,#24109,#24110,#24111,#24112,
#24113,#24114,#24115,#24116,#24117,#24118,#24119,#24120,#24121,#24122,#24123,
#24124,#24125,#24126,#24127,#24128,#24129,#24130,#24131,#24132,#24133,#24134,
#24135,#24136,#24137,#24138,#24139,#24140,#24141,#24142,#24143,#24144,#24145,
#24146,#24147,#24148,#24149,#24150,#24151,#24152,#24153,#24154,#24155,#24156,
#24157,#24158,#24159,#24160,#24161,#24162,#24163,#24164,#24165,#24166,#24167,
#24168,#24169,#24170,#24171,#24172,#24173,#24174,#24175,#24176,#24177,#24178,
#24179,#24180,#24181,#24182,#24183,#24184,#24185,#24186,#24187,#24188,#24189,
#24190,#24191,#24192,#24193,#24194,#24195,#24196,#24197,#24198,#24199,#24200),
(#24201,#24202,#24203,#24204,#24205,#24206,#24207,#24208,#24209,#24210,
#24211,#24212,#24213,#24214,#24215,#24216,#24217,#24218,#24219,#24220,#24221,
#24222,#24223,#24224,#24225,#24226,#24227,#24228,#24229,#24230,#24231,#24232,
#24233,#24234,#24235,#24236,#24237,#24238,#24239,#24240,#24241,#24242,#24243,
#24244,#24245,#24246,#24247,#24248,#24249,#24250,#24251,#24252,#24253,#24254,
#24255,#24256,#24257,#24258,#24259,#24260,#24261,#24262,#24263,#24264,#24265,
#24266,#24267,#24268,#24269,#24270,#24271,#24272,#24273,#24274,#24275,#24276,
#24277,#24278,#24279,#24280,#24281,#24282,#24283,#24284,#24285,#24286,#24287,
#24288,#24289,#24290,#24291,#24292,#24293,#24294,#24295,#24296,#24297,#24298,
#24299,#24300,#24301,#24302,#24303,#24304,#24305,#24306,#24307,#24308,#24309,
#24310,#24311,#24312,#24313,#24314,#24315,#24316,#24317,#24318,#24319,#24320,
#24321,#24322,#24323,#24324,#24325,#24326,#24327,#24328,#24329,#24330,#24331,
#24332,#24333,#24334,#24335,#24336,#24337,#24338,#24339,#24340,#24341,#24342,
#24343,#24344,#24345,#24346,#24347,#24348,#24349,#24350,#24351,#24352,#24353,
#24354,#24355,#24356,#24357,#24358,#24359,#24360,#24361),(#24362,#24363,
#24364,#24365,#24366,#24367,#24368,#24369,#24370,#24371,#24372,#24373,#24374,
#24375,#24376,#24377,#24378,#24379,#24380,#24381,#24382,#24383,#24384,#24385,
#24386,#24387,#24388,#24389,#24390,#24391,#24392,#24393,#24394,#24395,#24396,
#24397,#24398,#24399,#24400,#24401,#24402,#24403,#24404,#24405,#24406,#24407,
#24408,#24409,#24410,#24411,#24412,#24413,#24414,#24415,#24416,#24417,#24418,
#24419,#24420,#24421,#24422,#24423,#24424,#24425,#24426,#24427,#24428,#24429,
#24430,#24431,#24432,#24433,#24434,#24435,#24436,#24437,#24438,#24439,#24440,
#24441,#24442,#24443,#24444,#24445,#24446,#24447,#24448,#24449,#24450,#24451,
#24452,#24453,#24454,#24455,#24456,#24457,#24458,#24459,#24460,#24461,#24462,
#24463,#24464,#24465,#24466,#24467,#24468,#24469,#24470,#24471,#24472,#24473,
#24474,#24475,#24476,#24477,#24478,#24479,#24480,#24481,#24482,#24483,#24484,
#24485,#24486,#24487,#24488,#24489,#24490,#24491,#24492,#24493,#24494,#24495,
#24496,#24497,#24498,#24499,#24500,#24501,#24502,#24503,#24504,#24505,#24506,
#24507,#24508,#24509,#24510,#24511,#24512,#24513,#24514,#24515,#24516,#24517,
#24518,#24519,#24520,#24521,#24522),(#24523,#24524,#24525,#24526,#24527,
#24528,#24529,#24530,#24531,#24532,#24533,#24534,#24535,#24536,#24537,#24538,
#24539,#24540,#24541,#24542,#24543,#24544,#24545,#24546,#24547,#24548,#24549,
#24550,#24551,#24552,#24553,#24554,#24555,#24556,#24557,#24558,#24559,#24560,
#24561,#24562,#24563,#24564,#24565,#24566,#24567,#24568,#24569,#24570,#24571,
#24572,#24573,#24574,#24575,#24576,#24577,#24578,#24579,#24580,#24581,#24582,
#24583,#24584,#24585,#24586,#24587,#24588,#24589,#24590,#24591,#24592,#24593,
#24594,#24595,#24596,#24597,#24598,#24599,#24600,#24601,#24602,#24603,#24604,
#24605,#24606,#24607,#24608,#24609,#24610,#24611,#24612,#24613,#24614,#24615,
#24616,#24617,#24618,#24619,#24620,#24621,#24622,#24623,#24624,#24625,#24626,
#24627,#24628,#24629,#24630,#24631,#24632,#24633,#24634,#24635,#24636,#24637,
#24638,#24639,#24640,#24641,#24642,#24643,#24644,#24645,#24646,#24647,#24648,
#24649,#24650,#24651,#24652,#24653,#24654,#24655,#24656,#24657,#24658,#24659,
#24660,#24661,#24662,#24663,#24664,#24665,#24666,#24667,#24668,#24669,#24670,
#24671,#24672,#24673,#24674,#24675,#24676,#24677,#24678,#24679,#24680,#24681,
#24682,#24683)),.UNSPECIFIED.,.F.,.F.,.F.)
B_SPLINE_SURFACE_WITH_KNOTS((4,4),(3,2,2,2,2,2,2,2,2,2,2,2,2,2,2,2,2,2,
2,2,2,2,2,2,2,2,2,2,2,2,2,2,2,2,2,2,2,2,2,2,2,2,2,2,2,2,2,2,2,2,2,2,2,2,
2,2,2,2,2,2,2,2,2,2,2,2,2,2,2,2,2,2,2,2,2,2,2,2,2,2,3),(0.,1.),(0.,0.0125,
0.025,0.0375,0.05,0.0625,0.075,0.0875,0.1,0.1125,0.125,0.1375,0.15,0.1625,
0.175,0.1875,0.2,0.2125,0.225,0.2375,0.25,0.2625,0.275,0.2875,0.3,0.3125,
0.325,0.3375,0.35,0.3625,0.375,0.3875,0.4,0.4125,0.425,0.4375,0.45,0.4625,
0.475,0.4875,0.5,0.5125,0.525,0.5375,0.55,0.5625,0.575,0.5875,0.6,0.6125,
0.625,0.6375,0.65,0.6625,0.675,0.6875,0.7,0.7125,0.725,0.7375,0.75,0.7625,
0.775,0.7875,0.8,0.8125,0.825,0.8375,0.85,0.8625,0.875,0.8875,0.9,0.9125,
0.925,0.9375,0.95,0.9625,0.975,0.9875,1.),.UNSPECIFIED.)
GEOMETRIC_REPRESENTATION_ITEM()
RATIONAL_B_SPLINE_SURFACE(((1.,0.923879532511287,1.,0.923879532511287,1.,
0.923879532511287,1.,0.923879532511287,1.,0.923879532511287,1.,0.923879532511287,
1.,0.923879532511287,1.,0.923879532511287,1.,0.923879532511287,1.,0.923879532511287,
1.,0.923879532511287,1.,0.923879532511287,1.,0.923879532511287,1.,0.923879532511287,
1.,0.923879532511287,1.,0.923879532511287,1.,0.923879532511287,1.,0.923879532511287,
1.,0.923879532511287,1.,0.923879532511287,1.,0.923879532511287,1.,0.923879532511287,
1.,0.923879532511287,1.,0.923879532511287,1.,0.923879532511287,1.,0.923879532511287,
1.,0.923879532511287,1.,0.923879532511287,1.,0.923879532511287,1.,0.923879532511287,
1.,0.923879532511287,1.,0.923879532511287,1.,0.923879532511287,1.,0.923879532511287,
1.,0.923879532511287,1.,0.923879532511287,1.,0.923879532511287,1.,0.923879532511287,
1.,0.923879532511287,1.,0.923879532511287,1.,0.923879532511287,1.,0.923879532511287,
1.,0.923879532511287,1.,0.923879532511287,1.,0.923879532511287,1.,0.923879532511287,
1.,0.923879532511287,1.,0.923879532511287,1.,0.923879532511287,1.,0.923879532511287,
1.,0.923879532511287,1.,0.923879532511287,1.,0.923879532511287,1.,0.923879532511287,
1.,0.923879532511287,1.,0.923879532511287,1.,0.923879532511287,1.,0.923879532511287,
1.,0.923879532511287,1.,0.923879532511287,1.,0.923879532511287,1.,0.923879532511287,
1.,0.923879532511287,1.,0.923879532511287,1.,0.923879532511287,1.,0.923879532511287,
1.,0.923879532511287,1.,0.923879532511287,1.,0.923879532511287,1.,0.923879532511287,
1.,0.923879532511287,1.,0.923879532511287,1.,0.923879532511287,1.,0.923879532511287,
1.,0.923879532511287,1.,0.923879532511287,1.,0.923879532511287,1.,0.923879532511287,
1.,0.923879532511287,1.,0.923879532511287,1.),(0.998696642611305,0.922675387296324,
0.998696642611305,0.922675387296324,0.998696642611305,0.922675387296324,
0.998696642611305,0.922675387296324,0.998696642611305,0.922675387296324,
0.998696642611305,0.922675387296324,0.998696642611305,0.922675387296324,
0.998696642611305,0.922675387296324,0.998696642611305,0.922675387296324,
0.998696642611305,0.922675387296324,0.998696642611305,0.922675387296324,
0.998696642611305,0.922675387296324,0.998696642611305,0.922675387296324,
0.998696642611305,0.922675387296324,0.998696642611305,0.922675387296324,
0.998696642611305,0.922675387296324,0.998696642611305,0.922675387296324,
0.998696642611305,0.922675387296324,0.998696642611305,0.922675387296324,
0.998696642611305,0.922675387296324,0.998696642611305,0.922675387296324,
0.998696642611305,0.922675387296324,0.998696642611305,0.922675387296324,
0.998696642611305,0.922675387296324,0.998696642611305,0.922675387296324,
0.998696642611305,0.922675387296324,0.998696642611305,0.922675387296324,
0.998696642611305,0.922675387296324,0.998696642611305,0.922675387296324,
0.998696642611305,0.922675387296324,0.998696642611305,0.922675387296324,
0.998696642611305,0.922675387296324,0.998696642611305,0.922675387296324,
0.998696642611305,0.922675387296324,0.998696642611305,0.922675387296324,
0.998696642611305,0.922675387296324,0.998696642611305,0.922675387296324,
0.998696642611305,0.922675387296324,0.998696642611305,0.922675387296324,
0.998696642611305,0.922675387296324,0.998696642611305,0.922675387296324,
0.998696642611305,0.922675387296324,0.998696642611305,0.922675387296324,
0.998696642611305,0.922675387296324,0.998696642611305,0.922675387296324,
0.998696642611305,0.922675387296324,0.998696642611305,0.922675387296324,
0.998696642611305,0.922675387296324,0.998696642611305,0.922675387296324,
0.998696642611305,0.922675387296324,0.998696642611305,0.922675387296324,
0.998696642611305,0.922675387296324,0.998696642611305,0.922675387296324,
0.998696642611305,0.922675387296324,0.998696642611305,0.922675387296324,
0.998696642611305,0.922675387296324,0.998696642611305,0.922675387296324,
0.998696642611305,0.922675387296324,0.998696642611305,0.922675387296324,
0.998696642611305,0.922675387296324,0.998696642611305,0.922675387296324,
0.998696642611305,0.922675387296324,0.998696642611305,0.922675387296324,
0.998696642611305,0.922675387296324,0.998696642611305,0.922675387296324,
0.998696642611305,0.922675387296324,0.998696642611305,0.922675387296324,
0.998696642611305,0.922675387296324,0.998696642611305,0.922675387296324,
0.998696642611305,0.922675387296324,0.998696642611305,0.922675387296324,
0.998696642611305,0.922675387296324,0.998696642611305,0.922675387296324,
0.998696642611305,0.922675387296324,0.998696642611305,0.922675387296324,
0.998696642611305,0.922675387296324,0.998696642611305,0.922675387296324,
0.998696642611305,0.922675387296324,0.998696642611305,0.922675387296324,
0.998696642611305,0.922675387296324,0.998696642611305),(0.998696642611305,
0.922675387296324,0.998696642611305,0.922675387296324,0.998696642611305,
0.922675387296324,0.998696642611305,0.922675387296324,0.998696642611305,
0.922675387296324,0.998696642611305,0.922675387296324,0.998696642611305,
0.922675387296324,0.998696642611305,0.922675387296324,0.998696642611305,
0.922675387296324,0.998696642611305,0.922675387296324,0.998696642611305,
0.922675387296324,0.998696642611305,0.922675387296324,0.998696642611305,
0.922675387296324,0.998696642611305,0.922675387296324,0.998696642611305,
0.922675387296324,0.998696642611305,0.922675387296324,0.998696642611305,
0.922675387296324,0.998696642611305,0.922675387296324,0.998696642611305,
0.922675387296324,0.998696642611305,0.922675387296324,0.998696642611305,
0.922675387296324,0.998696642611305,0.922675387296324,0.998696642611305,
0.922675387296324,0.998696642611305,0.922675387296324,0.998696642611305,
0.922675387296324,0.998696642611305,0.922675387296324,0.998696642611305,
0.922675387296324,0.998696642611305,0.922675387296324,0.998696642611305,
0.922675387296324,0.998696642611305,0.922675387296324,0.998696642611305,
0.922675387296324,0.998696642611305,0.922675387296324,0.998696642611305,
0.922675387296324,0.998696642611305,0.922675387296324,0.998696642611305,
0.922675387296324,0.998696642611305,0.922675387296324,0.998696642611305,
0.922675387296324,0.998696642611305,0.922675387296324,0.998696642611305,
0.922675387296324,0.998696642611305,0.922675387296324,0.998696642611305,
0.922675387296324,0.998696642611305,0.922675387296324,0.998696642611305,
0.922675387296324,0.998696642611305,0.922675387296324,0.998696642611305,
0.922675387296324,0.998696642611305,0.922675387296324,0.998696642611305,
0.922675387296324,0.998696642611305,0.922675387296324,0.998696642611305,
0.922675387296324,0.998696642611305,0.922675387296324,0.998696642611305,
0.922675387296324,0.998696642611305,0.922675387296324,0.998696642611305,
0.922675387296324,0.998696642611305,0.922675387296324,0.998696642611305,
0.922675387296324,0.998696642611305,0.922675387296324,0.998696642611305,
0.922675387296324,0.998696642611305,0.922675387296324,0.998696642611305,
0.922675387296324,0.998696642611305,0.922675387296324,0.998696642611305,
0.922675387296324,0.998696642611305,0.922675387296324,0.998696642611305,
0.922675387296324,0.998696642611305,0.922675387296324,0.998696642611305,
0.922675387296324,0.998696642611305,0.922675387296324,0.998696642611305,
0.922675387296324,0.998696642611305,0.922675387296324,0.998696642611305,
0.922675387296324,0.998696642611305,0.922675387296324,0.998696642611305,
0.922675387296324,0.998696642611305,0.922675387296324,0.998696642611305,
0.922675387296324,0.998696642611305,0.922675387296324,0.998696642611305,
0.922675387296324,0.998696642611305,0.922675387296324,0.998696642611305,
0.922675387296324,0.998696642611305,0.922675387296324,0.998696642611305,
0.922675387296324,0.998696642611305,0.922675387296324,0.998696642611305),
(1.,0.923879532511287,1.,0.923879532511287,1.,0.923879532511287,1.,0.923879532511287,
1.,0.923879532511287,1.,0.923879532511287,1.,0.923879532511287,1.,0.923879532511287,
1.,0.923879532511287,1.,0.923879532511287,1.,0.923879532511287,1.,0.923879532511287,
1.,0.923879532511287,1.,0.923879532511287,1.,0.923879532511287,1.,0.923879532511287,
1.,0.923879532511287,1.,0.923879532511287,1.,0.923879532511287,1.,0.923879532511287,
1.,0.923879532511287,1.,0.923879532511287,1.,0.923879532511287,1.,0.923879532511287,
1.,0.923879532511287,1.,0.923879532511287,1.,0.923879532511287,1.,0.923879532511287,
1.,0.923879532511287,1.,0.923879532511287,1.,0.923879532511287,1.,0.923879532511287,
1.,0.923879532511287,1.,0.923879532511287,1.,0.923879532511287,1.,0.923879532511287,
1.,0.923879532511287,1.,0.923879532511287,1.,0.923879532511287,1.,0.923879532511287,
1.,0.923879532511287,1.,0.923879532511287,1.,0.923879532511287,1.,0.923879532511287,
1.,0.923879532511287,1.,0.923879532511287,1.,0.923879532511287,1.,0.923879532511287,
1.,0.923879532511287,1.,0.923879532511287,1.,0.923879532511287,1.,0.923879532511287,
1.,0.923879532511287,1.,0.923879532511287,1.,0.923879532511287,1.,0.923879532511287,
1.,0.923879532511287,1.,0.923879532511287,1.,0.923879532511287,1.,0.923879532511287,
1.,0.923879532511287,1.,0.923879532511287,1.,0.923879532511287,1.,0.923879532511287,
1.,0.923879532511287,1.,0.923879532511287,1.,0.923879532511287,1.,0.923879532511287,
1.,0.923879532511287,1.,0.923879532511287,1.,0.923879532511287,1.,0.923879532511287,
1.,0.923879532511287,1.,0.923879532511287,1.,0.923879532511287,1.,0.923879532511287,
1.,0.923879532511287,1.,0.923879532511287,1.,0.923879532511287,1.,0.923879532511287,
1.)))
REPRESENTATION_ITEM('')
SURFACE()
);
#566=(
BOUNDED_SURFACE()
B_SPLINE_SURFACE(1,2,((#24684,#24685,#24686,#24687,#24688,#24689,#24690,
#24691,#24692,#24693,#24694,#24695,#24696,#24697,#24698,#24699,#24700,#24701,
#24702,#24703,#24704,#24705,#24706,#24707,#24708,#24709,#24710,#24711,#24712,
#24713,#24714,#24715,#24716,#24717,#24718,#24719,#24720,#24721,#24722,#24723,
#24724,#24725,#24726,#24727,#24728,#24729,#24730,#24731,#24732,#24733,#24734,
#24735,#24736,#24737,#24738,#24739,#24740,#24741,#24742,#24743,#24744,#24745,
#24746,#24747,#24748,#24749,#24750,#24751,#24752,#24753,#24754,#24755,#24756,
#24757,#24758,#24759,#24760,#24761,#24762,#24763,#24764,#24765,#24766,#24767,
#24768,#24769,#24770,#24771,#24772,#24773,#24774,#24775,#24776,#24777,#24778,
#24779,#24780,#24781,#24782,#24783,#24784,#24785,#24786,#24787,#24788,#24789,
#24790,#24791,#24792,#24793,#24794,#24795,#24796,#24797,#24798,#24799,#24800,
#24801,#24802,#24803,#24804,#24805,#24806,#24807,#24808,#24809,#24810,#24811,
#24812,#24813,#24814,#24815,#24816,#24817,#24818,#24819,#24820,#24821,#24822,
#24823,#24824,#24825,#24826,#24827,#24828,#24829,#24830,#24831,#24832,#24833,
#24834,#24835,#24836,#24837,#24838,#24839,#24840,#24841,#24842,#24843,#24844),
(#24845,#24846,#24847,#24848,#24849,#24850,#24851,#24852,#24853,#24854,
#24855,#24856,#24857,#24858,#24859,#24860,#24861,#24862,#24863,#24864,#24865,
#24866,#24867,#24868,#24869,#24870,#24871,#24872,#24873,#24874,#24875,#24876,
#24877,#24878,#24879,#24880,#24881,#24882,#24883,#24884,#24885,#24886,#24887,
#24888,#24889,#24890,#24891,#24892,#24893,#24894,#24895,#24896,#24897,#24898,
#24899,#24900,#24901,#24902,#24903,#24904,#24905,#24906,#24907,#24908,#24909,
#24910,#24911,#24912,#24913,#24914,#24915,#24916,#24917,#24918,#24919,#24920,
#24921,#24922,#24923,#24924,#24925,#24926,#24927,#24928,#24929,#24930,#24931,
#24932,#24933,#24934,#24935,#24936,#24937,#24938,#24939,#24940,#24941,#24942,
#24943,#24944,#24945,#24946,#24947,#24948,#24949,#24950,#24951,#24952,#24953,
#24954,#24955,#24956,#24957,#24958,#24959,#24960,#24961,#24962,#24963,#24964,
#24965,#24966,#24967,#24968,#24969,#24970,#24971,#24972,#24973,#24974,#24975,
#24976,#24977,#24978,#24979,#24980,#24981,#24982,#24983,#24984,#24985,#24986,
#24987,#24988,#24989,#24990,#24991,#24992,#24993,#24994,#24995,#24996,#24997,
#24998,#24999,#25000,#25001,#25002,#25003,#25004,#25005)),.UNSPECIFIED.,
 .F.,.F.,.F.)
B_SPLINE_SURFACE_WITH_KNOTS((2,2),(3,2,2,2,2,2,2,2,2,2,2,2,2,2,2,2,2,2,
2,2,2,2,2,2,2,2,2,2,2,2,2,2,2,2,2,2,2,2,2,2,2,2,2,2,2,2,2,2,2,2,2,2,2,2,
2,2,2,2,2,2,2,2,2,2,2,2,2,2,2,2,2,2,2,2,2,2,2,2,2,2,3),(0.,1.),(0.,0.0125,
0.025,0.0375,0.05,0.0625,0.075,0.0875,0.1,0.1125,0.125,0.1375,0.15,0.1625,
0.175,0.1875,0.2,0.2125,0.225,0.2375,0.25,0.2625,0.275,0.2875,0.3,0.3125,
0.325,0.3375,0.35,0.3625,0.375,0.3875,0.4,0.4125,0.425,0.4375,0.45,0.4625,
0.475,0.4875,0.5,0.5125,0.525,0.5375,0.55,0.5625,0.575,0.5875,0.6,0.6125,
0.625,0.6375,0.65,0.6625,0.675,0.6875,0.7,0.7125,0.725,0.7375,0.75,0.7625,
0.775,0.7875,0.8,0.8125,0.825,0.8375,0.85,0.8625,0.875,0.8875,0.9,0.9125,
0.925,0.9375,0.95,0.9625,0.975,0.9875,1.),.UNSPECIFIED.)
GEOMETRIC_REPRESENTATION_ITEM()
RATIONAL_B_SPLINE_SURFACE(((1.,0.923879532511287,1.,0.923879532511287,1.,
0.923879532511287,1.,0.923879532511287,1.,0.923879532511287,1.,0.923879532511287,
1.,0.923879532511287,1.,0.923879532511287,1.,0.923879532511287,1.,0.923879532511287,
1.,0.923879532511287,1.,0.923879532511287,1.,0.923879532511287,1.,0.923879532511287,
1.,0.923879532511287,1.,0.923879532511287,1.,0.923879532511287,1.,0.923879532511287,
1.,0.923879532511287,1.,0.923879532511287,1.,0.923879532511287,1.,0.923879532511287,
1.,0.923879532511287,1.,0.923879532511287,1.,0.923879532511287,1.,0.923879532511287,
1.,0.923879532511287,1.,0.923879532511287,1.,0.923879532511287,1.,0.923879532511287,
1.,0.923879532511287,1.,0.923879532511287,1.,0.923879532511287,1.,0.923879532511287,
1.,0.923879532511287,1.,0.923879532511287,1.,0.923879532511287,1.,0.923879532511287,
1.,0.923879532511287,1.,0.923879532511287,1.,0.923879532511287,1.,0.923879532511287,
1.,0.923879532511287,1.,0.923879532511287,1.,0.923879532511287,1.,0.923879532511287,
1.,0.923879532511287,1.,0.923879532511287,1.,0.923879532511287,1.,0.923879532511287,
1.,0.923879532511287,1.,0.923879532511287,1.,0.923879532511287,1.,0.923879532511287,
1.,0.923879532511287,1.,0.923879532511287,1.,0.923879532511287,1.,0.923879532511287,
1.,0.923879532511287,1.,0.923879532511287,1.,0.923879532511287,1.,0.923879532511287,
1.,0.923879532511287,1.,0.923879532511287,1.,0.923879532511287,1.,0.923879532511287,
1.,0.923879532511287,1.,0.923879532511287,1.,0.923879532511287,1.,0.923879532511287,
1.,0.923879532511287,1.,0.923879532511287,1.,0.923879532511287,1.,0.923879532511287,
1.,0.923879532511287,1.,0.923879532511287,1.,0.923879532511287,1.,0.923879532511287,
1.,0.923879532511287,1.,0.923879532511287,1.),(1.,0.923879532511287,1.,
0.923879532511287,1.,0.923879532511287,1.,0.923879532511287,1.,0.923879532511287,
1.,0.923879532511287,1.,0.923879532511287,1.,0.923879532511287,1.,0.923879532511287,
1.,0.923879532511287,1.,0.923879532511287,1.,0.923879532511287,1.,0.923879532511287,
1.,0.923879532511287,1.,0.923879532511287,1.,0.923879532511287,1.,0.923879532511287,
1.,0.923879532511287,1.,0.923879532511287,1.,0.923879532511287,1.,0.923879532511287,
1.,0.923879532511287,1.,0.923879532511287,1.,0.923879532511287,1.,0.923879532511287,
1.,0.923879532511287,1.,0.923879532511287,1.,0.923879532511287,1.,0.923879532511287,
1.,0.923879532511287,1.,0.923879532511287,1.,0.923879532511287,1.,0.923879532511287,
1.,0.923879532511287,1.,0.923879532511287,1.,0.923879532511287,1.,0.923879532511287,
1.,0.923879532511287,1.,0.923879532511287,1.,0.923879532511287,1.,0.923879532511287,
1.,0.923879532511287,1.,0.923879532511287,1.,0.923879532511287,1.,0.923879532511287,
1.,0.923879532511287,1.,0.923879532511287,1.,0.923879532511287,1.,0.923879532511287,
1.,0.923879532511287,1.,0.923879532511287,1.,0.923879532511287,1.,0.923879532511287,
1.,0.923879532511287,1.,0.923879532511287,1.,0.923879532511287,1.,0.923879532511287,
1.,0.923879532511287,1.,0.923879532511287,1.,0.923879532511287,1.,0.923879532511287,
1.,0.923879532511287,1.,0.923879532511287,1.,0.923879532511287,1.,0.923879532511287,
1.,0.923879532511287,1.,0.923879532511287,1.,0.923879532511287,1.,0.923879532511287,
1.,0.923879532511287,1.,0.923879532511287,1.,0.923879532511287,1.,0.923879532511287,
1.,0.923879532511287,1.,0.923879532511287,1.,0.923879532511287,1.,0.923879532511287,
1.,0.923879532511287,1.,0.923879532511287,1.,0.923879532511287,1.)))
REPRESENTATION_ITEM('')
SURFACE()
);
#567=(
BOUNDED_SURFACE()
B_SPLINE_SURFACE(1,2,((#25023,#25024,#25025,#25026,#25027,#25028,#25029,
#25030,#25031,#25032,#25033,#25034,#25035,#25036,#25037,#25038,#25039,#25040,
#25041,#25042,#25043,#25044,#25045,#25046,#25047,#25048,#25049,#25050,#25051,
#25052,#25053,#25054,#25055,#25056,#25057,#25058,#25059,#25060,#25061,#25062,
#25063,#25064,#25065,#25066,#25067,#25068,#25069,#25070,#25071,#25072,#25073,
#25074,#25075,#25076,#25077,#25078,#25079,#25080,#25081,#25082,#25083,#25084,
#25085,#25086,#25087,#25088,#25089,#25090,#25091,#25092,#25093,#25094,#25095,
#25096,#25097,#25098,#25099,#25100,#25101,#25102,#25103,#25104,#25105,#25106,
#25107,#25108,#25109,#25110,#25111,#25112,#25113,#25114,#25115,#25116,#25117,
#25118,#25119,#25120,#25121,#25122,#25123,#25124,#25125,#25126,#25127,#25128,
#25129,#25130,#25131,#25132,#25133,#25134,#25135,#25136,#25137,#25138,#25139,
#25140,#25141,#25142,#25143,#25144,#25145,#25146,#25147,#25148,#25149,#25150,
#25151,#25152,#25153,#25154,#25155,#25156,#25157,#25158,#25159,#25160,#25161,
#25162,#25163,#25164,#25165,#25166,#25167,#25168,#25169,#25170,#25171,#25172,
#25173,#25174,#25175,#25176,#25177,#25178,#25179,#25180,#25181,#25182,#25183),
(#25184,#25185,#25186,#25187,#25188,#25189,#25190,#25191,#25192,#25193,
#25194,#25195,#25196,#25197,#25198,#25199,#25200,#25201,#25202,#25203,#25204,
#25205,#25206,#25207,#25208,#25209,#25210,#25211,#25212,#25213,#25214,#25215,
#25216,#25217,#25218,#25219,#25220,#25221,#25222,#25223,#25224,#25225,#25226,
#25227,#25228,#25229,#25230,#25231,#25232,#25233,#25234,#25235,#25236,#25237,
#25238,#25239,#25240,#25241,#25242,#25243,#25244,#25245,#25246,#25247,#25248,
#25249,#25250,#25251,#25252,#25253,#25254,#25255,#25256,#25257,#25258,#25259,
#25260,#25261,#25262,#25263,#25264,#25265,#25266,#25267,#25268,#25269,#25270,
#25271,#25272,#25273,#25274,#25275,#25276,#25277,#25278,#25279,#25280,#25281,
#25282,#25283,#25284,#25285,#25286,#25287,#25288,#25289,#25290,#25291,#25292,
#25293,#25294,#25295,#25296,#25297,#25298,#25299,#25300,#25301,#25302,#25303,
#25304,#25305,#25306,#25307,#25308,#25309,#25310,#25311,#25312,#25313,#25314,
#25315,#25316,#25317,#25318,#25319,#25320,#25321,#25322,#25323,#25324,#25325,
#25326,#25327,#25328,#25329,#25330,#25331,#25332,#25333,#25334,#25335,#25336,
#25337,#25338,#25339,#25340,#25341,#25342,#25343,#25344)),.UNSPECIFIED.,
 .F.,.F.,.F.)
B_SPLINE_SURFACE_WITH_KNOTS((2,2),(3,2,2,2,2,2,2,2,2,2,2,2,2,2,2,2,2,2,
2,2,2,2,2,2,2,2,2,2,2,2,2,2,2,2,2,2,2,2,2,2,2,2,2,2,2,2,2,2,2,2,2,2,2,2,
2,2,2,2,2,2,2,2,2,2,2,2,2,2,2,2,2,2,2,2,2,2,2,2,2,2,3),(0.,1.),(0.,0.0125,
0.025,0.0375,0.05,0.0625,0.075,0.0875,0.1,0.1125,0.125,0.1375,0.15,0.1625,
0.175,0.1875,0.2,0.2125,0.225,0.2375,0.25,0.2625,0.275,0.2875,0.3,0.3125,
0.325,0.3375,0.35,0.3625,0.375,0.3875,0.4,0.4125,0.425,0.4375,0.45,0.4625,
0.475,0.4875,0.5,0.5125,0.525,0.5375,0.55,0.5625,0.575,0.5875,0.6,0.6125,
0.625,0.6375,0.65,0.6625,0.675,0.6875,0.7,0.7125,0.725,0.7375,0.75,0.7625,
0.775,0.7875,0.8,0.8125,0.825,0.8375,0.85,0.8625,0.875,0.8875,0.9,0.9125,
0.925,0.9375,0.95,0.9625,0.975,0.9875,1.),.UNSPECIFIED.)
GEOMETRIC_REPRESENTATION_ITEM()
RATIONAL_B_SPLINE_SURFACE(((1.,0.923879532511287,1.,0.923879532511287,1.,
0.923879532511287,1.,0.923879532511287,1.,0.923879532511287,1.,0.923879532511287,
1.,0.923879532511287,1.,0.923879532511287,1.,0.923879532511287,1.,0.923879532511287,
1.,0.923879532511287,1.,0.923879532511287,1.,0.923879532511287,1.,0.923879532511287,
1.,0.923879532511287,1.,0.923879532511287,1.,0.923879532511287,1.,0.923879532511287,
1.,0.923879532511287,1.,0.923879532511287,1.,0.923879532511287,1.,0.923879532511287,
1.,0.923879532511287,1.,0.923879532511287,1.,0.923879532511287,1.,0.923879532511287,
1.,0.923879532511287,1.,0.923879532511287,1.,0.923879532511287,1.,0.923879532511287,
1.,0.923879532511287,1.,0.923879532511287,1.,0.923879532511287,1.,0.923879532511287,
1.,0.923879532511287,1.,0.923879532511287,1.,0.923879532511287,1.,0.923879532511287,
1.,0.923879532511287,1.,0.923879532511287,1.,0.923879532511287,1.,0.923879532511287,
1.,0.923879532511287,1.,0.923879532511287,1.,0.923879532511287,1.,0.923879532511287,
1.,0.923879532511287,1.,0.923879532511287,1.,0.923879532511287,1.,0.923879532511287,
1.,0.923879532511287,1.,0.923879532511287,1.,0.923879532511287,1.,0.923879532511287,
1.,0.923879532511287,1.,0.923879532511287,1.,0.923879532511287,1.,0.923879532511287,
1.,0.923879532511287,1.,0.923879532511287,1.,0.923879532511287,1.,0.923879532511287,
1.,0.923879532511287,1.,0.923879532511287,1.,0.923879532511287,1.,0.923879532511287,
1.,0.923879532511287,1.,0.923879532511287,1.,0.923879532511287,1.,0.923879532511287,
1.,0.923879532511287,1.,0.923879532511287,1.,0.923879532511287,1.,0.923879532511287,
1.,0.923879532511287,1.,0.923879532511287,1.,0.923879532511287,1.,0.923879532511287,
1.,0.923879532511287,1.,0.923879532511287,1.),(1.,0.923879532511287,1.,
0.923879532511287,1.,0.923879532511287,1.,0.923879532511287,1.,0.923879532511287,
1.,0.923879532511287,1.,0.923879532511287,1.,0.923879532511287,1.,0.923879532511287,
1.,0.923879532511287,1.,0.923879532511287,1.,0.923879532511287,1.,0.923879532511287,
1.,0.923879532511287,1.,0.923879532511287,1.,0.923879532511287,1.,0.923879532511287,
1.,0.923879532511287,1.,0.923879532511287,1.,0.923879532511287,1.,0.923879532511287,
1.,0.923879532511287,1.,0.923879532511287,1.,0.923879532511287,1.,0.923879532511287,
1.,0.923879532511287,1.,0.923879532511287,1.,0.923879532511287,1.,0.923879532511287,
1.,0.923879532511287,1.,0.923879532511287,1.,0.923879532511287,1.,0.923879532511287,
1.,0.923879532511287,1.,0.923879532511287,1.,0.923879532511287,1.,0.923879532511287,
1.,0.923879532511287,1.,0.923879532511287,1.,0.923879532511287,1.,0.923879532511287,
1.,0.923879532511287,1.,0.923879532511287,1.,0.923879532511287,1.,0.923879532511287,
1.,0.923879532511287,1.,0.923879532511287,1.,0.923879532511287,1.,0.923879532511287,
1.,0.923879532511287,1.,0.923879532511287,1.,0.923879532511287,1.,0.923879532511287,
1.,0.923879532511287,1.,0.923879532511287,1.,0.923879532511287,1.,0.923879532511287,
1.,0.923879532511287,1.,0.923879532511287,1.,0.923879532511287,1.,0.923879532511287,
1.,0.923879532511287,1.,0.923879532511287,1.,0.923879532511287,1.,0.923879532511287,
1.,0.923879532511287,1.,0.923879532511287,1.,0.923879532511287,1.,0.923879532511287,
1.,0.923879532511287,1.,0.923879532511287,1.,0.923879532511287,1.,0.923879532511287,
1.,0.923879532511287,1.,0.923879532511287,1.,0.923879532511287,1.,0.923879532511287,
1.,0.923879532511287,1.,0.923879532511287,1.,0.923879532511287,1.)))
REPRESENTATION_ITEM('')
SURFACE()
);
#568=(
BOUNDED_SURFACE()
B_SPLINE_SURFACE(3,2,((#25362,#25363,#25364,#25365,#25366,#25367,#25368,
#25369,#25370,#25371,#25372,#25373,#25374,#25375,#25376,#25377,#25378,#25379,
#25380,#25381,#25382,#25383,#25384,#25385,#25386,#25387,#25388,#25389,#25390,
#25391,#25392,#25393,#25394,#25395,#25396,#25397,#25398,#25399,#25400,#25401,
#25402,#25403,#25404,#25405,#25406,#25407,#25408,#25409,#25410,#25411,#25412,
#25413,#25414,#25415,#25416,#25417,#25418,#25419,#25420,#25421,#25422,#25423,
#25424,#25425,#25426,#25427,#25428,#25429,#25430,#25431,#25432,#25433,#25434,
#25435,#25436,#25437,#25438,#25439,#25440,#25441,#25442,#25443,#25444,#25445,
#25446,#25447,#25448,#25449,#25450,#25451,#25452,#25453,#25454,#25455,#25456,
#25457,#25458,#25459,#25460,#25461,#25462,#25463,#25464,#25465,#25466,#25467,
#25468,#25469,#25470,#25471,#25472,#25473,#25474,#25475,#25476,#25477,#25478,
#25479,#25480,#25481,#25482,#25483,#25484,#25485,#25486,#25487,#25488,#25489,
#25490,#25491,#25492,#25493,#25494,#25495,#25496,#25497,#25498,#25499,#25500,
#25501,#25502,#25503,#25504,#25505,#25506,#25507,#25508,#25509,#25510,#25511,
#25512,#25513,#25514,#25515,#25516,#25517,#25518,#25519,#25520,#25521,#25522),
(#25523,#25524,#25525,#25526,#25527,#25528,#25529,#25530,#25531,#25532,
#25533,#25534,#25535,#25536,#25537,#25538,#25539,#25540,#25541,#25542,#25543,
#25544,#25545,#25546,#25547,#25548,#25549,#25550,#25551,#25552,#25553,#25554,
#25555,#25556,#25557,#25558,#25559,#25560,#25561,#25562,#25563,#25564,#25565,
#25566,#25567,#25568,#25569,#25570,#25571,#25572,#25573,#25574,#25575,#25576,
#25577,#25578,#25579,#25580,#25581,#25582,#25583,#25584,#25585,#25586,#25587,
#25588,#25589,#25590,#25591,#25592,#25593,#25594,#25595,#25596,#25597,#25598,
#25599,#25600,#25601,#25602,#25603,#25604,#25605,#25606,#25607,#25608,#25609,
#25610,#25611,#25612,#25613,#25614,#25615,#25616,#25617,#25618,#25619,#25620,
#25621,#25622,#25623,#25624,#25625,#25626,#25627,#25628,#25629,#25630,#25631,
#25632,#25633,#25634,#25635,#25636,#25637,#25638,#25639,#25640,#25641,#25642,
#25643,#25644,#25645,#25646,#25647,#25648,#25649,#25650,#25651,#25652,#25653,
#25654,#25655,#25656,#25657,#25658,#25659,#25660,#25661,#25662,#25663,#25664,
#25665,#25666,#25667,#25668,#25669,#25670,#25671,#25672,#25673,#25674,#25675,
#25676,#25677,#25678,#25679,#25680,#25681,#25682,#25683),(#25684,#25685,
#25686,#25687,#25688,#25689,#25690,#25691,#25692,#25693,#25694,#25695,#25696,
#25697,#25698,#25699,#25700,#25701,#25702,#25703,#25704,#25705,#25706,#25707,
#25708,#25709,#25710,#25711,#25712,#25713,#25714,#25715,#25716,#25717,#25718,
#25719,#25720,#25721,#25722,#25723,#25724,#25725,#25726,#25727,#25728,#25729,
#25730,#25731,#25732,#25733,#25734,#25735,#25736,#25737,#25738,#25739,#25740,
#25741,#25742,#25743,#25744,#25745,#25746,#25747,#25748,#25749,#25750,#25751,
#25752,#25753,#25754,#25755,#25756,#25757,#25758,#25759,#25760,#25761,#25762,
#25763,#25764,#25765,#25766,#25767,#25768,#25769,#25770,#25771,#25772,#25773,
#25774,#25775,#25776,#25777,#25778,#25779,#25780,#25781,#25782,#25783,#25784,
#25785,#25786,#25787,#25788,#25789,#25790,#25791,#25792,#25793,#25794,#25795,
#25796,#25797,#25798,#25799,#25800,#25801,#25802,#25803,#25804,#25805,#25806,
#25807,#25808,#25809,#25810,#25811,#25812,#25813,#25814,#25815,#25816,#25817,
#25818,#25819,#25820,#25821,#25822,#25823,#25824,#25825,#25826,#25827,#25828,
#25829,#25830,#25831,#25832,#25833,#25834,#25835,#25836,#25837,#25838,#25839,
#25840,#25841,#25842,#25843,#25844),(#25845,#25846,#25847,#25848,#25849,
#25850,#25851,#25852,#25853,#25854,#25855,#25856,#25857,#25858,#25859,#25860,
#25861,#25862,#25863,#25864,#25865,#25866,#25867,#25868,#25869,#25870,#25871,
#25872,#25873,#25874,#25875,#25876,#25877,#25878,#25879,#25880,#25881,#25882,
#25883,#25884,#25885,#25886,#25887,#25888,#25889,#25890,#25891,#25892,#25893,
#25894,#25895,#25896,#25897,#25898,#25899,#25900,#25901,#25902,#25903,#25904,
#25905,#25906,#25907,#25908,#25909,#25910,#25911,#25912,#25913,#25914,#25915,
#25916,#25917,#25918,#25919,#25920,#25921,#25922,#25923,#25924,#25925,#25926,
#25927,#25928,#25929,#25930,#25931,#25932,#25933,#25934,#25935,#25936,#25937,
#25938,#25939,#25940,#25941,#25942,#25943,#25944,#25945,#25946,#25947,#25948,
#25949,#25950,#25951,#25952,#25953,#25954,#25955,#25956,#25957,#25958,#25959,
#25960,#25961,#25962,#25963,#25964,#25965,#25966,#25967,#25968,#25969,#25970,
#25971,#25972,#25973,#25974,#25975,#25976,#25977,#25978,#25979,#25980,#25981,
#25982,#25983,#25984,#25985,#25986,#25987,#25988,#25989,#25990,#25991,#25992,
#25993,#25994,#25995,#25996,#25997,#25998,#25999,#26000,#26001,#26002,#26003,
#26004,#26005)),.UNSPECIFIED.,.F.,.F.,.F.)
B_SPLINE_SURFACE_WITH_KNOTS((4,4),(3,2,2,2,2,2,2,2,2,2,2,2,2,2,2,2,2,2,
2,2,2,2,2,2,2,2,2,2,2,2,2,2,2,2,2,2,2,2,2,2,2,2,2,2,2,2,2,2,2,2,2,2,2,2,
2,2,2,2,2,2,2,2,2,2,2,2,2,2,2,2,2,2,2,2,2,2,2,2,2,2,3),(0.,1.),(0.,0.0125,
0.025,0.0375,0.05,0.0625,0.075,0.0875,0.1,0.1125,0.125,0.1375,0.15,0.1625,
0.175,0.1875,0.2,0.2125,0.225,0.2375,0.25,0.2625,0.275,0.2875,0.3,0.3125,
0.325,0.3375,0.35,0.3625,0.375,0.3875,0.4,0.4125,0.425,0.4375,0.45,0.4625,
0.475,0.4875,0.5,0.5125,0.525,0.5375,0.55,0.5625,0.575,0.5875,0.6,0.6125,
0.625,0.6375,0.65,0.6625,0.675,0.6875,0.7,0.7125,0.725,0.7375,0.75,0.7625,
0.775,0.7875,0.8,0.8125,0.825,0.8375,0.85,0.8625,0.875,0.8875,0.9,0.9125,
0.925,0.9375,0.95,0.9625,0.975,0.9875,1.),.UNSPECIFIED.)
GEOMETRIC_REPRESENTATION_ITEM()
RATIONAL_B_SPLINE_SURFACE(((1.,0.923879532511287,1.,0.923879532511287,1.,
0.923879532511287,1.,0.923879532511287,1.,0.923879532511287,1.,0.923879532511287,
1.,0.923879532511287,1.,0.923879532511287,1.,0.923879532511287,1.,0.923879532511287,
1.,0.923879532511287,1.,0.923879532511287,1.,0.923879532511287,1.,0.923879532511287,
1.,0.923879532511287,1.,0.923879532511287,1.,0.923879532511287,1.,0.923879532511287,
1.,0.923879532511287,1.,0.923879532511287,1.,0.923879532511287,1.,0.923879532511287,
1.,0.923879532511287,1.,0.923879532511287,1.,0.923879532511287,1.,0.923879532511287,
1.,0.923879532511287,1.,0.923879532511287,1.,0.923879532511287,1.,0.923879532511287,
1.,0.923879532511287,1.,0.923879532511287,1.,0.923879532511287,1.,0.923879532511287,
1.,0.923879532511287,1.,0.923879532511287,1.,0.923879532511287,1.,0.923879532511287,
1.,0.923879532511287,1.,0.923879532511287,1.,0.923879532511287,1.,0.923879532511287,
1.,0.923879532511287,1.,0.923879532511287,1.,0.923879532511287,1.,0.923879532511287,
1.,0.923879532511287,1.,0.923879532511287,1.,0.923879532511287,1.,0.923879532511287,
1.,0.923879532511287,1.,0.923879532511287,1.,0.923879532511287,1.,0.923879532511287,
1.,0.923879532511287,1.,0.923879532511287,1.,0.923879532511287,1.,0.923879532511287,
1.,0.923879532511287,1.,0.923879532511287,1.,0.923879532511287,1.,0.923879532511287,
1.,0.923879532511287,1.,0.923879532511287,1.,0.923879532511287,1.,0.923879532511287,
1.,0.923879532511287,1.,0.923879532511287,1.,0.923879532511287,1.,0.923879532511287,
1.,0.923879532511287,1.,0.923879532511287,1.,0.923879532511287,1.,0.923879532511287,
1.,0.923879532511287,1.,0.923879532511287,1.,0.923879532511287,1.,0.923879532511287,
1.,0.923879532511287,1.,0.923879532511287,1.),(0.998696642611305,0.922675387296324,
0.998696642611305,0.922675387296324,0.998696642611305,0.922675387296324,
0.998696642611305,0.922675387296324,0.998696642611305,0.922675387296324,
0.998696642611305,0.922675387296324,0.998696642611305,0.922675387296324,
0.998696642611305,0.922675387296324,0.998696642611305,0.922675387296324,
0.998696642611305,0.922675387296324,0.998696642611305,0.922675387296324,
0.998696642611305,0.922675387296324,0.998696642611305,0.922675387296324,
0.998696642611305,0.922675387296324,0.998696642611305,0.922675387296324,
0.998696642611305,0.922675387296324,0.998696642611305,0.922675387296324,
0.998696642611305,0.922675387296324,0.998696642611305,0.922675387296324,
0.998696642611305,0.922675387296324,0.998696642611305,0.922675387296324,
0.998696642611305,0.922675387296324,0.998696642611305,0.922675387296324,
0.998696642611305,0.922675387296324,0.998696642611305,0.922675387296324,
0.998696642611305,0.922675387296324,0.998696642611305,0.922675387296324,
0.998696642611305,0.922675387296324,0.998696642611305,0.922675387296324,
0.998696642611305,0.922675387296324,0.998696642611305,0.922675387296324,
0.998696642611305,0.922675387296324,0.998696642611305,0.922675387296324,
0.998696642611305,0.922675387296324,0.998696642611305,0.922675387296324,
0.998696642611305,0.922675387296324,0.998696642611305,0.922675387296324,
0.998696642611305,0.922675387296324,0.998696642611305,0.922675387296324,
0.998696642611305,0.922675387296324,0.998696642611305,0.922675387296324,
0.998696642611305,0.922675387296324,0.998696642611305,0.922675387296324,
0.998696642611305,0.922675387296324,0.998696642611305,0.922675387296324,
0.998696642611305,0.922675387296324,0.998696642611305,0.922675387296324,
0.998696642611305,0.922675387296324,0.998696642611305,0.922675387296324,
0.998696642611305,0.922675387296324,0.998696642611305,0.922675387296324,
0.998696642611305,0.922675387296324,0.998696642611305,0.922675387296324,
0.998696642611305,0.922675387296324,0.998696642611305,0.922675387296324,
0.998696642611305,0.922675387296324,0.998696642611305,0.922675387296324,
0.998696642611305,0.922675387296324,0.998696642611305,0.922675387296324,
0.998696642611305,0.922675387296324,0.998696642611305,0.922675387296324,
0.998696642611305,0.922675387296324,0.998696642611305,0.922675387296324,
0.998696642611305,0.922675387296324,0.998696642611305,0.922675387296324,
0.998696642611305,0.922675387296324,0.998696642611305,0.922675387296324,
0.998696642611305,0.922675387296324,0.998696642611305,0.922675387296324,
0.998696642611305,0.922675387296324,0.998696642611305,0.922675387296324,
0.998696642611305,0.922675387296324,0.998696642611305,0.922675387296324,
0.998696642611305,0.922675387296324,0.998696642611305,0.922675387296324,
0.998696642611305,0.922675387296324,0.998696642611305,0.922675387296324,
0.998696642611305,0.922675387296324,0.998696642611305,0.922675387296324,
0.998696642611305,0.922675387296324,0.998696642611305),(0.998696642611305,
0.922675387296324,0.998696642611305,0.922675387296324,0.998696642611305,
0.922675387296324,0.998696642611305,0.922675387296324,0.998696642611305,
0.922675387296324,0.998696642611305,0.922675387296324,0.998696642611305,
0.922675387296324,0.998696642611305,0.922675387296324,0.998696642611305,
0.922675387296324,0.998696642611305,0.922675387296324,0.998696642611305,
0.922675387296324,0.998696642611305,0.922675387296324,0.998696642611305,
0.922675387296324,0.998696642611305,0.922675387296324,0.998696642611305,
0.922675387296324,0.998696642611305,0.922675387296324,0.998696642611305,
0.922675387296324,0.998696642611305,0.922675387296324,0.998696642611305,
0.922675387296324,0.998696642611305,0.922675387296324,0.998696642611305,
0.922675387296324,0.998696642611305,0.922675387296324,0.998696642611305,
0.922675387296324,0.998696642611305,0.922675387296324,0.998696642611305,
0.922675387296324,0.998696642611305,0.922675387296324,0.998696642611305,
0.922675387296324,0.998696642611305,0.922675387296324,0.998696642611305,
0.922675387296324,0.998696642611305,0.922675387296324,0.998696642611305,
0.922675387296324,0.998696642611305,0.922675387296324,0.998696642611305,
0.922675387296324,0.998696642611305,0.922675387296324,0.998696642611305,
0.922675387296324,0.998696642611305,0.922675387296324,0.998696642611305,
0.922675387296324,0.998696642611305,0.922675387296324,0.998696642611305,
0.922675387296324,0.998696642611305,0.922675387296324,0.998696642611305,
0.922675387296324,0.998696642611305,0.922675387296324,0.998696642611305,
0.922675387296324,0.998696642611305,0.922675387296324,0.998696642611305,
0.922675387296324,0.998696642611305,0.922675387296324,0.998696642611305,
0.922675387296324,0.998696642611305,0.922675387296324,0.998696642611305,
0.922675387296324,0.998696642611305,0.922675387296324,0.998696642611305,
0.922675387296324,0.998696642611305,0.922675387296324,0.998696642611305,
0.922675387296324,0.998696642611305,0.922675387296324,0.998696642611305,
0.922675387296324,0.998696642611305,0.922675387296324,0.998696642611305,
0.922675387296324,0.998696642611305,0.922675387296324,0.998696642611305,
0.922675387296324,0.998696642611305,0.922675387296324,0.998696642611305,
0.922675387296324,0.998696642611305,0.922675387296324,0.998696642611305,
0.922675387296324,0.998696642611305,0.922675387296324,0.998696642611305,
0.922675387296324,0.998696642611305,0.922675387296324,0.998696642611305,
0.922675387296324,0.998696642611305,0.922675387296324,0.998696642611305,
0.922675387296324,0.998696642611305,0.922675387296324,0.998696642611305,
0.922675387296324,0.998696642611305,0.922675387296324,0.998696642611305,
0.922675387296324,0.998696642611305,0.922675387296324,0.998696642611305,
0.922675387296324,0.998696642611305,0.922675387296324,0.998696642611305,
0.922675387296324,0.998696642611305,0.922675387296324,0.998696642611305,
0.922675387296324,0.998696642611305,0.922675387296324,0.998696642611305),
(1.,0.923879532511287,1.,0.923879532511287,1.,0.923879532511287,1.,0.923879532511287,
1.,0.923879532511287,1.,0.923879532511287,1.,0.923879532511287,1.,0.923879532511287,
1.,0.923879532511287,1.,0.923879532511287,1.,0.923879532511287,1.,0.923879532511287,
1.,0.923879532511287,1.,0.923879532511287,1.,0.923879532511287,1.,0.923879532511287,
1.,0.923879532511287,1.,0.923879532511287,1.,0.923879532511287,1.,0.923879532511287,
1.,0.923879532511287,1.,0.923879532511287,1.,0.923879532511287,1.,0.923879532511287,
1.,0.923879532511287,1.,0.923879532511287,1.,0.923879532511287,1.,0.923879532511287,
1.,0.923879532511287,1.,0.923879532511287,1.,0.923879532511287,1.,0.923879532511287,
1.,0.923879532511287,1.,0.923879532511287,1.,0.923879532511287,1.,0.923879532511287,
1.,0.923879532511287,1.,0.923879532511287,1.,0.923879532511287,1.,0.923879532511287,
1.,0.923879532511287,1.,0.923879532511287,1.,0.923879532511287,1.,0.923879532511287,
1.,0.923879532511287,1.,0.923879532511287,1.,0.923879532511287,1.,0.923879532511287,
1.,0.923879532511287,1.,0.923879532511287,1.,0.923879532511287,1.,0.923879532511287,
1.,0.923879532511287,1.,0.923879532511287,1.,0.923879532511287,1.,0.923879532511287,
1.,0.923879532511287,1.,0.923879532511287,1.,0.923879532511287,1.,0.923879532511287,
1.,0.923879532511287,1.,0.923879532511287,1.,0.923879532511287,1.,0.923879532511287,
1.,0.923879532511287,1.,0.923879532511287,1.,0.923879532511287,1.,0.923879532511287,
1.,0.923879532511287,1.,0.923879532511287,1.,0.923879532511287,1.,0.923879532511287,
1.,0.923879532511287,1.,0.923879532511287,1.,0.923879532511287,1.,0.923879532511287,
1.,0.923879532511287,1.,0.923879532511287,1.,0.923879532511287,1.,0.923879532511287,
1.)))
REPRESENTATION_ITEM('')
SURFACE()
);
#569=(
BOUNDED_SURFACE()
B_SPLINE_SURFACE(1,2,((#26006,#26007,#26008,#26009,#26010,#26011,#26012,
#26013,#26014,#26015,#26016,#26017,#26018,#26019,#26020,#26021,#26022,#26023,
#26024,#26025,#26026,#26027,#26028,#26029,#26030,#26031,#26032,#26033,#26034,
#26035,#26036,#26037,#26038,#26039,#26040,#26041,#26042,#26043,#26044,#26045,
#26046,#26047,#26048,#26049,#26050,#26051,#26052,#26053,#26054,#26055,#26056,
#26057,#26058,#26059,#26060,#26061,#26062,#26063,#26064,#26065,#26066,#26067,
#26068,#26069,#26070,#26071,#26072,#26073,#26074,#26075,#26076,#26077,#26078,
#26079,#26080,#26081,#26082,#26083,#26084,#26085,#26086,#26087,#26088,#26089,
#26090,#26091,#26092,#26093,#26094,#26095,#26096,#26097,#26098,#26099,#26100,
#26101,#26102,#26103,#26104,#26105,#26106,#26107,#26108,#26109,#26110,#26111,
#26112,#26113,#26114,#26115,#26116,#26117,#26118,#26119,#26120,#26121,#26122,
#26123,#26124,#26125,#26126,#26127,#26128,#26129,#26130,#26131,#26132,#26133,
#26134,#26135,#26136,#26137,#26138,#26139,#26140,#26141,#26142,#26143,#26144,
#26145,#26146,#26147,#26148,#26149,#26150,#26151,#26152,#26153,#26154,#26155,
#26156,#26157,#26158,#26159,#26160,#26161,#26162,#26163,#26164,#26165,#26166),
(#26167,#26168,#26169,#26170,#26171,#26172,#26173,#26174,#26175,#26176,
#26177,#26178,#26179,#26180,#26181,#26182,#26183,#26184,#26185,#26186,#26187,
#26188,#26189,#26190,#26191,#26192,#26193,#26194,#26195,#26196,#26197,#26198,
#26199,#26200,#26201,#26202,#26203,#26204,#26205,#26206,#26207,#26208,#26209,
#26210,#26211,#26212,#26213,#26214,#26215,#26216,#26217,#26218,#26219,#26220,
#26221,#26222,#26223,#26224,#26225,#26226,#26227,#26228,#26229,#26230,#26231,
#26232,#26233,#26234,#26235,#26236,#26237,#26238,#26239,#26240,#26241,#26242,
#26243,#26244,#26245,#26246,#26247,#26248,#26249,#26250,#26251,#26252,#26253,
#26254,#26255,#26256,#26257,#26258,#26259,#26260,#26261,#26262,#26263,#26264,
#26265,#26266,#26267,#26268,#26269,#26270,#26271,#26272,#26273,#26274,#26275,
#26276,#26277,#26278,#26279,#26280,#26281,#26282,#26283,#26284,#26285,#26286,
#26287,#26288,#26289,#26290,#26291,#26292,#26293,#26294,#26295,#26296,#26297,
#26298,#26299,#26300,#26301,#26302,#26303,#26304,#26305,#26306,#26307,#26308,
#26309,#26310,#26311,#26312,#26313,#26314,#26315,#26316,#26317,#26318,#26319,
#26320,#26321,#26322,#26323,#26324,#26325,#26326,#26327)),.UNSPECIFIED.,
 .F.,.F.,.F.)
B_SPLINE_SURFACE_WITH_KNOTS((2,2),(3,2,2,2,2,2,2,2,2,2,2,2,2,2,2,2,2,2,
2,2,2,2,2,2,2,2,2,2,2,2,2,2,2,2,2,2,2,2,2,2,2,2,2,2,2,2,2,2,2,2,2,2,2,2,
2,2,2,2,2,2,2,2,2,2,2,2,2,2,2,2,2,2,2,2,2,2,2,2,2,2,3),(0.,1.),(0.,0.0125,
0.025,0.0375,0.05,0.0625,0.075,0.0875,0.1,0.1125,0.125,0.1375,0.15,0.1625,
0.175,0.1875,0.2,0.2125,0.225,0.2375,0.25,0.2625,0.275,0.2875,0.3,0.3125,
0.325,0.3375,0.35,0.3625,0.375,0.3875,0.4,0.4125,0.425,0.4375,0.45,0.4625,
0.475,0.4875,0.5,0.5125,0.525,0.5375,0.55,0.5625,0.575,0.5875,0.6,0.6125,
0.625,0.6375,0.65,0.6625,0.675,0.6875,0.7,0.7125,0.725,0.7375,0.75,0.7625,
0.775,0.7875,0.8,0.8125,0.825,0.8375,0.85,0.8625,0.875,0.8875,0.9,0.9125,
0.925,0.9375,0.95,0.9625,0.975,0.9875,1.),.UNSPECIFIED.)
GEOMETRIC_REPRESENTATION_ITEM()
RATIONAL_B_SPLINE_SURFACE(((1.,0.923879532511287,1.,0.923879532511287,1.,
0.923879532511287,1.,0.923879532511287,1.,0.923879532511287,1.,0.923879532511287,
1.,0.923879532511287,1.,0.923879532511287,1.,0.923879532511287,1.,0.923879532511287,
1.,0.923879532511287,1.,0.923879532511287,1.,0.923879532511287,1.,0.923879532511287,
1.,0.923879532511287,1.,0.923879532511287,1.,0.923879532511287,1.,0.923879532511287,
1.,0.923879532511287,1.,0.923879532511287,1.,0.923879532511287,1.,0.923879532511287,
1.,0.923879532511287,1.,0.923879532511287,1.,0.923879532511287,1.,0.923879532511287,
1.,0.923879532511287,1.,0.923879532511287,1.,0.923879532511287,1.,0.923879532511287,
1.,0.923879532511287,1.,0.923879532511287,1.,0.923879532511287,1.,0.923879532511287,
1.,0.923879532511287,1.,0.923879532511287,1.,0.923879532511287,1.,0.923879532511287,
1.,0.923879532511287,1.,0.923879532511287,1.,0.923879532511287,1.,0.923879532511287,
1.,0.923879532511287,1.,0.923879532511287,1.,0.923879532511287,1.,0.923879532511287,
1.,0.923879532511287,1.,0.923879532511287,1.,0.923879532511287,1.,0.923879532511287,
1.,0.923879532511287,1.,0.923879532511287,1.,0.923879532511287,1.,0.923879532511287,
1.,0.923879532511287,1.,0.923879532511287,1.,0.923879532511287,1.,0.923879532511287,
1.,0.923879532511287,1.,0.923879532511287,1.,0.923879532511287,1.,0.923879532511287,
1.,0.923879532511287,1.,0.923879532511287,1.,0.923879532511287,1.,0.923879532511287,
1.,0.923879532511287,1.,0.923879532511287,1.,0.923879532511287,1.,0.923879532511287,
1.,0.923879532511287,1.,0.923879532511287,1.,0.923879532511287,1.,0.923879532511287,
1.,0.923879532511287,1.,0.923879532511287,1.,0.923879532511287,1.,0.923879532511287,
1.,0.923879532511287,1.,0.923879532511287,1.),(1.,0.923879532511287,1.,
0.923879532511287,1.,0.923879532511287,1.,0.923879532511287,1.,0.923879532511287,
1.,0.923879532511287,1.,0.923879532511287,1.,0.923879532511287,1.,0.923879532511287,
1.,0.923879532511287,1.,0.923879532511287,1.,0.923879532511287,1.,0.923879532511287,
1.,0.923879532511287,1.,0.923879532511287,1.,0.923879532511287,1.,0.923879532511287,
1.,0.923879532511287,1.,0.923879532511287,1.,0.923879532511287,1.,0.923879532511287,
1.,0.923879532511287,1.,0.923879532511287,1.,0.923879532511287,1.,0.923879532511287,
1.,0.923879532511287,1.,0.923879532511287,1.,0.923879532511287,1.,0.923879532511287,
1.,0.923879532511287,1.,0.923879532511287,1.,0.923879532511287,1.,0.923879532511287,
1.,0.923879532511287,1.,0.923879532511287,1.,0.923879532511287,1.,0.923879532511287,
1.,0.923879532511287,1.,0.923879532511287,1.,0.923879532511287,1.,0.923879532511287,
1.,0.923879532511287,1.,0.923879532511287,1.,0.923879532511287,1.,0.923879532511287,
1.,0.923879532511287,1.,0.923879532511287,1.,0.923879532511287,1.,0.923879532511287,
1.,0.923879532511287,1.,0.923879532511287,1.,0.923879532511287,1.,0.923879532511287,
1.,0.923879532511287,1.,0.923879532511287,1.,0.923879532511287,1.,0.923879532511287,
1.,0.923879532511287,1.,0.923879532511287,1.,0.923879532511287,1.,0.923879532511287,
1.,0.923879532511287,1.,0.923879532511287,1.,0.923879532511287,1.,0.923879532511287,
1.,0.923879532511287,1.,0.923879532511287,1.,0.923879532511287,1.,0.923879532511287,
1.,0.923879532511287,1.,0.923879532511287,1.,0.923879532511287,1.,0.923879532511287,
1.,0.923879532511287,1.,0.923879532511287,1.,0.923879532511287,1.,0.923879532511287,
1.,0.923879532511287,1.,0.923879532511287,1.,0.923879532511287,1.)))
REPRESENTATION_ITEM('')
SURFACE()
);
#570=(
BOUNDED_SURFACE()
B_SPLINE_SURFACE(1,2,((#26345,#26346,#26347,#26348,#26349,#26350,#26351,
#26352,#26353,#26354,#26355,#26356,#26357,#26358,#26359,#26360,#26361,#26362,
#26363,#26364,#26365,#26366,#26367,#26368,#26369,#26370,#26371,#26372,#26373,
#26374,#26375,#26376,#26377,#26378,#26379,#26380,#26381,#26382,#26383,#26384,
#26385,#26386,#26387,#26388,#26389,#26390,#26391,#26392,#26393,#26394,#26395,
#26396,#26397,#26398,#26399,#26400,#26401,#26402,#26403,#26404,#26405,#26406,
#26407,#26408,#26409,#26410,#26411,#26412,#26413,#26414,#26415,#26416,#26417,
#26418,#26419,#26420,#26421,#26422,#26423,#26424,#26425,#26426,#26427,#26428,
#26429,#26430,#26431,#26432,#26433,#26434,#26435,#26436,#26437,#26438,#26439,
#26440,#26441,#26442,#26443,#26444,#26445,#26446,#26447,#26448,#26449,#26450,
#26451,#26452,#26453,#26454,#26455,#26456,#26457,#26458,#26459,#26460,#26461,
#26462,#26463,#26464,#26465,#26466,#26467,#26468,#26469,#26470,#26471,#26472,
#26473,#26474,#26475,#26476,#26477,#26478,#26479,#26480,#26481,#26482,#26483,
#26484,#26485,#26486,#26487,#26488,#26489,#26490,#26491,#26492,#26493,#26494,
#26495,#26496,#26497,#26498,#26499,#26500,#26501,#26502,#26503,#26504,#26505),
(#26506,#26507,#26508,#26509,#26510,#26511,#26512,#26513,#26514,#26515,
#26516,#26517,#26518,#26519,#26520,#26521,#26522,#26523,#26524,#26525,#26526,
#26527,#26528,#26529,#26530,#26531,#26532,#26533,#26534,#26535,#26536,#26537,
#26538,#26539,#26540,#26541,#26542,#26543,#26544,#26545,#26546,#26547,#26548,
#26549,#26550,#26551,#26552,#26553,#26554,#26555,#26556,#26557,#26558,#26559,
#26560,#26561,#26562,#26563,#26564,#26565,#26566,#26567,#26568,#26569,#26570,
#26571,#26572,#26573,#26574,#26575,#26576,#26577,#26578,#26579,#26580,#26581,
#26582,#26583,#26584,#26585,#26586,#26587,#26588,#26589,#26590,#26591,#26592,
#26593,#26594,#26595,#26596,#26597,#26598,#26599,#26600,#26601,#26602,#26603,
#26604,#26605,#26606,#26607,#26608,#26609,#26610,#26611,#26612,#26613,#26614,
#26615,#26616,#26617,#26618,#26619,#26620,#26621,#26622,#26623,#26624,#26625,
#26626,#26627,#26628,#26629,#26630,#26631,#26632,#26633,#26634,#26635,#26636,
#26637,#26638,#26639,#26640,#26641,#26642,#26643,#26644,#26645,#26646,#26647,
#26648,#26649,#26650,#26651,#26652,#26653,#26654,#26655,#26656,#26657,#26658,
#26659,#26660,#26661,#26662,#26663,#26664,#26665,#26666)),.UNSPECIFIED.,
 .F.,.F.,.F.)
B_SPLINE_SURFACE_WITH_KNOTS((2,2),(3,2,2,2,2,2,2,2,2,2,2,2,2,2,2,2,2,2,
2,2,2,2,2,2,2,2,2,2,2,2,2,2,2,2,2,2,2,2,2,2,2,2,2,2,2,2,2,2,2,2,2,2,2,2,
2,2,2,2,2,2,2,2,2,2,2,2,2,2,2,2,2,2,2,2,2,2,2,2,2,2,3),(0.,1.),(0.,0.0125,
0.025,0.0375,0.05,0.0625,0.075,0.0875,0.1,0.1125,0.125,0.1375,0.15,0.1625,
0.175,0.1875,0.2,0.2125,0.225,0.2375,0.25,0.2625,0.275,0.2875,0.3,0.3125,
0.325,0.3375,0.35,0.3625,0.375,0.3875,0.4,0.4125,0.425,0.4375,0.45,0.4625,
0.475,0.4875,0.5,0.5125,0.525,0.5375,0.55,0.5625,0.575,0.5875,0.6,0.6125,
0.625,0.6375,0.65,0.6625,0.675,0.6875,0.7,0.7125,0.725,0.7375,0.75,0.7625,
0.775,0.7875,0.8,0.8125,0.825,0.8375,0.85,0.8625,0.875,0.8875,0.9,0.9125,
0.925,0.9375,0.95,0.9625,0.975,0.9875,1.),.UNSPECIFIED.)
GEOMETRIC_REPRESENTATION_ITEM()
RATIONAL_B_SPLINE_SURFACE(((1.,0.923879532511287,1.,0.923879532511287,1.,
0.923879532511287,1.,0.923879532511287,1.,0.923879532511287,1.,0.923879532511287,
1.,0.923879532511287,1.,0.923879532511287,1.,0.923879532511287,1.,0.923879532511287,
1.,0.923879532511287,1.,0.923879532511287,1.,0.923879532511287,1.,0.923879532511287,
1.,0.923879532511287,1.,0.923879532511287,1.,0.923879532511287,1.,0.923879532511287,
1.,0.923879532511287,1.,0.923879532511287,1.,0.923879532511287,1.,0.923879532511287,
1.,0.923879532511287,1.,0.923879532511287,1.,0.923879532511287,1.,0.923879532511287,
1.,0.923879532511287,1.,0.923879532511287,1.,0.923879532511287,1.,0.923879532511287,
1.,0.923879532511287,1.,0.923879532511287,1.,0.923879532511287,1.,0.923879532511287,
1.,0.923879532511287,1.,0.923879532511287,1.,0.923879532511287,1.,0.923879532511287,
1.,0.923879532511287,1.,0.923879532511287,1.,0.923879532511287,1.,0.923879532511287,
1.,0.923879532511287,1.,0.923879532511287,1.,0.923879532511287,1.,0.923879532511287,
1.,0.923879532511287,1.,0.923879532511287,1.,0.923879532511287,1.,0.923879532511287,
1.,0.923879532511287,1.,0.923879532511287,1.,0.923879532511287,1.,0.923879532511287,
1.,0.923879532511287,1.,0.923879532511287,1.,0.923879532511287,1.,0.923879532511287,
1.,0.923879532511287,1.,0.923879532511287,1.,0.923879532511287,1.,0.923879532511287,
1.,0.923879532511287,1.,0.923879532511287,1.,0.923879532511287,1.,0.923879532511287,
1.,0.923879532511287,1.,0.923879532511287,1.,0.923879532511287,1.,0.923879532511287,
1.,0.923879532511287,1.,0.923879532511287,1.,0.923879532511287,1.,0.923879532511287,
1.,0.923879532511287,1.,0.923879532511287,1.,0.923879532511287,1.,0.923879532511287,
1.,0.923879532511287,1.,0.923879532511287,1.),(1.,0.923879532511287,1.,
0.923879532511287,1.,0.923879532511287,1.,0.923879532511287,1.,0.923879532511287,
1.,0.923879532511287,1.,0.923879532511287,1.,0.923879532511287,1.,0.923879532511287,
1.,0.923879532511287,1.,0.923879532511287,1.,0.923879532511287,1.,0.923879532511287,
1.,0.923879532511287,1.,0.923879532511287,1.,0.923879532511287,1.,0.923879532511287,
1.,0.923879532511287,1.,0.923879532511287,1.,0.923879532511287,1.,0.923879532511287,
1.,0.923879532511287,1.,0.923879532511287,1.,0.923879532511287,1.,0.923879532511287,
1.,0.923879532511287,1.,0.923879532511287,1.,0.923879532511287,1.,0.923879532511287,
1.,0.923879532511287,1.,0.923879532511287,1.,0.923879532511287,1.,0.923879532511287,
1.,0.923879532511287,1.,0.923879532511287,1.,0.923879532511287,1.,0.923879532511287,
1.,0.923879532511287,1.,0.923879532511287,1.,0.923879532511287,1.,0.923879532511287,
1.,0.923879532511287,1.,0.923879532511287,1.,0.923879532511287,1.,0.923879532511287,
1.,0.923879532511287,1.,0.923879532511287,1.,0.923879532511287,1.,0.923879532511287,
1.,0.923879532511287,1.,0.923879532511287,1.,0.923879532511287,1.,0.923879532511287,
1.,0.923879532511287,1.,0.923879532511287,1.,0.923879532511287,1.,0.923879532511287,
1.,0.923879532511287,1.,0.923879532511287,1.,0.923879532511287,1.,0.923879532511287,
1.,0.923879532511287,1.,0.923879532511287,1.,0.923879532511287,1.,0.923879532511287,
1.,0.923879532511287,1.,0.923879532511287,1.,0.923879532511287,1.,0.923879532511287,
1.,0.923879532511287,1.,0.923879532511287,1.,0.923879532511287,1.,0.923879532511287,
1.,0.923879532511287,1.,0.923879532511287,1.,0.923879532511287,1.,0.923879532511287,
1.,0.923879532511287,1.,0.923879532511287,1.,0.923879532511287,1.)))
REPRESENTATION_ITEM('')
SURFACE()
);
#571=(
BOUNDED_SURFACE()
B_SPLINE_SURFACE(3,2,((#26684,#26685,#26686,#26687,#26688,#26689,#26690,
#26691,#26692,#26693,#26694,#26695,#26696,#26697,#26698,#26699,#26700,#26701,
#26702,#26703,#26704,#26705,#26706,#26707,#26708,#26709,#26710,#26711,#26712,
#26713,#26714,#26715,#26716,#26717,#26718,#26719,#26720,#26721,#26722,#26723,
#26724,#26725,#26726,#26727,#26728,#26729,#26730,#26731,#26732,#26733,#26734,
#26735,#26736,#26737,#26738,#26739,#26740,#26741,#26742,#26743,#26744,#26745,
#26746,#26747,#26748,#26749,#26750,#26751,#26752,#26753,#26754,#26755,#26756,
#26757,#26758,#26759,#26760,#26761,#26762,#26763,#26764,#26765,#26766,#26767,
#26768,#26769,#26770,#26771,#26772,#26773,#26774,#26775,#26776,#26777,#26778,
#26779,#26780,#26781,#26782,#26783,#26784,#26785,#26786,#26787,#26788,#26789,
#26790,#26791,#26792,#26793,#26794,#26795,#26796,#26797,#26798,#26799,#26800,
#26801,#26802,#26803,#26804,#26805,#26806,#26807,#26808,#26809,#26810,#26811,
#26812,#26813,#26814,#26815,#26816,#26817,#26818,#26819,#26820,#26821,#26822,
#26823,#26824,#26825,#26826,#26827,#26828,#26829,#26830,#26831,#26832,#26833,
#26834,#26835,#26836,#26837,#26838,#26839,#26840,#26841,#26842,#26843,#26844),
(#26845,#26846,#26847,#26848,#26849,#26850,#26851,#26852,#26853,#26854,
#26855,#26856,#26857,#26858,#26859,#26860,#26861,#26862,#26863,#26864,#26865,
#26866,#26867,#26868,#26869,#26870,#26871,#26872,#26873,#26874,#26875,#26876,
#26877,#26878,#26879,#26880,#26881,#26882,#26883,#26884,#26885,#26886,#26887,
#26888,#26889,#26890,#26891,#26892,#26893,#26894,#26895,#26896,#26897,#26898,
#26899,#26900,#26901,#26902,#26903,#26904,#26905,#26906,#26907,#26908,#26909,
#26910,#26911,#26912,#26913,#26914,#26915,#26916,#26917,#26918,#26919,#26920,
#26921,#26922,#26923,#26924,#26925,#26926,#26927,#26928,#26929,#26930,#26931,
#26932,#26933,#26934,#26935,#26936,#26937,#26938,#26939,#26940,#26941,#26942,
#26943,#26944,#26945,#26946,#26947,#26948,#26949,#26950,#26951,#26952,#26953,
#26954,#26955,#26956,#26957,#26958,#26959,#26960,#26961,#26962,#26963,#26964,
#26965,#26966,#26967,#26968,#26969,#26970,#26971,#26972,#26973,#26974,#26975,
#26976,#26977,#26978,#26979,#26980,#26981,#26982,#26983,#26984,#26985,#26986,
#26987,#26988,#26989,#26990,#26991,#26992,#26993,#26994,#26995,#26996,#26997,
#26998,#26999,#27000,#27001,#27002,#27003,#27004,#27005),(#27006,#27007,
#27008,#27009,#27010,#27011,#27012,#27013,#27014,#27015,#27016,#27017,#27018,
#27019,#27020,#27021,#27022,#27023,#27024,#27025,#27026,#27027,#27028,#27029,
#27030,#27031,#27032,#27033,#27034,#27035,#27036,#27037,#27038,#27039,#27040,
#27041,#27042,#27043,#27044,#27045,#27046,#27047,#27048,#27049,#27050,#27051,
#27052,#27053,#27054,#27055,#27056,#27057,#27058,#27059,#27060,#27061,#27062,
#27063,#27064,#27065,#27066,#27067,#27068,#27069,#27070,#27071,#27072,#27073,
#27074,#27075,#27076,#27077,#27078,#27079,#27080,#27081,#27082,#27083,#27084,
#27085,#27086,#27087,#27088,#27089,#27090,#27091,#27092,#27093,#27094,#27095,
#27096,#27097,#27098,#27099,#27100,#27101,#27102,#27103,#27104,#27105,#27106,
#27107,#27108,#27109,#27110,#27111,#27112,#27113,#27114,#27115,#27116,#27117,
#27118,#27119,#27120,#27121,#27122,#27123,#27124,#27125,#27126,#27127,#27128,
#27129,#27130,#27131,#27132,#27133,#27134,#27135,#27136,#27137,#27138,#27139,
#27140,#27141,#27142,#27143,#27144,#27145,#27146,#27147,#27148,#27149,#27150,
#27151,#27152,#27153,#27154,#27155,#27156,#27157,#27158,#27159,#27160,#27161,
#27162,#27163,#27164,#27165,#27166),(#27167,#27168,#27169,#27170,#27171,
#27172,#27173,#27174,#27175,#27176,#27177,#27178,#27179,#27180,#27181,#27182,
#27183,#27184,#27185,#27186,#27187,#27188,#27189,#27190,#27191,#27192,#27193,
#27194,#27195,#27196,#27197,#27198,#27199,#27200,#27201,#27202,#27203,#27204,
#27205,#27206,#27207,#27208,#27209,#27210,#27211,#27212,#27213,#27214,#27215,
#27216,#27217,#27218,#27219,#27220,#27221,#27222,#27223,#27224,#27225,#27226,
#27227,#27228,#27229,#27230,#27231,#27232,#27233,#27234,#27235,#27236,#27237,
#27238,#27239,#27240,#27241,#27242,#27243,#27244,#27245,#27246,#27247,#27248,
#27249,#27250,#27251,#27252,#27253,#27254,#27255,#27256,#27257,#27258,#27259,
#27260,#27261,#27262,#27263,#27264,#27265,#27266,#27267,#27268,#27269,#27270,
#27271,#27272,#27273,#27274,#27275,#27276,#27277,#27278,#27279,#27280,#27281,
#27282,#27283,#27284,#27285,#27286,#27287,#27288,#27289,#27290,#27291,#27292,
#27293,#27294,#27295,#27296,#27297,#27298,#27299,#27300,#27301,#27302,#27303,
#27304,#27305,#27306,#27307,#27308,#27309,#27310,#27311,#27312,#27313,#27314,
#27315,#27316,#27317,#27318,#27319,#27320,#27321,#27322,#27323,#27324,#27325,
#27326,#27327)),.UNSPECIFIED.,.F.,.F.,.F.)
B_SPLINE_SURFACE_WITH_KNOTS((4,4),(3,2,2,2,2,2,2,2,2,2,2,2,2,2,2,2,2,2,
2,2,2,2,2,2,2,2,2,2,2,2,2,2,2,2,2,2,2,2,2,2,2,2,2,2,2,2,2,2,2,2,2,2,2,2,
2,2,2,2,2,2,2,2,2,2,2,2,2,2,2,2,2,2,2,2,2,2,2,2,2,2,3),(0.,1.),(0.,0.0125,
0.025,0.0375,0.05,0.0625,0.075,0.0875,0.1,0.1125,0.125,0.1375,0.15,0.1625,
0.175,0.1875,0.2,0.2125,0.225,0.2375,0.25,0.2625,0.275,0.2875,0.3,0.3125,
0.325,0.3375,0.35,0.3625,0.375,0.3875,0.4,0.4125,0.425,0.4375,0.45,0.4625,
0.475,0.4875,0.5,0.5125,0.525,0.5375,0.55,0.5625,0.575,0.5875,0.6,0.6125,
0.625,0.6375,0.65,0.6625,0.675,0.6875,0.7,0.7125,0.725,0.7375,0.75,0.7625,
0.775,0.7875,0.8,0.8125,0.825,0.8375,0.85,0.8625,0.875,0.8875,0.9,0.9125,
0.925,0.9375,0.95,0.9625,0.975,0.9875,1.),.UNSPECIFIED.)
GEOMETRIC_REPRESENTATION_ITEM()
RATIONAL_B_SPLINE_SURFACE(((1.,0.923879532511287,1.,0.923879532511287,1.,
0.923879532511287,1.,0.923879532511287,1.,0.923879532511287,1.,0.923879532511287,
1.,0.923879532511287,1.,0.923879532511287,1.,0.923879532511287,1.,0.923879532511287,
1.,0.923879532511287,1.,0.923879532511287,1.,0.923879532511287,1.,0.923879532511287,
1.,0.923879532511287,1.,0.923879532511287,1.,0.923879532511287,1.,0.923879532511287,
1.,0.923879532511287,1.,0.923879532511287,1.,0.923879532511287,1.,0.923879532511287,
1.,0.923879532511287,1.,0.923879532511287,1.,0.923879532511287,1.,0.923879532511287,
1.,0.923879532511287,1.,0.923879532511287,1.,0.923879532511287,1.,0.923879532511287,
1.,0.923879532511287,1.,0.923879532511287,1.,0.923879532511287,1.,0.923879532511287,
1.,0.923879532511287,1.,0.923879532511287,1.,0.923879532511287,1.,0.923879532511287,
1.,0.923879532511287,1.,0.923879532511287,1.,0.923879532511287,1.,0.923879532511287,
1.,0.923879532511287,1.,0.923879532511287,1.,0.923879532511287,1.,0.923879532511287,
1.,0.923879532511287,1.,0.923879532511287,1.,0.923879532511287,1.,0.923879532511287,
1.,0.923879532511287,1.,0.923879532511287,1.,0.923879532511287,1.,0.923879532511287,
1.,0.923879532511287,1.,0.923879532511287,1.,0.923879532511287,1.,0.923879532511287,
1.,0.923879532511287,1.,0.923879532511287,1.,0.923879532511287,1.,0.923879532511287,
1.,0.923879532511287,1.,0.923879532511287,1.,0.923879532511287,1.,0.923879532511287,
1.,0.923879532511287,1.,0.923879532511287,1.,0.923879532511287,1.,0.923879532511287,
1.,0.923879532511287,1.,0.923879532511287,1.,0.923879532511287,1.,0.923879532511287,
1.,0.923879532511287,1.,0.923879532511287,1.,0.923879532511287,1.,0.923879532511287,
1.,0.923879532511287,1.,0.923879532511287,1.),(0.998696642611305,0.922675387296324,
0.998696642611305,0.922675387296324,0.998696642611305,0.922675387296324,
0.998696642611305,0.922675387296324,0.998696642611305,0.922675387296324,
0.998696642611305,0.922675387296324,0.998696642611305,0.922675387296324,
0.998696642611305,0.922675387296324,0.998696642611305,0.922675387296324,
0.998696642611305,0.922675387296324,0.998696642611305,0.922675387296324,
0.998696642611305,0.922675387296324,0.998696642611305,0.922675387296324,
0.998696642611305,0.922675387296324,0.998696642611305,0.922675387296324,
0.998696642611305,0.922675387296324,0.998696642611305,0.922675387296324,
0.998696642611305,0.922675387296324,0.998696642611305,0.922675387296324,
0.998696642611305,0.922675387296324,0.998696642611305,0.922675387296324,
0.998696642611305,0.922675387296324,0.998696642611305,0.922675387296324,
0.998696642611305,0.922675387296324,0.998696642611305,0.922675387296324,
0.998696642611305,0.922675387296324,0.998696642611305,0.922675387296324,
0.998696642611305,0.922675387296324,0.998696642611305,0.922675387296324,
0.998696642611305,0.922675387296324,0.998696642611305,0.922675387296324,
0.998696642611305,0.922675387296324,0.998696642611305,0.922675387296324,
0.998696642611305,0.922675387296324,0.998696642611305,0.922675387296324,
0.998696642611305,0.922675387296324,0.998696642611305,0.922675387296324,
0.998696642611305,0.922675387296324,0.998696642611305,0.922675387296324,
0.998696642611305,0.922675387296324,0.998696642611305,0.922675387296324,
0.998696642611305,0.922675387296324,0.998696642611305,0.922675387296324,
0.998696642611305,0.922675387296324,0.998696642611305,0.922675387296324,
0.998696642611305,0.922675387296324,0.998696642611305,0.922675387296324,
0.998696642611305,0.922675387296324,0.998696642611305,0.922675387296324,
0.998696642611305,0.922675387296324,0.998696642611305,0.922675387296324,
0.998696642611305,0.922675387296324,0.998696642611305,0.922675387296324,
0.998696642611305,0.922675387296324,0.998696642611305,0.922675387296324,
0.998696642611305,0.922675387296324,0.998696642611305,0.922675387296324,
0.998696642611305,0.922675387296324,0.998696642611305,0.922675387296324,
0.998696642611305,0.922675387296324,0.998696642611305,0.922675387296324,
0.998696642611305,0.922675387296324,0.998696642611305,0.922675387296324,
0.998696642611305,0.922675387296324,0.998696642611305,0.922675387296324,
0.998696642611305,0.922675387296324,0.998696642611305,0.922675387296324,
0.998696642611305,0.922675387296324,0.998696642611305,0.922675387296324,
0.998696642611305,0.922675387296324,0.998696642611305,0.922675387296324,
0.998696642611305,0.922675387296324,0.998696642611305,0.922675387296324,
0.998696642611305,0.922675387296324,0.998696642611305,0.922675387296324,
0.998696642611305,0.922675387296324,0.998696642611305,0.922675387296324,
0.998696642611305,0.922675387296324,0.998696642611305,0.922675387296324,
0.998696642611305,0.922675387296324,0.998696642611305),(0.998696642611305,
0.922675387296324,0.998696642611305,0.922675387296324,0.998696642611305,
0.922675387296324,0.998696642611305,0.922675387296324,0.998696642611305,
0.922675387296324,0.998696642611305,0.922675387296324,0.998696642611305,
0.922675387296324,0.998696642611305,0.922675387296324,0.998696642611305,
0.922675387296324,0.998696642611305,0.922675387296324,0.998696642611305,
0.922675387296324,0.998696642611305,0.922675387296324,0.998696642611305,
0.922675387296324,0.998696642611305,0.922675387296324,0.998696642611305,
0.922675387296324,0.998696642611305,0.922675387296324,0.998696642611305,
0.922675387296324,0.998696642611305,0.922675387296324,0.998696642611305,
0.922675387296324,0.998696642611305,0.922675387296324,0.998696642611305,
0.922675387296324,0.998696642611305,0.922675387296324,0.998696642611305,
0.922675387296324,0.998696642611305,0.922675387296324,0.998696642611305,
0.922675387296324,0.998696642611305,0.922675387296324,0.998696642611305,
0.922675387296324,0.998696642611305,0.922675387296324,0.998696642611305,
0.922675387296324,0.998696642611305,0.922675387296324,0.998696642611305,
0.922675387296324,0.998696642611305,0.922675387296324,0.998696642611305,
0.922675387296324,0.998696642611305,0.922675387296324,0.998696642611305,
0.922675387296324,0.998696642611305,0.922675387296324,0.998696642611305,
0.922675387296324,0.998696642611305,0.922675387296324,0.998696642611305,
0.922675387296324,0.998696642611305,0.922675387296324,0.998696642611305,
0.922675387296324,0.998696642611305,0.922675387296324,0.998696642611305,
0.922675387296324,0.998696642611305,0.922675387296324,0.998696642611305,
0.922675387296324,0.998696642611305,0.922675387296324,0.998696642611305,
0.922675387296324,0.998696642611305,0.922675387296324,0.998696642611305,
0.922675387296324,0.998696642611305,0.922675387296324,0.998696642611305,
0.922675387296324,0.998696642611305,0.922675387296324,0.998696642611305,
0.922675387296324,0.998696642611305,0.922675387296324,0.998696642611305,
0.922675387296324,0.998696642611305,0.922675387296324,0.998696642611305,
0.922675387296324,0.998696642611305,0.922675387296324,0.998696642611305,
0.922675387296324,0.998696642611305,0.922675387296324,0.998696642611305,
0.922675387296324,0.998696642611305,0.922675387296324,0.998696642611305,
0.922675387296324,0.998696642611305,0.922675387296324,0.998696642611305,
0.922675387296324,0.998696642611305,0.922675387296324,0.998696642611305,
0.922675387296324,0.998696642611305,0.922675387296324,0.998696642611305,
0.922675387296324,0.998696642611305,0.922675387296324,0.998696642611305,
0.922675387296324,0.998696642611305,0.922675387296324,0.998696642611305,
0.922675387296324,0.998696642611305,0.922675387296324,0.998696642611305,
0.922675387296324,0.998696642611305,0.922675387296324,0.998696642611305,
0.922675387296324,0.998696642611305,0.922675387296324,0.998696642611305,
0.922675387296324,0.998696642611305,0.922675387296324,0.998696642611305),
(1.,0.923879532511287,1.,0.923879532511287,1.,0.923879532511287,1.,0.923879532511287,
1.,0.923879532511287,1.,0.923879532511287,1.,0.923879532511287,1.,0.923879532511287,
1.,0.923879532511287,1.,0.923879532511287,1.,0.923879532511287,1.,0.923879532511287,
1.,0.923879532511287,1.,0.923879532511287,1.,0.923879532511287,1.,0.923879532511287,
1.,0.923879532511287,1.,0.923879532511287,1.,0.923879532511287,1.,0.923879532511287,
1.,0.923879532511287,1.,0.923879532511287,1.,0.923879532511287,1.,0.923879532511287,
1.,0.923879532511287,1.,0.923879532511287,1.,0.923879532511287,1.,0.923879532511287,
1.,0.923879532511287,1.,0.923879532511287,1.,0.923879532511287,1.,0.923879532511287,
1.,0.923879532511287,1.,0.923879532511287,1.,0.923879532511287,1.,0.923879532511287,
1.,0.923879532511287,1.,0.923879532511287,1.,0.923879532511287,1.,0.923879532511287,
1.,0.923879532511287,1.,0.923879532511287,1.,0.923879532511287,1.,0.923879532511287,
1.,0.923879532511287,1.,0.923879532511287,1.,0.923879532511287,1.,0.923879532511287,
1.,0.923879532511287,1.,0.923879532511287,1.,0.923879532511287,1.,0.923879532511287,
1.,0.923879532511287,1.,0.923879532511287,1.,0.923879532511287,1.,0.923879532511287,
1.,0.923879532511287,1.,0.923879532511287,1.,0.923879532511287,1.,0.923879532511287,
1.,0.923879532511287,1.,0.923879532511287,1.,0.923879532511287,1.,0.923879532511287,
1.,0.923879532511287,1.,0.923879532511287,1.,0.923879532511287,1.,0.923879532511287,
1.,0.923879532511287,1.,0.923879532511287,1.,0.923879532511287,1.,0.923879532511287,
1.,0.923879532511287,1.,0.923879532511287,1.,0.923879532511287,1.,0.923879532511287,
1.,0.923879532511287,1.,0.923879532511287,1.,0.923879532511287,1.,0.923879532511287,
1.)))
REPRESENTATION_ITEM('')
SURFACE()
);
#572=(
BOUNDED_SURFACE()
B_SPLINE_SURFACE(1,2,((#27328,#27329,#27330,#27331,#27332,#27333,#27334,
#27335,#27336,#27337,#27338,#27339,#27340,#27341,#27342,#27343,#27344,#27345,
#27346,#27347,#27348,#27349,#27350,#27351,#27352,#27353,#27354,#27355,#27356,
#27357,#27358,#27359,#27360,#27361,#27362,#27363,#27364,#27365,#27366,#27367,
#27368,#27369,#27370,#27371,#27372,#27373,#27374,#27375,#27376,#27377,#27378,
#27379,#27380,#27381,#27382,#27383,#27384,#27385,#27386,#27387,#27388,#27389,
#27390,#27391,#27392,#27393,#27394,#27395,#27396,#27397,#27398,#27399,#27400,
#27401,#27402,#27403,#27404,#27405,#27406,#27407,#27408,#27409,#27410,#27411,
#27412,#27413,#27414,#27415,#27416,#27417,#27418,#27419,#27420,#27421,#27422,
#27423,#27424,#27425,#27426,#27427,#27428,#27429,#27430,#27431,#27432,#27433,
#27434,#27435,#27436,#27437,#27438,#27439,#27440,#27441,#27442,#27443,#27444,
#27445,#27446,#27447,#27448,#27449,#27450,#27451,#27452,#27453,#27454,#27455,
#27456,#27457,#27458,#27459,#27460,#27461,#27462,#27463,#27464,#27465,#27466,
#27467,#27468,#27469,#27470,#27471,#27472,#27473,#27474,#27475,#27476,#27477,
#27478,#27479,#27480,#27481,#27482,#27483,#27484,#27485,#27486,#27487,#27488),
(#27489,#27490,#27491,#27492,#27493,#27494,#27495,#27496,#27497,#27498,
#27499,#27500,#27501,#27502,#27503,#27504,#27505,#27506,#27507,#27508,#27509,
#27510,#27511,#27512,#27513,#27514,#27515,#27516,#27517,#27518,#27519,#27520,
#27521,#27522,#27523,#27524,#27525,#27526,#27527,#27528,#27529,#27530,#27531,
#27532,#27533,#27534,#27535,#27536,#27537,#27538,#27539,#27540,#27541,#27542,
#27543,#27544,#27545,#27546,#27547,#27548,#27549,#27550,#27551,#27552,#27553,
#27554,#27555,#27556,#27557,#27558,#27559,#27560,#27561,#27562,#27563,#27564,
#27565,#27566,#27567,#27568,#27569,#27570,#27571,#27572,#27573,#27574,#27575,
#27576,#27577,#27578,#27579,#27580,#27581,#27582,#27583,#27584,#27585,#27586,
#27587,#27588,#27589,#27590,#27591,#27592,#27593,#27594,#27595,#27596,#27597,
#27598,#27599,#27600,#27601,#27602,#27603,#27604,#27605,#27606,#27607,#27608,
#27609,#27610,#27611,#27612,#27613,#27614,#27615,#27616,#27617,#27618,#27619,
#27620,#27621,#27622,#27623,#27624,#27625,#27626,#27627,#27628,#27629,#27630,
#27631,#27632,#27633,#27634,#27635,#27636,#27637,#27638,#27639,#27640,#27641,
#27642,#27643,#27644,#27645,#27646,#27647,#27648,#27649)),.UNSPECIFIED.,
 .F.,.F.,.F.)
B_SPLINE_SURFACE_WITH_KNOTS((2,2),(3,2,2,2,2,2,2,2,2,2,2,2,2,2,2,2,2,2,
2,2,2,2,2,2,2,2,2,2,2,2,2,2,2,2,2,2,2,2,2,2,2,2,2,2,2,2,2,2,2,2,2,2,2,2,
2,2,2,2,2,2,2,2,2,2,2,2,2,2,2,2,2,2,2,2,2,2,2,2,2,2,3),(0.,1.),(0.,0.0125,
0.025,0.0375,0.05,0.0625,0.075,0.0875,0.1,0.1125,0.125,0.1375,0.15,0.1625,
0.175,0.1875,0.2,0.2125,0.225,0.2375,0.25,0.2625,0.275,0.2875,0.3,0.3125,
0.325,0.3375,0.35,0.3625,0.375,0.3875,0.4,0.4125,0.425,0.4375,0.45,0.4625,
0.475,0.4875,0.5,0.5125,0.525,0.5375,0.55,0.5625,0.575,0.5875,0.6,0.6125,
0.625,0.6375,0.65,0.6625,0.675,0.6875,0.7,0.7125,0.725,0.7375,0.75,0.7625,
0.775,0.7875,0.8,0.8125,0.825,0.8375,0.85,0.8625,0.875,0.8875,0.9,0.9125,
0.925,0.9375,0.95,0.9625,0.975,0.9875,1.),.UNSPECIFIED.)
GEOMETRIC_REPRESENTATION_ITEM()
RATIONAL_B_SPLINE_SURFACE(((1.,0.923879532511287,1.,0.923879532511287,1.,
0.923879532511287,1.,0.923879532511287,1.,0.923879532511287,1.,0.923879532511287,
1.,0.923879532511287,1.,0.923879532511287,1.,0.923879532511287,1.,0.923879532511287,
1.,0.923879532511287,1.,0.923879532511287,1.,0.923879532511287,1.,0.923879532511287,
1.,0.923879532511287,1.,0.923879532511287,1.,0.923879532511287,1.,0.923879532511287,
1.,0.923879532511287,1.,0.923879532511287,1.,0.923879532511287,1.,0.923879532511287,
1.,0.923879532511287,1.,0.923879532511287,1.,0.923879532511287,1.,0.923879532511287,
1.,0.923879532511287,1.,0.923879532511287,1.,0.923879532511287,1.,0.923879532511287,
1.,0.923879532511287,1.,0.923879532511287,1.,0.923879532511287,1.,0.923879532511287,
1.,0.923879532511287,1.,0.923879532511287,1.,0.923879532511287,1.,0.923879532511287,
1.,0.923879532511287,1.,0.923879532511287,1.,0.923879532511287,1.,0.923879532511287,
1.,0.923879532511287,1.,0.923879532511287,1.,0.923879532511287,1.,0.923879532511287,
1.,0.923879532511287,1.,0.923879532511287,1.,0.923879532511287,1.,0.923879532511287,
1.,0.923879532511287,1.,0.923879532511287,1.,0.923879532511287,1.,0.923879532511287,
1.,0.923879532511287,1.,0.923879532511287,1.,0.923879532511287,1.,0.923879532511287,
1.,0.923879532511287,1.,0.923879532511287,1.,0.923879532511287,1.,0.923879532511287,
1.,0.923879532511287,1.,0.923879532511287,1.,0.923879532511287,1.,0.923879532511287,
1.,0.923879532511287,1.,0.923879532511287,1.,0.923879532511287,1.,0.923879532511287,
1.,0.923879532511287,1.,0.923879532511287,1.,0.923879532511287,1.,0.923879532511287,
1.,0.923879532511287,1.,0.923879532511287,1.,0.923879532511287,1.,0.923879532511287,
1.,0.923879532511287,1.,0.923879532511287,1.),(1.,0.923879532511287,1.,
0.923879532511287,1.,0.923879532511287,1.,0.923879532511287,1.,0.923879532511287,
1.,0.923879532511287,1.,0.923879532511287,1.,0.923879532511287,1.,0.923879532511287,
1.,0.923879532511287,1.,0.923879532511287,1.,0.923879532511287,1.,0.923879532511287,
1.,0.923879532511287,1.,0.923879532511287,1.,0.923879532511287,1.,0.923879532511287,
1.,0.923879532511287,1.,0.923879532511287,1.,0.923879532511287,1.,0.923879532511287,
1.,0.923879532511287,1.,0.923879532511287,1.,0.923879532511287,1.,0.923879532511287,
1.,0.923879532511287,1.,0.923879532511287,1.,0.923879532511287,1.,0.923879532511287,
1.,0.923879532511287,1.,0.923879532511287,1.,0.923879532511287,1.,0.923879532511287,
1.,0.923879532511287,1.,0.923879532511287,1.,0.923879532511287,1.,0.923879532511287,
1.,0.923879532511287,1.,0.923879532511287,1.,0.923879532511287,1.,0.923879532511287,
1.,0.923879532511287,1.,0.923879532511287,1.,0.923879532511287,1.,0.923879532511287,
1.,0.923879532511287,1.,0.923879532511287,1.,0.923879532511287,1.,0.923879532511287,
1.,0.923879532511287,1.,0.923879532511287,1.,0.923879532511287,1.,0.923879532511287,
1.,0.923879532511287,1.,0.923879532511287,1.,0.923879532511287,1.,0.923879532511287,
1.,0.923879532511287,1.,0.923879532511287,1.,0.923879532511287,1.,0.923879532511287,
1.,0.923879532511287,1.,0.923879532511287,1.,0.923879532511287,1.,0.923879532511287,
1.,0.923879532511287,1.,0.923879532511287,1.,0.923879532511287,1.,0.923879532511287,
1.,0.923879532511287,1.,0.923879532511287,1.,0.923879532511287,1.,0.923879532511287,
1.,0.923879532511287,1.,0.923879532511287,1.,0.923879532511287,1.,0.923879532511287,
1.,0.923879532511287,1.,0.923879532511287,1.,0.923879532511287,1.)))
REPRESENTATION_ITEM('')
SURFACE()
);
#573=(
BOUNDED_SURFACE()
B_SPLINE_SURFACE(1,2,((#27667,#27668,#27669,#27670,#27671,#27672,#27673,
#27674,#27675,#27676,#27677,#27678,#27679,#27680,#27681,#27682,#27683,#27684,
#27685,#27686,#27687,#27688,#27689,#27690,#27691,#27692,#27693,#27694,#27695,
#27696,#27697,#27698,#27699,#27700,#27701,#27702,#27703,#27704,#27705,#27706,
#27707,#27708,#27709,#27710,#27711,#27712,#27713,#27714,#27715,#27716,#27717,
#27718,#27719,#27720,#27721,#27722,#27723,#27724,#27725,#27726,#27727,#27728,
#27729,#27730,#27731,#27732,#27733,#27734,#27735,#27736,#27737,#27738,#27739,
#27740,#27741,#27742,#27743,#27744,#27745,#27746,#27747,#27748,#27749,#27750,
#27751,#27752,#27753,#27754,#27755,#27756,#27757,#27758,#27759,#27760,#27761,
#27762,#27763,#27764,#27765,#27766,#27767,#27768,#27769,#27770,#27771,#27772,
#27773,#27774,#27775,#27776,#27777,#27778,#27779,#27780,#27781,#27782,#27783,
#27784,#27785,#27786,#27787,#27788,#27789,#27790,#27791,#27792,#27793,#27794,
#27795,#27796,#27797,#27798,#27799,#27800,#27801,#27802,#27803,#27804,#27805,
#27806,#27807,#27808,#27809,#27810,#27811,#27812,#27813,#27814,#27815,#27816,
#27817,#27818,#27819,#27820,#27821,#27822,#27823,#27824,#27825,#27826,#27827),
(#27828,#27829,#27830,#27831,#27832,#27833,#27834,#27835,#27836,#27837,
#27838,#27839,#27840,#27841,#27842,#27843,#27844,#27845,#27846,#27847,#27848,
#27849,#27850,#27851,#27852,#27853,#27854,#27855,#27856,#27857,#27858,#27859,
#27860,#27861,#27862,#27863,#27864,#27865,#27866,#27867,#27868,#27869,#27870,
#27871,#27872,#27873,#27874,#27875,#27876,#27877,#27878,#27879,#27880,#27881,
#27882,#27883,#27884,#27885,#27886,#27887,#27888,#27889,#27890,#27891,#27892,
#27893,#27894,#27895,#27896,#27897,#27898,#27899,#27900,#27901,#27902,#27903,
#27904,#27905,#27906,#27907,#27908,#27909,#27910,#27911,#27912,#27913,#27914,
#27915,#27916,#27917,#27918,#27919,#27920,#27921,#27922,#27923,#27924,#27925,
#27926,#27927,#27928,#27929,#27930,#27931,#27932,#27933,#27934,#27935,#27936,
#27937,#27938,#27939,#27940,#27941,#27942,#27943,#27944,#27945,#27946,#27947,
#27948,#27949,#27950,#27951,#27952,#27953,#27954,#27955,#27956,#27957,#27958,
#27959,#27960,#27961,#27962,#27963,#27964,#27965,#27966,#27967,#27968,#27969,
#27970,#27971,#27972,#27973,#27974,#27975,#27976,#27977,#27978,#27979,#27980,
#27981,#27982,#27983,#27984,#27985,#27986,#27987,#27988)),.UNSPECIFIED.,
 .F.,.F.,.F.)
B_SPLINE_SURFACE_WITH_KNOTS((2,2),(3,2,2,2,2,2,2,2,2,2,2,2,2,2,2,2,2,2,
2,2,2,2,2,2,2,2,2,2,2,2,2,2,2,2,2,2,2,2,2,2,2,2,2,2,2,2,2,2,2,2,2,2,2,2,
2,2,2,2,2,2,2,2,2,2,2,2,2,2,2,2,2,2,2,2,2,2,2,2,2,2,3),(0.,1.),(0.,0.0125,
0.025,0.0375,0.05,0.0625,0.075,0.0875,0.1,0.1125,0.125,0.1375,0.15,0.1625,
0.175,0.1875,0.2,0.2125,0.225,0.2375,0.25,0.2625,0.275,0.2875,0.3,0.3125,
0.325,0.3375,0.35,0.3625,0.375,0.3875,0.4,0.4125,0.425,0.4375,0.45,0.4625,
0.475,0.4875,0.5,0.5125,0.525,0.5375,0.55,0.5625,0.575,0.5875,0.6,0.6125,
0.625,0.6375,0.65,0.6625,0.675,0.6875,0.7,0.7125,0.725,0.7375,0.75,0.7625,
0.775,0.7875,0.8,0.8125,0.825,0.8375,0.85,0.8625,0.875,0.8875,0.9,0.9125,
0.925,0.9375,0.95,0.9625,0.975,0.9875,1.),.UNSPECIFIED.)
GEOMETRIC_REPRESENTATION_ITEM()
RATIONAL_B_SPLINE_SURFACE(((1.,0.923879532511287,1.,0.923879532511287,1.,
0.923879532511287,1.,0.923879532511287,1.,0.923879532511287,1.,0.923879532511287,
1.,0.923879532511287,1.,0.923879532511287,1.,0.923879532511287,1.,0.923879532511287,
1.,0.923879532511287,1.,0.923879532511287,1.,0.923879532511287,1.,0.923879532511287,
1.,0.923879532511287,1.,0.923879532511287,1.,0.923879532511287,1.,0.923879532511287,
1.,0.923879532511287,1.,0.923879532511287,1.,0.923879532511287,1.,0.923879532511287,
1.,0.923879532511287,1.,0.923879532511287,1.,0.923879532511287,1.,0.923879532511287,
1.,0.923879532511287,1.,0.923879532511287,1.,0.923879532511287,1.,0.923879532511287,
1.,0.923879532511287,1.,0.923879532511287,1.,0.923879532511287,1.,0.923879532511287,
1.,0.923879532511287,1.,0.923879532511287,1.,0.923879532511287,1.,0.923879532511287,
1.,0.923879532511287,1.,0.923879532511287,1.,0.923879532511287,1.,0.923879532511287,
1.,0.923879532511287,1.,0.923879532511287,1.,0.923879532511287,1.,0.923879532511287,
1.,0.923879532511287,1.,0.923879532511287,1.,0.923879532511287,1.,0.923879532511287,
1.,0.923879532511287,1.,0.923879532511287,1.,0.923879532511287,1.,0.923879532511287,
1.,0.923879532511287,1.,0.923879532511287,1.,0.923879532511287,1.,0.923879532511287,
1.,0.923879532511287,1.,0.923879532511287,1.,0.923879532511287,1.,0.923879532511287,
1.,0.923879532511287,1.,0.923879532511287,1.,0.923879532511287,1.,0.923879532511287,
1.,0.923879532511287,1.,0.923879532511287,1.,0.923879532511287,1.,0.923879532511287,
1.,0.923879532511287,1.,0.923879532511287,1.,0.923879532511287,1.,0.923879532511287,
1.,0.923879532511287,1.,0.923879532511287,1.,0.923879532511287,1.,0.923879532511287,
1.,0.923879532511287,1.,0.923879532511287,1.),(1.,0.923879532511287,1.,
0.923879532511287,1.,0.923879532511287,1.,0.923879532511287,1.,0.923879532511287,
1.,0.923879532511287,1.,0.923879532511287,1.,0.923879532511287,1.,0.923879532511287,
1.,0.923879532511287,1.,0.923879532511287,1.,0.923879532511287,1.,0.923879532511287,
1.,0.923879532511287,1.,0.923879532511287,1.,0.923879532511287,1.,0.923879532511287,
1.,0.923879532511287,1.,0.923879532511287,1.,0.923879532511287,1.,0.923879532511287,
1.,0.923879532511287,1.,0.923879532511287,1.,0.923879532511287,1.,0.923879532511287,
1.,0.923879532511287,1.,0.923879532511287,1.,0.923879532511287,1.,0.923879532511287,
1.,0.923879532511287,1.,0.923879532511287,1.,0.923879532511287,1.,0.923879532511287,
1.,0.923879532511287,1.,0.923879532511287,1.,0.923879532511287,1.,0.923879532511287,
1.,0.923879532511287,1.,0.923879532511287,1.,0.923879532511287,1.,0.923879532511287,
1.,0.923879532511287,1.,0.923879532511287,1.,0.923879532511287,1.,0.923879532511287,
1.,0.923879532511287,1.,0.923879532511287,1.,0.923879532511287,1.,0.923879532511287,
1.,0.923879532511287,1.,0.923879532511287,1.,0.923879532511287,1.,0.923879532511287,
1.,0.923879532511287,1.,0.923879532511287,1.,0.923879532511287,1.,0.923879532511287,
1.,0.923879532511287,1.,0.923879532511287,1.,0.923879532511287,1.,0.923879532511287,
1.,0.923879532511287,1.,0.923879532511287,1.,0.923879532511287,1.,0.923879532511287,
1.,0.923879532511287,1.,0.923879532511287,1.,0.923879532511287,1.,0.923879532511287,
1.,0.923879532511287,1.,0.923879532511287,1.,0.923879532511287,1.,0.923879532511287,
1.,0.923879532511287,1.,0.923879532511287,1.,0.923879532511287,1.,0.923879532511287,
1.,0.923879532511287,1.,0.923879532511287,1.,0.923879532511287,1.)))
REPRESENTATION_ITEM('')
SURFACE()
);
#574=(
BOUNDED_SURFACE()
B_SPLINE_SURFACE(3,2,((#28006,#28007,#28008,#28009,#28010,#28011,#28012,
#28013,#28014,#28015,#28016,#28017,#28018,#28019,#28020,#28021,#28022,#28023,
#28024,#28025,#28026,#28027,#28028,#28029,#28030,#28031,#28032,#28033,#28034,
#28035,#28036,#28037,#28038,#28039,#28040,#28041,#28042,#28043,#28044,#28045,
#28046,#28047,#28048,#28049,#28050,#28051,#28052,#28053,#28054,#28055,#28056,
#28057,#28058,#28059,#28060,#28061,#28062,#28063,#28064,#28065,#28066,#28067,
#28068,#28069,#28070,#28071,#28072,#28073,#28074,#28075,#28076,#28077,#28078,
#28079,#28080,#28081,#28082,#28083,#28084,#28085,#28086,#28087,#28088,#28089,
#28090,#28091,#28092,#28093,#28094,#28095,#28096,#28097,#28098,#28099,#28100,
#28101,#28102,#28103,#28104,#28105,#28106,#28107,#28108,#28109,#28110,#28111,
#28112,#28113,#28114,#28115,#28116,#28117,#28118,#28119,#28120,#28121,#28122,
#28123,#28124,#28125,#28126,#28127,#28128,#28129,#28130,#28131,#28132,#28133,
#28134,#28135,#28136,#28137,#28138,#28139,#28140,#28141,#28142,#28143,#28144,
#28145,#28146,#28147,#28148,#28149,#28150,#28151,#28152,#28153,#28154,#28155,
#28156,#28157,#28158,#28159,#28160,#28161,#28162,#28163,#28164,#28165,#28166),
(#28167,#28168,#28169,#28170,#28171,#28172,#28173,#28174,#28175,#28176,
#28177,#28178,#28179,#28180,#28181,#28182,#28183,#28184,#28185,#28186,#28187,
#28188,#28189,#28190,#28191,#28192,#28193,#28194,#28195,#28196,#28197,#28198,
#28199,#28200,#28201,#28202,#28203,#28204,#28205,#28206,#28207,#28208,#28209,
#28210,#28211,#28212,#28213,#28214,#28215,#28216,#28217,#28218,#28219,#28220,
#28221,#28222,#28223,#28224,#28225,#28226,#28227,#28228,#28229,#28230,#28231,
#28232,#28233,#28234,#28235,#28236,#28237,#28238,#28239,#28240,#28241,#28242,
#28243,#28244,#28245,#28246,#28247,#28248,#28249,#28250,#28251,#28252,#28253,
#28254,#28255,#28256,#28257,#28258,#28259,#28260,#28261,#28262,#28263,#28264,
#28265,#28266,#28267,#28268,#28269,#28270,#28271,#28272,#28273,#28274,#28275,
#28276,#28277,#28278,#28279,#28280,#28281,#28282,#28283,#28284,#28285,#28286,
#28287,#28288,#28289,#28290,#28291,#28292,#28293,#28294,#28295,#28296,#28297,
#28298,#28299,#28300,#28301,#28302,#28303,#28304,#28305,#28306,#28307,#28308,
#28309,#28310,#28311,#28312,#28313,#28314,#28315,#28316,#28317,#28318,#28319,
#28320,#28321,#28322,#28323,#28324,#28325,#28326,#28327),(#28328,#28329,
#28330,#28331,#28332,#28333,#28334,#28335,#28336,#28337,#28338,#28339,#28340,
#28341,#28342,#28343,#28344,#28345,#28346,#28347,#28348,#28349,#28350,#28351,
#28352,#28353,#28354,#28355,#28356,#28357,#28358,#28359,#28360,#28361,#28362,
#28363,#28364,#28365,#28366,#28367,#28368,#28369,#28370,#28371,#28372,#28373,
#28374,#28375,#28376,#28377,#28378,#28379,#28380,#28381,#28382,#28383,#28384,
#28385,#28386,#28387,#28388,#28389,#28390,#28391,#28392,#28393,#28394,#28395,
#28396,#28397,#28398,#28399,#28400,#28401,#28402,#28403,#28404,#28405,#28406,
#28407,#28408,#28409,#28410,#28411,#28412,#28413,#28414,#28415,#28416,#28417,
#28418,#28419,#28420,#28421,#28422,#28423,#28424,#28425,#28426,#28427,#28428,
#28429,#28430,#28431,#28432,#28433,#28434,#28435,#28436,#28437,#28438,#28439,
#28440,#28441,#28442,#28443,#28444,#28445,#28446,#28447,#28448,#28449,#28450,
#28451,#28452,#28453,#28454,#28455,#28456,#28457,#28458,#28459,#28460,#28461,
#28462,#28463,#28464,#28465,#28466,#28467,#28468,#28469,#28470,#28471,#28472,
#28473,#28474,#28475,#28476,#28477,#28478,#28479,#28480,#28481,#28482,#28483,
#28484,#28485,#28486,#28487,#28488),(#28489,#28490,#28491,#28492,#28493,
#28494,#28495,#28496,#28497,#28498,#28499,#28500,#28501,#28502,#28503,#28504,
#28505,#28506,#28507,#28508,#28509,#28510,#28511,#28512,#28513,#28514,#28515,
#28516,#28517,#28518,#28519,#28520,#28521,#28522,#28523,#28524,#28525,#28526,
#28527,#28528,#28529,#28530,#28531,#28532,#28533,#28534,#28535,#28536,#28537,
#28538,#28539,#28540,#28541,#28542,#28543,#28544,#28545,#28546,#28547,#28548,
#28549,#28550,#28551,#28552,#28553,#28554,#28555,#28556,#28557,#28558,#28559,
#28560,#28561,#28562,#28563,#28564,#28565,#28566,#28567,#28568,#28569,#28570,
#28571,#28572,#28573,#28574,#28575,#28576,#28577,#28578,#28579,#28580,#28581,
#28582,#28583,#28584,#28585,#28586,#28587,#28588,#28589,#28590,#28591,#28592,
#28593,#28594,#28595,#28596,#28597,#28598,#28599,#28600,#28601,#28602,#28603,
#28604,#28605,#28606,#28607,#28608,#28609,#28610,#28611,#28612,#28613,#28614,
#28615,#28616,#28617,#28618,#28619,#28620,#28621,#28622,#28623,#28624,#28625,
#28626,#28627,#28628,#28629,#28630,#28631,#28632,#28633,#28634,#28635,#28636,
#28637,#28638,#28639,#28640,#28641,#28642,#28643,#28644,#28645,#28646,#28647,
#28648,#28649)),.UNSPECIFIED.,.F.,.F.,.F.)
B_SPLINE_SURFACE_WITH_KNOTS((4,4),(3,2,2,2,2,2,2,2,2,2,2,2,2,2,2,2,2,2,
2,2,2,2,2,2,2,2,2,2,2,2,2,2,2,2,2,2,2,2,2,2,2,2,2,2,2,2,2,2,2,2,2,2,2,2,
2,2,2,2,2,2,2,2,2,2,2,2,2,2,2,2,2,2,2,2,2,2,2,2,2,2,3),(0.,1.),(0.,0.0125,
0.025,0.0375,0.05,0.0625,0.075,0.0875,0.1,0.1125,0.125,0.1375,0.15,0.1625,
0.175,0.1875,0.2,0.2125,0.225,0.2375,0.25,0.2625,0.275,0.2875,0.3,0.3125,
0.325,0.3375,0.35,0.3625,0.375,0.3875,0.4,0.4125,0.425,0.4375,0.45,0.4625,
0.475,0.4875,0.5,0.5125,0.525,0.5375,0.55,0.5625,0.575,0.5875,0.6,0.6125,
0.625,0.6375,0.65,0.6625,0.675,0.6875,0.7,0.7125,0.725,0.7375,0.75,0.7625,
0.775,0.7875,0.8,0.8125,0.825,0.8375,0.85,0.8625,0.875,0.8875,0.9,0.9125,
0.925,0.9375,0.95,0.9625,0.975,0.9875,1.),.UNSPECIFIED.)
GEOMETRIC_REPRESENTATION_ITEM()
RATIONAL_B_SPLINE_SURFACE(((1.,0.923879532511287,1.,0.923879532511287,1.,
0.923879532511287,1.,0.923879532511287,1.,0.923879532511287,1.,0.923879532511287,
1.,0.923879532511287,1.,0.923879532511287,1.,0.923879532511287,1.,0.923879532511287,
1.,0.923879532511287,1.,0.923879532511287,1.,0.923879532511287,1.,0.923879532511287,
1.,0.923879532511287,1.,0.923879532511287,1.,0.923879532511287,1.,0.923879532511287,
1.,0.923879532511287,1.,0.923879532511287,1.,0.923879532511287,1.,0.923879532511287,
1.,0.923879532511287,1.,0.923879532511287,1.,0.923879532511287,1.,0.923879532511287,
1.,0.923879532511287,1.,0.923879532511287,1.,0.923879532511287,1.,0.923879532511287,
1.,0.923879532511287,1.,0.923879532511287,1.,0.923879532511287,1.,0.923879532511287,
1.,0.923879532511287,1.,0.923879532511287,1.,0.923879532511287,1.,0.923879532511287,
1.,0.923879532511287,1.,0.923879532511287,1.,0.923879532511287,1.,0.923879532511287,
1.,0.923879532511287,1.,0.923879532511287,1.,0.923879532511287,1.,0.923879532511287,
1.,0.923879532511287,1.,0.923879532511287,1.,0.923879532511287,1.,0.923879532511287,
1.,0.923879532511287,1.,0.923879532511287,1.,0.923879532511287,1.,0.923879532511287,
1.,0.923879532511287,1.,0.923879532511287,1.,0.923879532511287,1.,0.923879532511287,
1.,0.923879532511287,1.,0.923879532511287,1.,0.923879532511287,1.,0.923879532511287,
1.,0.923879532511287,1.,0.923879532511287,1.,0.923879532511287,1.,0.923879532511287,
1.,0.923879532511287,1.,0.923879532511287,1.,0.923879532511287,1.,0.923879532511287,
1.,0.923879532511287,1.,0.923879532511287,1.,0.923879532511287,1.,0.923879532511287,
1.,0.923879532511287,1.,0.923879532511287,1.,0.923879532511287,1.,0.923879532511287,
1.,0.923879532511287,1.,0.923879532511287,1.),(0.998696642611305,0.922675387296324,
0.998696642611305,0.922675387296324,0.998696642611305,0.922675387296324,
0.998696642611305,0.922675387296324,0.998696642611305,0.922675387296324,
0.998696642611305,0.922675387296324,0.998696642611305,0.922675387296324,
0.998696642611305,0.922675387296324,0.998696642611305,0.922675387296324,
0.998696642611305,0.922675387296324,0.998696642611305,0.922675387296324,
0.998696642611305,0.922675387296324,0.998696642611305,0.922675387296324,
0.998696642611305,0.922675387296324,0.998696642611305,0.922675387296324,
0.998696642611305,0.922675387296324,0.998696642611305,0.922675387296324,
0.998696642611305,0.922675387296324,0.998696642611305,0.922675387296324,
0.998696642611305,0.922675387296324,0.998696642611305,0.922675387296324,
0.998696642611305,0.922675387296324,0.998696642611305,0.922675387296324,
0.998696642611305,0.922675387296324,0.998696642611305,0.922675387296324,
0.998696642611305,0.922675387296324,0.998696642611305,0.922675387296324,
0.998696642611305,0.922675387296324,0.998696642611305,0.922675387296324,
0.998696642611305,0.922675387296324,0.998696642611305,0.922675387296324,
0.998696642611305,0.922675387296324,0.998696642611305,0.922675387296324,
0.998696642611305,0.922675387296324,0.998696642611305,0.922675387296324,
0.998696642611305,0.922675387296324,0.998696642611305,0.922675387296324,
0.998696642611305,0.922675387296324,0.998696642611305,0.922675387296324,
0.998696642611305,0.922675387296324,0.998696642611305,0.922675387296324,
0.998696642611305,0.922675387296324,0.998696642611305,0.922675387296324,
0.998696642611305,0.922675387296324,0.998696642611305,0.922675387296324,
0.998696642611305,0.922675387296324,0.998696642611305,0.922675387296324,
0.998696642611305,0.922675387296324,0.998696642611305,0.922675387296324,
0.998696642611305,0.922675387296324,0.998696642611305,0.922675387296324,
0.998696642611305,0.922675387296324,0.998696642611305,0.922675387296324,
0.998696642611305,0.922675387296324,0.998696642611305,0.922675387296324,
0.998696642611305,0.922675387296324,0.998696642611305,0.922675387296324,
0.998696642611305,0.922675387296324,0.998696642611305,0.922675387296324,
0.998696642611305,0.922675387296324,0.998696642611305,0.922675387296324,
0.998696642611305,0.922675387296324,0.998696642611305,0.922675387296324,
0.998696642611305,0.922675387296324,0.998696642611305,0.922675387296324,
0.998696642611305,0.922675387296324,0.998696642611305,0.922675387296324,
0.998696642611305,0.922675387296324,0.998696642611305,0.922675387296324,
0.998696642611305,0.922675387296324,0.998696642611305,0.922675387296324,
0.998696642611305,0.922675387296324,0.998696642611305,0.922675387296324,
0.998696642611305,0.922675387296324,0.998696642611305,0.922675387296324,
0.998696642611305,0.922675387296324,0.998696642611305,0.922675387296324,
0.998696642611305,0.922675387296324,0.998696642611305,0.922675387296324,
0.998696642611305,0.922675387296324,0.998696642611305),(0.998696642611305,
0.922675387296324,0.998696642611305,0.922675387296324,0.998696642611305,
0.922675387296324,0.998696642611305,0.922675387296324,0.998696642611305,
0.922675387296324,0.998696642611305,0.922675387296324,0.998696642611305,
0.922675387296324,0.998696642611305,0.922675387296324,0.998696642611305,
0.922675387296324,0.998696642611305,0.922675387296324,0.998696642611305,
0.922675387296324,0.998696642611305,0.922675387296324,0.998696642611305,
0.922675387296324,0.998696642611305,0.922675387296324,0.998696642611305,
0.922675387296324,0.998696642611305,0.922675387296324,0.998696642611305,
0.922675387296324,0.998696642611305,0.922675387296324,0.998696642611305,
0.922675387296324,0.998696642611305,0.922675387296324,0.998696642611305,
0.922675387296324,0.998696642611305,0.922675387296324,0.998696642611305,
0.922675387296324,0.998696642611305,0.922675387296324,0.998696642611305,
0.922675387296324,0.998696642611305,0.922675387296324,0.998696642611305,
0.922675387296324,0.998696642611305,0.922675387296324,0.998696642611305,
0.922675387296324,0.998696642611305,0.922675387296324,0.998696642611305,
0.922675387296324,0.998696642611305,0.922675387296324,0.998696642611305,
0.922675387296324,0.998696642611305,0.922675387296324,0.998696642611305,
0.922675387296324,0.998696642611305,0.922675387296324,0.998696642611305,
0.922675387296324,0.998696642611305,0.922675387296324,0.998696642611305,
0.922675387296324,0.998696642611305,0.922675387296324,0.998696642611305,
0.922675387296324,0.998696642611305,0.922675387296324,0.998696642611305,
0.922675387296324,0.998696642611305,0.922675387296324,0.998696642611305,
0.922675387296324,0.998696642611305,0.922675387296324,0.998696642611305,
0.922675387296324,0.998696642611305,0.922675387296324,0.998696642611305,
0.922675387296324,0.998696642611305,0.922675387296324,0.998696642611305,
0.922675387296324,0.998696642611305,0.922675387296324,0.998696642611305,
0.922675387296324,0.998696642611305,0.922675387296324,0.998696642611305,
0.922675387296324,0.998696642611305,0.922675387296324,0.998696642611305,
0.922675387296324,0.998696642611305,0.922675387296324,0.998696642611305,
0.922675387296324,0.998696642611305,0.922675387296324,0.998696642611305,
0.922675387296324,0.998696642611305,0.922675387296324,0.998696642611305,
0.922675387296324,0.998696642611305,0.922675387296324,0.998696642611305,
0.922675387296324,0.998696642611305,0.922675387296324,0.998696642611305,
0.922675387296324,0.998696642611305,0.922675387296324,0.998696642611305,
0.922675387296324,0.998696642611305,0.922675387296324,0.998696642611305,
0.922675387296324,0.998696642611305,0.922675387296324,0.998696642611305,
0.922675387296324,0.998696642611305,0.922675387296324,0.998696642611305,
0.922675387296324,0.998696642611305,0.922675387296324,0.998696642611305,
0.922675387296324,0.998696642611305,0.922675387296324,0.998696642611305,
0.922675387296324,0.998696642611305,0.922675387296324,0.998696642611305),
(1.,0.923879532511287,1.,0.923879532511287,1.,0.923879532511287,1.,0.923879532511287,
1.,0.923879532511287,1.,0.923879532511287,1.,0.923879532511287,1.,0.923879532511287,
1.,0.923879532511287,1.,0.923879532511287,1.,0.923879532511287,1.,0.923879532511287,
1.,0.923879532511287,1.,0.923879532511287,1.,0.923879532511287,1.,0.923879532511287,
1.,0.923879532511287,1.,0.923879532511287,1.,0.923879532511287,1.,0.923879532511287,
1.,0.923879532511287,1.,0.923879532511287,1.,0.923879532511287,1.,0.923879532511287,
1.,0.923879532511287,1.,0.923879532511287,1.,0.923879532511287,1.,0.923879532511287,
1.,0.923879532511287,1.,0.923879532511287,1.,0.923879532511287,1.,0.923879532511287,
1.,0.923879532511287,1.,0.923879532511287,1.,0.923879532511287,1.,0.923879532511287,
1.,0.923879532511287,1.,0.923879532511287,1.,0.923879532511287,1.,0.923879532511287,
1.,0.923879532511287,1.,0.923879532511287,1.,0.923879532511287,1.,0.923879532511287,
1.,0.923879532511287,1.,0.923879532511287,1.,0.923879532511287,1.,0.923879532511287,
1.,0.923879532511287,1.,0.923879532511287,1.,0.923879532511287,1.,0.923879532511287,
1.,0.923879532511287,1.,0.923879532511287,1.,0.923879532511287,1.,0.923879532511287,
1.,0.923879532511287,1.,0.923879532511287,1.,0.923879532511287,1.,0.923879532511287,
1.,0.923879532511287,1.,0.923879532511287,1.,0.923879532511287,1.,0.923879532511287,
1.,0.923879532511287,1.,0.923879532511287,1.,0.923879532511287,1.,0.923879532511287,
1.,0.923879532511287,1.,0.923879532511287,1.,0.923879532511287,1.,0.923879532511287,
1.,0.923879532511287,1.,0.923879532511287,1.,0.923879532511287,1.,0.923879532511287,
1.,0.923879532511287,1.,0.923879532511287,1.,0.923879532511287,1.,0.923879532511287,
1.)))
REPRESENTATION_ITEM('')
SURFACE()
);
#575=(
BOUNDED_SURFACE()
B_SPLINE_SURFACE(1,2,((#28650,#28651,#28652,#28653,#28654,#28655,#28656,
#28657,#28658,#28659,#28660,#28661,#28662,#28663,#28664,#28665,#28666,#28667,
#28668,#28669,#28670,#28671,#28672,#28673,#28674,#28675,#28676,#28677,#28678,
#28679,#28680,#28681,#28682,#28683,#28684,#28685,#28686,#28687,#28688,#28689,
#28690,#28691,#28692,#28693,#28694,#28695,#28696,#28697,#28698,#28699,#28700,
#28701,#28702,#28703,#28704,#28705,#28706,#28707,#28708,#28709,#28710,#28711,
#28712,#28713,#28714,#28715,#28716,#28717,#28718,#28719,#28720,#28721,#28722,
#28723,#28724,#28725,#28726,#28727,#28728,#28729,#28730,#28731,#28732,#28733,
#28734,#28735,#28736,#28737,#28738,#28739,#28740,#28741,#28742,#28743,#28744,
#28745,#28746,#28747,#28748,#28749,#28750,#28751,#28752,#28753,#28754,#28755,
#28756,#28757,#28758,#28759,#28760,#28761,#28762,#28763,#28764,#28765,#28766,
#28767,#28768,#28769,#28770,#28771,#28772,#28773,#28774,#28775,#28776,#28777,
#28778,#28779,#28780,#28781,#28782,#28783,#28784,#28785,#28786,#28787,#28788,
#28789,#28790,#28791,#28792,#28793,#28794,#28795,#28796,#28797,#28798,#28799,
#28800,#28801,#28802,#28803,#28804,#28805,#28806,#28807,#28808,#28809,#28810),
(#28811,#28812,#28813,#28814,#28815,#28816,#28817,#28818,#28819,#28820,
#28821,#28822,#28823,#28824,#28825,#28826,#28827,#28828,#28829,#28830,#28831,
#28832,#28833,#28834,#28835,#28836,#28837,#28838,#28839,#28840,#28841,#28842,
#28843,#28844,#28845,#28846,#28847,#28848,#28849,#28850,#28851,#28852,#28853,
#28854,#28855,#28856,#28857,#28858,#28859,#28860,#28861,#28862,#28863,#28864,
#28865,#28866,#28867,#28868,#28869,#28870,#28871,#28872,#28873,#28874,#28875,
#28876,#28877,#28878,#28879,#28880,#28881,#28882,#28883,#28884,#28885,#28886,
#28887,#28888,#28889,#28890,#28891,#28892,#28893,#28894,#28895,#28896,#28897,
#28898,#28899,#28900,#28901,#28902,#28903,#28904,#28905,#28906,#28907,#28908,
#28909,#28910,#28911,#28912,#28913,#28914,#28915,#28916,#28917,#28918,#28919,
#28920,#28921,#28922,#28923,#28924,#28925,#28926,#28927,#28928,#28929,#28930,
#28931,#28932,#28933,#28934,#28935,#28936,#28937,#28938,#28939,#28940,#28941,
#28942,#28943,#28944,#28945,#28946,#28947,#28948,#28949,#28950,#28951,#28952,
#28953,#28954,#28955,#28956,#28957,#28958,#28959,#28960,#28961,#28962,#28963,
#28964,#28965,#28966,#28967,#28968,#28969,#28970,#28971)),.UNSPECIFIED.,
 .F.,.F.,.F.)
B_SPLINE_SURFACE_WITH_KNOTS((2,2),(3,2,2,2,2,2,2,2,2,2,2,2,2,2,2,2,2,2,
2,2,2,2,2,2,2,2,2,2,2,2,2,2,2,2,2,2,2,2,2,2,2,2,2,2,2,2,2,2,2,2,2,2,2,2,
2,2,2,2,2,2,2,2,2,2,2,2,2,2,2,2,2,2,2,2,2,2,2,2,2,2,3),(0.,1.),(0.,0.0125,
0.025,0.0375,0.05,0.0625,0.075,0.0875,0.1,0.1125,0.125,0.1375,0.15,0.1625,
0.175,0.1875,0.2,0.2125,0.225,0.2375,0.25,0.2625,0.275,0.2875,0.3,0.3125,
0.325,0.3375,0.35,0.3625,0.375,0.3875,0.4,0.4125,0.425,0.4375,0.45,0.4625,
0.475,0.4875,0.5,0.5125,0.525,0.5375,0.55,0.5625,0.575,0.5875,0.6,0.6125,
0.625,0.6375,0.65,0.6625,0.675,0.6875,0.7,0.7125,0.725,0.7375,0.75,0.7625,
0.775,0.7875,0.8,0.8125,0.825,0.8375,0.85,0.8625,0.875,0.8875,0.9,0.9125,
0.925,0.9375,0.95,0.9625,0.975,0.9875,1.),.UNSPECIFIED.)
GEOMETRIC_REPRESENTATION_ITEM()
RATIONAL_B_SPLINE_SURFACE(((1.,0.923879532511287,1.,0.923879532511287,1.,
0.923879532511287,1.,0.923879532511287,1.,0.923879532511287,1.,0.923879532511287,
1.,0.923879532511287,1.,0.923879532511287,1.,0.923879532511287,1.,0.923879532511287,
1.,0.923879532511287,1.,0.923879532511287,1.,0.923879532511287,1.,0.923879532511287,
1.,0.923879532511287,1.,0.923879532511287,1.,0.923879532511287,1.,0.923879532511287,
1.,0.923879532511287,1.,0.923879532511287,1.,0.923879532511287,1.,0.923879532511287,
1.,0.923879532511287,1.,0.923879532511287,1.,0.923879532511287,1.,0.923879532511287,
1.,0.923879532511287,1.,0.923879532511287,1.,0.923879532511287,1.,0.923879532511287,
1.,0.923879532511287,1.,0.923879532511287,1.,0.923879532511287,1.,0.923879532511287,
1.,0.923879532511287,1.,0.923879532511287,1.,0.923879532511287,1.,0.923879532511287,
1.,0.923879532511287,1.,0.923879532511287,1.,0.923879532511287,1.,0.923879532511287,
1.,0.923879532511287,1.,0.923879532511287,1.,0.923879532511287,1.,0.923879532511287,
1.,0.923879532511287,1.,0.923879532511287,1.,0.923879532511287,1.,0.923879532511287,
1.,0.923879532511287,1.,0.923879532511287,1.,0.923879532511287,1.,0.923879532511287,
1.,0.923879532511287,1.,0.923879532511287,1.,0.923879532511287,1.,0.923879532511287,
1.,0.923879532511287,1.,0.923879532511287,1.,0.923879532511287,1.,0.923879532511287,
1.,0.923879532511287,1.,0.923879532511287,1.,0.923879532511287,1.,0.923879532511287,
1.,0.923879532511287,1.,0.923879532511287,1.,0.923879532511287,1.,0.923879532511287,
1.,0.923879532511287,1.,0.923879532511287,1.,0.923879532511287,1.,0.923879532511287,
1.,0.923879532511287,1.,0.923879532511287,1.,0.923879532511287,1.,0.923879532511287,
1.,0.923879532511287,1.,0.923879532511287,1.),(1.,0.923879532511287,1.,
0.923879532511287,1.,0.923879532511287,1.,0.923879532511287,1.,0.923879532511287,
1.,0.923879532511287,1.,0.923879532511287,1.,0.923879532511287,1.,0.923879532511287,
1.,0.923879532511287,1.,0.923879532511287,1.,0.923879532511287,1.,0.923879532511287,
1.,0.923879532511287,1.,0.923879532511287,1.,0.923879532511287,1.,0.923879532511287,
1.,0.923879532511287,1.,0.923879532511287,1.,0.923879532511287,1.,0.923879532511287,
1.,0.923879532511287,1.,0.923879532511287,1.,0.923879532511287,1.,0.923879532511287,
1.,0.923879532511287,1.,0.923879532511287,1.,0.923879532511287,1.,0.923879532511287,
1.,0.923879532511287,1.,0.923879532511287,1.,0.923879532511287,1.,0.923879532511287,
1.,0.923879532511287,1.,0.923879532511287,1.,0.923879532511287,1.,0.923879532511287,
1.,0.923879532511287,1.,0.923879532511287,1.,0.923879532511287,1.,0.923879532511287,
1.,0.923879532511287,1.,0.923879532511287,1.,0.923879532511287,1.,0.923879532511287,
1.,0.923879532511287,1.,0.923879532511287,1.,0.923879532511287,1.,0.923879532511287,
1.,0.923879532511287,1.,0.923879532511287,1.,0.923879532511287,1.,0.923879532511287,
1.,0.923879532511287,1.,0.923879532511287,1.,0.923879532511287,1.,0.923879532511287,
1.,0.923879532511287,1.,0.923879532511287,1.,0.923879532511287,1.,0.923879532511287,
1.,0.923879532511287,1.,0.923879532511287,1.,0.923879532511287,1.,0.923879532511287,
1.,0.923879532511287,1.,0.923879532511287,1.,0.923879532511287,1.,0.923879532511287,
1.,0.923879532511287,1.,0.923879532511287,1.,0.923879532511287,1.,0.923879532511287,
1.,0.923879532511287,1.,0.923879532511287,1.,0.923879532511287,1.,0.923879532511287,
1.,0.923879532511287,1.,0.923879532511287,1.,0.923879532511287,1.)))
REPRESENTATION_ITEM('')
SURFACE()
);
#576=(
BOUNDED_SURFACE()
B_SPLINE_SURFACE(1,2,((#28989,#28990,#28991,#28992,#28993,#28994,#28995,
#28996,#28997,#28998,#28999,#29000,#29001,#29002,#29003,#29004,#29005,#29006,
#29007,#29008,#29009,#29010,#29011,#29012,#29013,#29014,#29015,#29016,#29017,
#29018,#29019,#29020,#29021,#29022,#29023,#29024,#29025,#29026,#29027,#29028,
#29029,#29030,#29031,#29032,#29033,#29034,#29035,#29036,#29037,#29038,#29039,
#29040,#29041,#29042,#29043,#29044,#29045,#29046,#29047,#29048,#29049,#29050,
#29051,#29052,#29053,#29054,#29055,#29056,#29057,#29058,#29059,#29060,#29061,
#29062,#29063,#29064,#29065,#29066,#29067,#29068,#29069,#29070,#29071,#29072,
#29073,#29074,#29075,#29076,#29077,#29078,#29079,#29080,#29081,#29082,#29083,
#29084,#29085,#29086,#29087,#29088,#29089,#29090,#29091,#29092,#29093,#29094,
#29095,#29096,#29097,#29098,#29099,#29100,#29101,#29102,#29103,#29104,#29105,
#29106,#29107,#29108,#29109,#29110,#29111,#29112,#29113,#29114,#29115,#29116,
#29117,#29118,#29119,#29120,#29121,#29122,#29123,#29124,#29125,#29126,#29127,
#29128,#29129,#29130,#29131,#29132,#29133,#29134,#29135,#29136,#29137,#29138,
#29139,#29140,#29141,#29142,#29143,#29144,#29145,#29146,#29147,#29148,#29149),
(#29150,#29151,#29152,#29153,#29154,#29155,#29156,#29157,#29158,#29159,
#29160,#29161,#29162,#29163,#29164,#29165,#29166,#29167,#29168,#29169,#29170,
#29171,#29172,#29173,#29174,#29175,#29176,#29177,#29178,#29179,#29180,#29181,
#29182,#29183,#29184,#29185,#29186,#29187,#29188,#29189,#29190,#29191,#29192,
#29193,#29194,#29195,#29196,#29197,#29198,#29199,#29200,#29201,#29202,#29203,
#29204,#29205,#29206,#29207,#29208,#29209,#29210,#29211,#29212,#29213,#29214,
#29215,#29216,#29217,#29218,#29219,#29220,#29221,#29222,#29223,#29224,#29225,
#29226,#29227,#29228,#29229,#29230,#29231,#29232,#29233,#29234,#29235,#29236,
#29237,#29238,#29239,#29240,#29241,#29242,#29243,#29244,#29245,#29246,#29247,
#29248,#29249,#29250,#29251,#29252,#29253,#29254,#29255,#29256,#29257,#29258,
#29259,#29260,#29261,#29262,#29263,#29264,#29265,#29266,#29267,#29268,#29269,
#29270,#29271,#29272,#29273,#29274,#29275,#29276,#29277,#29278,#29279,#29280,
#29281,#29282,#29283,#29284,#29285,#29286,#29287,#29288,#29289,#29290,#29291,
#29292,#29293,#29294,#29295,#29296,#29297,#29298,#29299,#29300,#29301,#29302,
#29303,#29304,#29305,#29306,#29307,#29308,#29309,#29310)),.UNSPECIFIED.,
 .F.,.F.,.F.)
B_SPLINE_SURFACE_WITH_KNOTS((2,2),(3,2,2,2,2,2,2,2,2,2,2,2,2,2,2,2,2,2,
2,2,2,2,2,2,2,2,2,2,2,2,2,2,2,2,2,2,2,2,2,2,2,2,2,2,2,2,2,2,2,2,2,2,2,2,
2,2,2,2,2,2,2,2,2,2,2,2,2,2,2,2,2,2,2,2,2,2,2,2,2,2,3),(0.,1.),(0.,0.0125,
0.025,0.0375,0.05,0.0625,0.075,0.0875,0.1,0.1125,0.125,0.1375,0.15,0.1625,
0.175,0.1875,0.2,0.2125,0.225,0.2375,0.25,0.2625,0.275,0.2875,0.3,0.3125,
0.325,0.3375,0.35,0.3625,0.375,0.3875,0.4,0.4125,0.425,0.4375,0.45,0.4625,
0.475,0.4875,0.5,0.5125,0.525,0.5375,0.55,0.5625,0.575,0.5875,0.6,0.6125,
0.625,0.6375,0.65,0.6625,0.675,0.6875,0.7,0.7125,0.725,0.7375,0.75,0.7625,
0.775,0.7875,0.8,0.8125,0.825,0.8375,0.85,0.8625,0.875,0.8875,0.9,0.9125,
0.925,0.9375,0.95,0.9625,0.975,0.9875,1.),.UNSPECIFIED.)
GEOMETRIC_REPRESENTATION_ITEM()
RATIONAL_B_SPLINE_SURFACE(((1.,0.923879532511287,1.,0.923879532511287,1.,
0.923879532511287,1.,0.923879532511287,1.,0.923879532511287,1.,0.923879532511287,
1.,0.923879532511287,1.,0.923879532511287,1.,0.923879532511287,1.,0.923879532511287,
1.,0.923879532511287,1.,0.923879532511287,1.,0.923879532511287,1.,0.923879532511287,
1.,0.923879532511287,1.,0.923879532511287,1.,0.923879532511287,1.,0.923879532511287,
1.,0.923879532511287,1.,0.923879532511287,1.,0.923879532511287,1.,0.923879532511287,
1.,0.923879532511287,1.,0.923879532511287,1.,0.923879532511287,1.,0.923879532511287,
1.,0.923879532511287,1.,0.923879532511287,1.,0.923879532511287,1.,0.923879532511287,
1.,0.923879532511287,1.,0.923879532511287,1.,0.923879532511287,1.,0.923879532511287,
1.,0.923879532511287,1.,0.923879532511287,1.,0.923879532511287,1.,0.923879532511287,
1.,0.923879532511287,1.,0.923879532511287,1.,0.923879532511287,1.,0.923879532511287,
1.,0.923879532511287,1.,0.923879532511287,1.,0.923879532511287,1.,0.923879532511287,
1.,0.923879532511287,1.,0.923879532511287,1.,0.923879532511287,1.,0.923879532511287,
1.,0.923879532511287,1.,0.923879532511287,1.,0.923879532511287,1.,0.923879532511287,
1.,0.923879532511287,1.,0.923879532511287,1.,0.923879532511287,1.,0.923879532511287,
1.,0.923879532511287,1.,0.923879532511287,1.,0.923879532511287,1.,0.923879532511287,
1.,0.923879532511287,1.,0.923879532511287,1.,0.923879532511287,1.,0.923879532511287,
1.,0.923879532511287,1.,0.923879532511287,1.,0.923879532511287,1.,0.923879532511287,
1.,0.923879532511287,1.,0.923879532511287,1.,0.923879532511287,1.,0.923879532511287,
1.,0.923879532511287,1.,0.923879532511287,1.,0.923879532511287,1.,0.923879532511287,
1.,0.923879532511287,1.,0.923879532511287,1.),(1.,0.923879532511287,1.,
0.923879532511287,1.,0.923879532511287,1.,0.923879532511287,1.,0.923879532511287,
1.,0.923879532511287,1.,0.923879532511287,1.,0.923879532511287,1.,0.923879532511287,
1.,0.923879532511287,1.,0.923879532511287,1.,0.923879532511287,1.,0.923879532511287,
1.,0.923879532511287,1.,0.923879532511287,1.,0.923879532511287,1.,0.923879532511287,
1.,0.923879532511287,1.,0.923879532511287,1.,0.923879532511287,1.,0.923879532511287,
1.,0.923879532511287,1.,0.923879532511287,1.,0.923879532511287,1.,0.923879532511287,
1.,0.923879532511287,1.,0.923879532511287,1.,0.923879532511287,1.,0.923879532511287,
1.,0.923879532511287,1.,0.923879532511287,1.,0.923879532511287,1.,0.923879532511287,
1.,0.923879532511287,1.,0.923879532511287,1.,0.923879532511287,1.,0.923879532511287,
1.,0.923879532511287,1.,0.923879532511287,1.,0.923879532511287,1.,0.923879532511287,
1.,0.923879532511287,1.,0.923879532511287,1.,0.923879532511287,1.,0.923879532511287,
1.,0.923879532511287,1.,0.923879532511287,1.,0.923879532511287,1.,0.923879532511287,
1.,0.923879532511287,1.,0.923879532511287,1.,0.923879532511287,1.,0.923879532511287,
1.,0.923879532511287,1.,0.923879532511287,1.,0.923879532511287,1.,0.923879532511287,
1.,0.923879532511287,1.,0.923879532511287,1.,0.923879532511287,1.,0.923879532511287,
1.,0.923879532511287,1.,0.923879532511287,1.,0.923879532511287,1.,0.923879532511287,
1.,0.923879532511287,1.,0.923879532511287,1.,0.923879532511287,1.,0.923879532511287,
1.,0.923879532511287,1.,0.923879532511287,1.,0.923879532511287,1.,0.923879532511287,
1.,0.923879532511287,1.,0.923879532511287,1.,0.923879532511287,1.,0.923879532511287,
1.,0.923879532511287,1.,0.923879532511287,1.,0.923879532511287,1.)))
REPRESENTATION_ITEM('')
SURFACE()
);
#577=(
BOUNDED_SURFACE()
B_SPLINE_SURFACE(3,2,((#29328,#29329,#29330,#29331,#29332,#29333,#29334,
#29335,#29336,#29337,#29338,#29339,#29340,#29341,#29342,#29343,#29344,#29345,
#29346,#29347,#29348,#29349,#29350,#29351,#29352,#29353,#29354,#29355,#29356,
#29357,#29358,#29359,#29360,#29361,#29362,#29363,#29364,#29365,#29366,#29367,
#29368,#29369,#29370,#29371,#29372,#29373,#29374,#29375,#29376,#29377,#29378,
#29379,#29380,#29381,#29382,#29383,#29384,#29385,#29386,#29387,#29388,#29389,
#29390,#29391,#29392,#29393,#29394,#29395,#29396,#29397,#29398,#29399,#29400,
#29401,#29402,#29403,#29404,#29405,#29406,#29407,#29408,#29409,#29410,#29411,
#29412,#29413,#29414,#29415,#29416,#29417,#29418,#29419,#29420,#29421,#29422,
#29423,#29424,#29425,#29426,#29427,#29428,#29429,#29430,#29431,#29432,#29433,
#29434,#29435,#29436,#29437,#29438,#29439,#29440,#29441,#29442,#29443,#29444,
#29445,#29446,#29447,#29448,#29449,#29450,#29451,#29452,#29453,#29454,#29455,
#29456,#29457,#29458,#29459,#29460,#29461,#29462,#29463,#29464,#29465,#29466,
#29467,#29468,#29469,#29470,#29471,#29472,#29473,#29474,#29475,#29476,#29477,
#29478,#29479,#29480,#29481,#29482,#29483,#29484,#29485,#29486,#29487,#29488),
(#29489,#29490,#29491,#29492,#29493,#29494,#29495,#29496,#29497,#29498,
#29499,#29500,#29501,#29502,#29503,#29504,#29505,#29506,#29507,#29508,#29509,
#29510,#29511,#29512,#29513,#29514,#29515,#29516,#29517,#29518,#29519,#29520,
#29521,#29522,#29523,#29524,#29525,#29526,#29527,#29528,#29529,#29530,#29531,
#29532,#29533,#29534,#29535,#29536,#29537,#29538,#29539,#29540,#29541,#29542,
#29543,#29544,#29545,#29546,#29547,#29548,#29549,#29550,#29551,#29552,#29553,
#29554,#29555,#29556,#29557,#29558,#29559,#29560,#29561,#29562,#29563,#29564,
#29565,#29566,#29567,#29568,#29569,#29570,#29571,#29572,#29573,#29574,#29575,
#29576,#29577,#29578,#29579,#29580,#29581,#29582,#29583,#29584,#29585,#29586,
#29587,#29588,#29589,#29590,#29591,#29592,#29593,#29594,#29595,#29596,#29597,
#29598,#29599,#29600,#29601,#29602,#29603,#29604,#29605,#29606,#29607,#29608,
#29609,#29610,#29611,#29612,#29613,#29614,#29615,#29616,#29617,#29618,#29619,
#29620,#29621,#29622,#29623,#29624,#29625,#29626,#29627,#29628,#29629,#29630,
#29631,#29632,#29633,#29634,#29635,#29636,#29637,#29638,#29639,#29640,#29641,
#29642,#29643,#29644,#29645,#29646,#29647,#29648,#29649),(#29650,#29651,
#29652,#29653,#29654,#29655,#29656,#29657,#29658,#29659,#29660,#29661,#29662,
#29663,#29664,#29665,#29666,#29667,#29668,#29669,#29670,#29671,#29672,#29673,
#29674,#29675,#29676,#29677,#29678,#29679,#29680,#29681,#29682,#29683,#29684,
#29685,#29686,#29687,#29688,#29689,#29690,#29691,#29692,#29693,#29694,#29695,
#29696,#29697,#29698,#29699,#29700,#29701,#29702,#29703,#29704,#29705,#29706,
#29707,#29708,#29709,#29710,#29711,#29712,#29713,#29714,#29715,#29716,#29717,
#29718,#29719,#29720,#29721,#29722,#29723,#29724,#29725,#29726,#29727,#29728,
#29729,#29730,#29731,#29732,#29733,#29734,#29735,#29736,#29737,#29738,#29739,
#29740,#29741,#29742,#29743,#29744,#29745,#29746,#29747,#29748,#29749,#29750,
#29751,#29752,#29753,#29754,#29755,#29756,#29757,#29758,#29759,#29760,#29761,
#29762,#29763,#29764,#29765,#29766,#29767,#29768,#29769,#29770,#29771,#29772,
#29773,#29774,#29775,#29776,#29777,#29778,#29779,#29780,#29781,#29782,#29783,
#29784,#29785,#29786,#29787,#29788,#29789,#29790,#29791,#29792,#29793,#29794,
#29795,#29796,#29797,#29798,#29799,#29800,#29801,#29802,#29803,#29804,#29805,
#29806,#29807,#29808,#29809,#29810),(#29811,#29812,#29813,#29814,#29815,
#29816,#29817,#29818,#29819,#29820,#29821,#29822,#29823,#29824,#29825,#29826,
#29827,#29828,#29829,#29830,#29831,#29832,#29833,#29834,#29835,#29836,#29837,
#29838,#29839,#29840,#29841,#29842,#29843,#29844,#29845,#29846,#29847,#29848,
#29849,#29850,#29851,#29852,#29853,#29854,#29855,#29856,#29857,#29858,#29859,
#29860,#29861,#29862,#29863,#29864,#29865,#29866,#29867,#29868,#29869,#29870,
#29871,#29872,#29873,#29874,#29875,#29876,#29877,#29878,#29879,#29880,#29881,
#29882,#29883,#29884,#29885,#29886,#29887,#29888,#29889,#29890,#29891,#29892,
#29893,#29894,#29895,#29896,#29897,#29898,#29899,#29900,#29901,#29902,#29903,
#29904,#29905,#29906,#29907,#29908,#29909,#29910,#29911,#29912,#29913,#29914,
#29915,#29916,#29917,#29918,#29919,#29920,#29921,#29922,#29923,#29924,#29925,
#29926,#29927,#29928,#29929,#29930,#29931,#29932,#29933,#29934,#29935,#29936,
#29937,#29938,#29939,#29940,#29941,#29942,#29943,#29944,#29945,#29946,#29947,
#29948,#29949,#29950,#29951,#29952,#29953,#29954,#29955,#29956,#29957,#29958,
#29959,#29960,#29961,#29962,#29963,#29964,#29965,#29966,#29967,#29968,#29969,
#29970,#29971)),.UNSPECIFIED.,.F.,.F.,.F.)
B_SPLINE_SURFACE_WITH_KNOTS((4,4),(3,2,2,2,2,2,2,2,2,2,2,2,2,2,2,2,2,2,
2,2,2,2,2,2,2,2,2,2,2,2,2,2,2,2,2,2,2,2,2,2,2,2,2,2,2,2,2,2,2,2,2,2,2,2,
2,2,2,2,2,2,2,2,2,2,2,2,2,2,2,2,2,2,2,2,2,2,2,2,2,2,3),(0.,1.),(0.,0.0125,
0.025,0.0375,0.05,0.0625,0.075,0.0875,0.1,0.1125,0.125,0.1375,0.15,0.1625,
0.175,0.1875,0.2,0.2125,0.225,0.2375,0.25,0.2625,0.275,0.2875,0.3,0.3125,
0.325,0.3375,0.35,0.3625,0.375,0.3875,0.4,0.4125,0.425,0.4375,0.45,0.4625,
0.475,0.4875,0.5,0.5125,0.525,0.5375,0.55,0.5625,0.575,0.5875,0.6,0.6125,
0.625,0.6375,0.65,0.6625,0.675,0.6875,0.7,0.7125,0.725,0.7375,0.75,0.7625,
0.775,0.7875,0.8,0.8125,0.825,0.8375,0.85,0.8625,0.875,0.8875,0.9,0.9125,
0.925,0.9375,0.95,0.9625,0.975,0.9875,1.),.UNSPECIFIED.)
GEOMETRIC_REPRESENTATION_ITEM()
RATIONAL_B_SPLINE_SURFACE(((1.,0.923879532511287,1.,0.923879532511287,1.,
0.923879532511287,1.,0.923879532511287,1.,0.923879532511287,1.,0.923879532511287,
1.,0.923879532511287,1.,0.923879532511287,1.,0.923879532511287,1.,0.923879532511287,
1.,0.923879532511287,1.,0.923879532511287,1.,0.923879532511287,1.,0.923879532511287,
1.,0.923879532511287,1.,0.923879532511287,1.,0.923879532511287,1.,0.923879532511287,
1.,0.923879532511287,1.,0.923879532511287,1.,0.923879532511287,1.,0.923879532511287,
1.,0.923879532511287,1.,0.923879532511287,1.,0.923879532511287,1.,0.923879532511287,
1.,0.923879532511287,1.,0.923879532511287,1.,0.923879532511287,1.,0.923879532511287,
1.,0.923879532511287,1.,0.923879532511287,1.,0.923879532511287,1.,0.923879532511287,
1.,0.923879532511287,1.,0.923879532511287,1.,0.923879532511287,1.,0.923879532511287,
1.,0.923879532511287,1.,0.923879532511287,1.,0.923879532511287,1.,0.923879532511287,
1.,0.923879532511287,1.,0.923879532511287,1.,0.923879532511287,1.,0.923879532511287,
1.,0.923879532511287,1.,0.923879532511287,1.,0.923879532511287,1.,0.923879532511287,
1.,0.923879532511287,1.,0.923879532511287,1.,0.923879532511287,1.,0.923879532511287,
1.,0.923879532511287,1.,0.923879532511287,1.,0.923879532511287,1.,0.923879532511287,
1.,0.923879532511287,1.,0.923879532511287,1.,0.923879532511287,1.,0.923879532511287,
1.,0.923879532511287,1.,0.923879532511287,1.,0.923879532511287,1.,0.923879532511287,
1.,0.923879532511287,1.,0.923879532511287,1.,0.923879532511287,1.,0.923879532511287,
1.,0.923879532511287,1.,0.923879532511287,1.,0.923879532511287,1.,0.923879532511287,
1.,0.923879532511287,1.,0.923879532511287,1.,0.923879532511287,1.,0.923879532511287,
1.,0.923879532511287,1.,0.923879532511287,1.),(0.998696642611305,0.922675387296324,
0.998696642611305,0.922675387296324,0.998696642611305,0.922675387296324,
0.998696642611305,0.922675387296324,0.998696642611305,0.922675387296324,
0.998696642611305,0.922675387296324,0.998696642611305,0.922675387296324,
0.998696642611305,0.922675387296324,0.998696642611305,0.922675387296324,
0.998696642611305,0.922675387296324,0.998696642611305,0.922675387296324,
0.998696642611305,0.922675387296324,0.998696642611305,0.922675387296324,
0.998696642611305,0.922675387296324,0.998696642611305,0.922675387296324,
0.998696642611305,0.922675387296324,0.998696642611305,0.922675387296324,
0.998696642611305,0.922675387296324,0.998696642611305,0.922675387296324,
0.998696642611305,0.922675387296324,0.998696642611305,0.922675387296324,
0.998696642611305,0.922675387296324,0.998696642611305,0.922675387296324,
0.998696642611305,0.922675387296324,0.998696642611305,0.922675387296324,
0.998696642611305,0.922675387296324,0.998696642611305,0.922675387296324,
0.998696642611305,0.922675387296324,0.998696642611305,0.922675387296324,
0.998696642611305,0.922675387296324,0.998696642611305,0.922675387296324,
0.998696642611305,0.922675387296324,0.998696642611305,0.922675387296324,
0.998696642611305,0.922675387296324,0.998696642611305,0.922675387296324,
0.998696642611305,0.922675387296324,0.998696642611305,0.922675387296324,
0.998696642611305,0.922675387296324,0.998696642611305,0.922675387296324,
0.998696642611305,0.922675387296324,0.998696642611305,0.922675387296324,
0.998696642611305,0.922675387296324,0.998696642611305,0.922675387296324,
0.998696642611305,0.922675387296324,0.998696642611305,0.922675387296324,
0.998696642611305,0.922675387296324,0.998696642611305,0.922675387296324,
0.998696642611305,0.922675387296324,0.998696642611305,0.922675387296324,
0.998696642611305,0.922675387296324,0.998696642611305,0.922675387296324,
0.998696642611305,0.922675387296324,0.998696642611305,0.922675387296324,
0.998696642611305,0.922675387296324,0.998696642611305,0.922675387296324,
0.998696642611305,0.922675387296324,0.998696642611305,0.922675387296324,
0.998696642611305,0.922675387296324,0.998696642611305,0.922675387296324,
0.998696642611305,0.922675387296324,0.998696642611305,0.922675387296324,
0.998696642611305,0.922675387296324,0.998696642611305,0.922675387296324,
0.998696642611305,0.922675387296324,0.998696642611305,0.922675387296324,
0.998696642611305,0.922675387296324,0.998696642611305,0.922675387296324,
0.998696642611305,0.922675387296324,0.998696642611305,0.922675387296324,
0.998696642611305,0.922675387296324,0.998696642611305,0.922675387296324,
0.998696642611305,0.922675387296324,0.998696642611305,0.922675387296324,
0.998696642611305,0.922675387296324,0.998696642611305,0.922675387296324,
0.998696642611305,0.922675387296324,0.998696642611305,0.922675387296324,
0.998696642611305,0.922675387296324,0.998696642611305,0.922675387296324,
0.998696642611305,0.922675387296324,0.998696642611305),(0.998696642611305,
0.922675387296324,0.998696642611305,0.922675387296324,0.998696642611305,
0.922675387296324,0.998696642611305,0.922675387296324,0.998696642611305,
0.922675387296324,0.998696642611305,0.922675387296324,0.998696642611305,
0.922675387296324,0.998696642611305,0.922675387296324,0.998696642611305,
0.922675387296324,0.998696642611305,0.922675387296324,0.998696642611305,
0.922675387296324,0.998696642611305,0.922675387296324,0.998696642611305,
0.922675387296324,0.998696642611305,0.922675387296324,0.998696642611305,
0.922675387296324,0.998696642611305,0.922675387296324,0.998696642611305,
0.922675387296324,0.998696642611305,0.922675387296324,0.998696642611305,
0.922675387296324,0.998696642611305,0.922675387296324,0.998696642611305,
0.922675387296324,0.998696642611305,0.922675387296324,0.998696642611305,
0.922675387296324,0.998696642611305,0.922675387296324,0.998696642611305,
0.922675387296324,0.998696642611305,0.922675387296324,0.998696642611305,
0.922675387296324,0.998696642611305,0.922675387296324,0.998696642611305,
0.922675387296324,0.998696642611305,0.922675387296324,0.998696642611305,
0.922675387296324,0.998696642611305,0.922675387296324,0.998696642611305,
0.922675387296324,0.998696642611305,0.922675387296324,0.998696642611305,
0.922675387296324,0.998696642611305,0.922675387296324,0.998696642611305,
0.922675387296324,0.998696642611305,0.922675387296324,0.998696642611305,
0.922675387296324,0.998696642611305,0.922675387296324,0.998696642611305,
0.922675387296324,0.998696642611305,0.922675387296324,0.998696642611305,
0.922675387296324,0.998696642611305,0.922675387296324,0.998696642611305,
0.922675387296324,0.998696642611305,0.922675387296324,0.998696642611305,
0.922675387296324,0.998696642611305,0.922675387296324,0.998696642611305,
0.922675387296324,0.998696642611305,0.922675387296324,0.998696642611305,
0.922675387296324,0.998696642611305,0.922675387296324,0.998696642611305,
0.922675387296324,0.998696642611305,0.922675387296324,0.998696642611305,
0.922675387296324,0.998696642611305,0.922675387296324,0.998696642611305,
0.922675387296324,0.998696642611305,0.922675387296324,0.998696642611305,
0.922675387296324,0.998696642611305,0.922675387296324,0.998696642611305,
0.922675387296324,0.998696642611305,0.922675387296324,0.998696642611305,
0.922675387296324,0.998696642611305,0.922675387296324,0.998696642611305,
0.922675387296324,0.998696642611305,0.922675387296324,0.998696642611305,
0.922675387296324,0.998696642611305,0.922675387296324,0.998696642611305,
0.922675387296324,0.998696642611305,0.922675387296324,0.998696642611305,
0.922675387296324,0.998696642611305,0.922675387296324,0.998696642611305,
0.922675387296324,0.998696642611305,0.922675387296324,0.998696642611305,
0.922675387296324,0.998696642611305,0.922675387296324,0.998696642611305,
0.922675387296324,0.998696642611305,0.922675387296324,0.998696642611305,
0.922675387296324,0.998696642611305,0.922675387296324,0.998696642611305),
(1.,0.923879532511287,1.,0.923879532511287,1.,0.923879532511287,1.,0.923879532511287,
1.,0.923879532511287,1.,0.923879532511287,1.,0.923879532511287,1.,0.923879532511287,
1.,0.923879532511287,1.,0.923879532511287,1.,0.923879532511287,1.,0.923879532511287,
1.,0.923879532511287,1.,0.923879532511287,1.,0.923879532511287,1.,0.923879532511287,
1.,0.923879532511287,1.,0.923879532511287,1.,0.923879532511287,1.,0.923879532511287,
1.,0.923879532511287,1.,0.923879532511287,1.,0.923879532511287,1.,0.923879532511287,
1.,0.923879532511287,1.,0.923879532511287,1.,0.923879532511287,1.,0.923879532511287,
1.,0.923879532511287,1.,0.923879532511287,1.,0.923879532511287,1.,0.923879532511287,
1.,0.923879532511287,1.,0.923879532511287,1.,0.923879532511287,1.,0.923879532511287,
1.,0.923879532511287,1.,0.923879532511287,1.,0.923879532511287,1.,0.923879532511287,
1.,0.923879532511287,1.,0.923879532511287,1.,0.923879532511287,1.,0.923879532511287,
1.,0.923879532511287,1.,0.923879532511287,1.,0.923879532511287,1.,0.923879532511287,
1.,0.923879532511287,1.,0.923879532511287,1.,0.923879532511287,1.,0.923879532511287,
1.,0.923879532511287,1.,0.923879532511287,1.,0.923879532511287,1.,0.923879532511287,
1.,0.923879532511287,1.,0.923879532511287,1.,0.923879532511287,1.,0.923879532511287,
1.,0.923879532511287,1.,0.923879532511287,1.,0.923879532511287,1.,0.923879532511287,
1.,0.923879532511287,1.,0.923879532511287,1.,0.923879532511287,1.,0.923879532511287,
1.,0.923879532511287,1.,0.923879532511287,1.,0.923879532511287,1.,0.923879532511287,
1.,0.923879532511287,1.,0.923879532511287,1.,0.923879532511287,1.,0.923879532511287,
1.,0.923879532511287,1.,0.923879532511287,1.,0.923879532511287,1.,0.923879532511287,
1.)))
REPRESENTATION_ITEM('')
SURFACE()
);
#578=(
BOUNDED_SURFACE()
B_SPLINE_SURFACE(1,2,((#29972,#29973,#29974,#29975,#29976,#29977,#29978,
#29979,#29980,#29981,#29982,#29983,#29984,#29985,#29986,#29987,#29988,#29989,
#29990,#29991,#29992,#29993,#29994,#29995,#29996,#29997,#29998,#29999,#30000,
#30001,#30002,#30003,#30004,#30005,#30006,#30007,#30008,#30009,#30010,#30011,
#30012,#30013,#30014,#30015,#30016,#30017,#30018,#30019,#30020,#30021,#30022,
#30023,#30024,#30025,#30026,#30027,#30028,#30029,#30030,#30031,#30032,#30033,
#30034,#30035,#30036,#30037,#30038,#30039,#30040,#30041,#30042,#30043,#30044,
#30045,#30046,#30047,#30048,#30049,#30050,#30051,#30052,#30053,#30054,#30055,
#30056,#30057,#30058,#30059,#30060,#30061,#30062,#30063,#30064,#30065,#30066,
#30067,#30068,#30069,#30070,#30071,#30072,#30073,#30074,#30075,#30076,#30077,
#30078,#30079,#30080,#30081,#30082,#30083,#30084,#30085,#30086,#30087,#30088,
#30089,#30090,#30091,#30092,#30093,#30094,#30095,#30096,#30097,#30098,#30099,
#30100,#30101,#30102,#30103,#30104,#30105,#30106,#30107,#30108,#30109,#30110,
#30111,#30112,#30113,#30114,#30115,#30116,#30117,#30118,#30119,#30120,#30121,
#30122,#30123,#30124,#30125,#30126,#30127,#30128,#30129,#30130,#30131,#30132),
(#30133,#30134,#30135,#30136,#30137,#30138,#30139,#30140,#30141,#30142,
#30143,#30144,#30145,#30146,#30147,#30148,#30149,#30150,#30151,#30152,#30153,
#30154,#30155,#30156,#30157,#30158,#30159,#30160,#30161,#30162,#30163,#30164,
#30165,#30166,#30167,#30168,#30169,#30170,#30171,#30172,#30173,#30174,#30175,
#30176,#30177,#30178,#30179,#30180,#30181,#30182,#30183,#30184,#30185,#30186,
#30187,#30188,#30189,#30190,#30191,#30192,#30193,#30194,#30195,#30196,#30197,
#30198,#30199,#30200,#30201,#30202,#30203,#30204,#30205,#30206,#30207,#30208,
#30209,#30210,#30211,#30212,#30213,#30214,#30215,#30216,#30217,#30218,#30219,
#30220,#30221,#30222,#30223,#30224,#30225,#30226,#30227,#30228,#30229,#30230,
#30231,#30232,#30233,#30234,#30235,#30236,#30237,#30238,#30239,#30240,#30241,
#30242,#30243,#30244,#30245,#30246,#30247,#30248,#30249,#30250,#30251,#30252,
#30253,#30254,#30255,#30256,#30257,#30258,#30259,#30260,#30261,#30262,#30263,
#30264,#30265,#30266,#30267,#30268,#30269,#30270,#30271,#30272,#30273,#30274,
#30275,#30276,#30277,#30278,#30279,#30280,#30281,#30282,#30283,#30284,#30285,
#30286,#30287,#30288,#30289,#30290,#30291,#30292,#30293)),.UNSPECIFIED.,
 .F.,.F.,.F.)
B_SPLINE_SURFACE_WITH_KNOTS((2,2),(3,2,2,2,2,2,2,2,2,2,2,2,2,2,2,2,2,2,
2,2,2,2,2,2,2,2,2,2,2,2,2,2,2,2,2,2,2,2,2,2,2,2,2,2,2,2,2,2,2,2,2,2,2,2,
2,2,2,2,2,2,2,2,2,2,2,2,2,2,2,2,2,2,2,2,2,2,2,2,2,2,3),(0.,1.),(0.,0.0125,
0.025,0.0375,0.05,0.0625,0.075,0.0875,0.1,0.1125,0.125,0.1375,0.15,0.1625,
0.175,0.1875,0.2,0.2125,0.225,0.2375,0.25,0.2625,0.275,0.2875,0.3,0.3125,
0.325,0.3375,0.35,0.3625,0.375,0.3875,0.4,0.4125,0.425,0.4375,0.45,0.4625,
0.475,0.4875,0.5,0.5125,0.525,0.5375,0.55,0.5625,0.575,0.5875,0.6,0.6125,
0.625,0.6375,0.65,0.6625,0.675,0.6875,0.7,0.7125,0.725,0.7375,0.75,0.7625,
0.775,0.7875,0.8,0.8125,0.825,0.8375,0.85,0.8625,0.875,0.8875,0.9,0.9125,
0.925,0.9375,0.95,0.9625,0.975,0.9875,1.),.UNSPECIFIED.)
GEOMETRIC_REPRESENTATION_ITEM()
RATIONAL_B_SPLINE_SURFACE(((1.,0.923879532511287,1.,0.923879532511287,1.,
0.923879532511287,1.,0.923879532511287,1.,0.923879532511287,1.,0.923879532511287,
1.,0.923879532511287,1.,0.923879532511287,1.,0.923879532511287,1.,0.923879532511287,
1.,0.923879532511287,1.,0.923879532511287,1.,0.923879532511287,1.,0.923879532511287,
1.,0.923879532511287,1.,0.923879532511287,1.,0.923879532511287,1.,0.923879532511287,
1.,0.923879532511287,1.,0.923879532511287,1.,0.923879532511287,1.,0.923879532511287,
1.,0.923879532511287,1.,0.923879532511287,1.,0.923879532511287,1.,0.923879532511287,
1.,0.923879532511287,1.,0.923879532511287,1.,0.923879532511287,1.,0.923879532511287,
1.,0.923879532511287,1.,0.923879532511287,1.,0.923879532511287,1.,0.923879532511287,
1.,0.923879532511287,1.,0.923879532511287,1.,0.923879532511287,1.,0.923879532511287,
1.,0.923879532511287,1.,0.923879532511287,1.,0.923879532511287,1.,0.923879532511287,
1.,0.923879532511287,1.,0.923879532511287,1.,0.923879532511287,1.,0.923879532511287,
1.,0.923879532511287,1.,0.923879532511287,1.,0.923879532511287,1.,0.923879532511287,
1.,0.923879532511287,1.,0.923879532511287,1.,0.923879532511287,1.,0.923879532511287,
1.,0.923879532511287,1.,0.923879532511287,1.,0.923879532511287,1.,0.923879532511287,
1.,0.923879532511287,1.,0.923879532511287,1.,0.923879532511287,1.,0.923879532511287,
1.,0.923879532511287,1.,0.923879532511287,1.,0.923879532511287,1.,0.923879532511287,
1.,0.923879532511287,1.,0.923879532511287,1.,0.923879532511287,1.,0.923879532511287,
1.,0.923879532511287,1.,0.923879532511287,1.,0.923879532511287,1.,0.923879532511287,
1.,0.923879532511287,1.,0.923879532511287,1.,0.923879532511287,1.,0.923879532511287,
1.,0.923879532511287,1.,0.923879532511287,1.),(1.,0.923879532511287,1.,
0.923879532511287,1.,0.923879532511287,1.,0.923879532511287,1.,0.923879532511287,
1.,0.923879532511287,1.,0.923879532511287,1.,0.923879532511287,1.,0.923879532511287,
1.,0.923879532511287,1.,0.923879532511287,1.,0.923879532511287,1.,0.923879532511287,
1.,0.923879532511287,1.,0.923879532511287,1.,0.923879532511287,1.,0.923879532511287,
1.,0.923879532511287,1.,0.923879532511287,1.,0.923879532511287,1.,0.923879532511287,
1.,0.923879532511287,1.,0.923879532511287,1.,0.923879532511287,1.,0.923879532511287,
1.,0.923879532511287,1.,0.923879532511287,1.,0.923879532511287,1.,0.923879532511287,
1.,0.923879532511287,1.,0.923879532511287,1.,0.923879532511287,1.,0.923879532511287,
1.,0.923879532511287,1.,0.923879532511287,1.,0.923879532511287,1.,0.923879532511287,
1.,0.923879532511287,1.,0.923879532511287,1.,0.923879532511287,1.,0.923879532511287,
1.,0.923879532511287,1.,0.923879532511287,1.,0.923879532511287,1.,0.923879532511287,
1.,0.923879532511287,1.,0.923879532511287,1.,0.923879532511287,1.,0.923879532511287,
1.,0.923879532511287,1.,0.923879532511287,1.,0.923879532511287,1.,0.923879532511287,
1.,0.923879532511287,1.,0.923879532511287,1.,0.923879532511287,1.,0.923879532511287,
1.,0.923879532511287,1.,0.923879532511287,1.,0.923879532511287,1.,0.923879532511287,
1.,0.923879532511287,1.,0.923879532511287,1.,0.923879532511287,1.,0.923879532511287,
1.,0.923879532511287,1.,0.923879532511287,1.,0.923879532511287,1.,0.923879532511287,
1.,0.923879532511287,1.,0.923879532511287,1.,0.923879532511287,1.,0.923879532511287,
1.,0.923879532511287,1.,0.923879532511287,1.,0.923879532511287,1.,0.923879532511287,
1.,0.923879532511287,1.,0.923879532511287,1.,0.923879532511287,1.)))
REPRESENTATION_ITEM('')
SURFACE()
);
#579=(
BOUNDED_SURFACE()
B_SPLINE_SURFACE(1,2,((#30311,#30312,#30313,#30314,#30315,#30316,#30317,
#30318,#30319,#30320,#30321,#30322,#30323,#30324,#30325,#30326,#30327,#30328,
#30329,#30330,#30331,#30332,#30333,#30334,#30335,#30336,#30337,#30338,#30339,
#30340,#30341,#30342,#30343,#30344,#30345,#30346,#30347,#30348,#30349,#30350,
#30351,#30352,#30353,#30354,#30355,#30356,#30357,#30358,#30359,#30360,#30361,
#30362,#30363,#30364,#30365,#30366,#30367,#30368,#30369,#30370,#30371,#30372,
#30373,#30374,#30375,#30376,#30377,#30378,#30379,#30380,#30381,#30382,#30383,
#30384,#30385,#30386,#30387,#30388,#30389,#30390,#30391,#30392,#30393,#30394,
#30395,#30396,#30397,#30398,#30399,#30400,#30401,#30402,#30403,#30404,#30405,
#30406,#30407,#30408,#30409,#30410,#30411,#30412,#30413,#30414,#30415,#30416,
#30417,#30418,#30419,#30420,#30421,#30422,#30423,#30424,#30425,#30426,#30427,
#30428,#30429,#30430,#30431,#30432,#30433,#30434,#30435,#30436,#30437,#30438,
#30439,#30440,#30441,#30442,#30443,#30444,#30445,#30446,#30447,#30448,#30449,
#30450,#30451,#30452,#30453,#30454,#30455,#30456,#30457,#30458,#30459,#30460,
#30461,#30462,#30463,#30464,#30465,#30466,#30467,#30468,#30469,#30470,#30471),
(#30472,#30473,#30474,#30475,#30476,#30477,#30478,#30479,#30480,#30481,
#30482,#30483,#30484,#30485,#30486,#30487,#30488,#30489,#30490,#30491,#30492,
#30493,#30494,#30495,#30496,#30497,#30498,#30499,#30500,#30501,#30502,#30503,
#30504,#30505,#30506,#30507,#30508,#30509,#30510,#30511,#30512,#30513,#30514,
#30515,#30516,#30517,#30518,#30519,#30520,#30521,#30522,#30523,#30524,#30525,
#30526,#30527,#30528,#30529,#30530,#30531,#30532,#30533,#30534,#30535,#30536,
#30537,#30538,#30539,#30540,#30541,#30542,#30543,#30544,#30545,#30546,#30547,
#30548,#30549,#30550,#30551,#30552,#30553,#30554,#30555,#30556,#30557,#30558,
#30559,#30560,#30561,#30562,#30563,#30564,#30565,#30566,#30567,#30568,#30569,
#30570,#30571,#30572,#30573,#30574,#30575,#30576,#30577,#30578,#30579,#30580,
#30581,#30582,#30583,#30584,#30585,#30586,#30587,#30588,#30589,#30590,#30591,
#30592,#30593,#30594,#30595,#30596,#30597,#30598,#30599,#30600,#30601,#30602,
#30603,#30604,#30605,#30606,#30607,#30608,#30609,#30610,#30611,#30612,#30613,
#30614,#30615,#30616,#30617,#30618,#30619,#30620,#30621,#30622,#30623,#30624,
#30625,#30626,#30627,#30628,#30629,#30630,#30631,#30632)),.UNSPECIFIED.,
 .F.,.F.,.F.)
B_SPLINE_SURFACE_WITH_KNOTS((2,2),(3,2,2,2,2,2,2,2,2,2,2,2,2,2,2,2,2,2,
2,2,2,2,2,2,2,2,2,2,2,2,2,2,2,2,2,2,2,2,2,2,2,2,2,2,2,2,2,2,2,2,2,2,2,2,
2,2,2,2,2,2,2,2,2,2,2,2,2,2,2,2,2,2,2,2,2,2,2,2,2,2,3),(0.,1.),(0.,0.0125,
0.025,0.0375,0.05,0.0625,0.075,0.0875,0.1,0.1125,0.125,0.1375,0.15,0.1625,
0.175,0.1875,0.2,0.2125,0.225,0.2375,0.25,0.2625,0.275,0.2875,0.3,0.3125,
0.325,0.3375,0.35,0.3625,0.375,0.3875,0.4,0.4125,0.425,0.4375,0.45,0.4625,
0.475,0.4875,0.5,0.5125,0.525,0.5375,0.55,0.5625,0.575,0.5875,0.6,0.6125,
0.625,0.6375,0.65,0.6625,0.675,0.6875,0.7,0.7125,0.725,0.7375,0.75,0.7625,
0.775,0.7875,0.8,0.8125,0.825,0.8375,0.85,0.8625,0.875,0.8875,0.9,0.9125,
0.925,0.9375,0.95,0.9625,0.975,0.9875,1.),.UNSPECIFIED.)
GEOMETRIC_REPRESENTATION_ITEM()
RATIONAL_B_SPLINE_SURFACE(((1.,0.923879532511287,1.,0.923879532511287,1.,
0.923879532511287,1.,0.923879532511287,1.,0.923879532511287,1.,0.923879532511287,
1.,0.923879532511287,1.,0.923879532511287,1.,0.923879532511287,1.,0.923879532511287,
1.,0.923879532511287,1.,0.923879532511287,1.,0.923879532511287,1.,0.923879532511287,
1.,0.923879532511287,1.,0.923879532511287,1.,0.923879532511287,1.,0.923879532511287,
1.,0.923879532511287,1.,0.923879532511287,1.,0.923879532511287,1.,0.923879532511287,
1.,0.923879532511287,1.,0.923879532511287,1.,0.923879532511287,1.,0.923879532511287,
1.,0.923879532511287,1.,0.923879532511287,1.,0.923879532511287,1.,0.923879532511287,
1.,0.923879532511287,1.,0.923879532511287,1.,0.923879532511287,1.,0.923879532511287,
1.,0.923879532511287,1.,0.923879532511287,1.,0.923879532511287,1.,0.923879532511287,
1.,0.923879532511287,1.,0.923879532511287,1.,0.923879532511287,1.,0.923879532511287,
1.,0.923879532511287,1.,0.923879532511287,1.,0.923879532511287,1.,0.923879532511287,
1.,0.923879532511287,1.,0.923879532511287,1.,0.923879532511287,1.,0.923879532511287,
1.,0.923879532511287,1.,0.923879532511287,1.,0.923879532511287,1.,0.923879532511287,
1.,0.923879532511287,1.,0.923879532511287,1.,0.923879532511287,1.,0.923879532511287,
1.,0.923879532511287,1.,0.923879532511287,1.,0.923879532511287,1.,0.923879532511287,
1.,0.923879532511287,1.,0.923879532511287,1.,0.923879532511287,1.,0.923879532511287,
1.,0.923879532511287,1.,0.923879532511287,1.,0.923879532511287,1.,0.923879532511287,
1.,0.923879532511287,1.,0.923879532511287,1.,0.923879532511287,1.,0.923879532511287,
1.,0.923879532511287,1.,0.923879532511287,1.,0.923879532511287,1.,0.923879532511287,
1.,0.923879532511287,1.,0.923879532511287,1.),(1.,0.923879532511287,1.,
0.923879532511287,1.,0.923879532511287,1.,0.923879532511287,1.,0.923879532511287,
1.,0.923879532511287,1.,0.923879532511287,1.,0.923879532511287,1.,0.923879532511287,
1.,0.923879532511287,1.,0.923879532511287,1.,0.923879532511287,1.,0.923879532511287,
1.,0.923879532511287,1.,0.923879532511287,1.,0.923879532511287,1.,0.923879532511287,
1.,0.923879532511287,1.,0.923879532511287,1.,0.923879532511287,1.,0.923879532511287,
1.,0.923879532511287,1.,0.923879532511287,1.,0.923879532511287,1.,0.923879532511287,
1.,0.923879532511287,1.,0.923879532511287,1.,0.923879532511287,1.,0.923879532511287,
1.,0.923879532511287,1.,0.923879532511287,1.,0.923879532511287,1.,0.923879532511287,
1.,0.923879532511287,1.,0.923879532511287,1.,0.923879532511287,1.,0.923879532511287,
1.,0.923879532511287,1.,0.923879532511287,1.,0.923879532511287,1.,0.923879532511287,
1.,0.923879532511287,1.,0.923879532511287,1.,0.923879532511287,1.,0.923879532511287,
1.,0.923879532511287,1.,0.923879532511287,1.,0.923879532511287,1.,0.923879532511287,
1.,0.923879532511287,1.,0.923879532511287,1.,0.923879532511287,1.,0.923879532511287,
1.,0.923879532511287,1.,0.923879532511287,1.,0.923879532511287,1.,0.923879532511287,
1.,0.923879532511287,1.,0.923879532511287,1.,0.923879532511287,1.,0.923879532511287,
1.,0.923879532511287,1.,0.923879532511287,1.,0.923879532511287,1.,0.923879532511287,
1.,0.923879532511287,1.,0.923879532511287,1.,0.923879532511287,1.,0.923879532511287,
1.,0.923879532511287,1.,0.923879532511287,1.,0.923879532511287,1.,0.923879532511287,
1.,0.923879532511287,1.,0.923879532511287,1.,0.923879532511287,1.,0.923879532511287,
1.,0.923879532511287,1.,0.923879532511287,1.,0.923879532511287,1.)))
REPRESENTATION_ITEM('')
SURFACE()
);
#580=(
BOUNDED_SURFACE()
B_SPLINE_SURFACE(3,2,((#30650,#30651,#30652,#30653,#30654,#30655,#30656,
#30657,#30658,#30659,#30660,#30661,#30662,#30663,#30664,#30665,#30666,#30667,
#30668,#30669,#30670,#30671,#30672,#30673,#30674,#30675,#30676,#30677,#30678,
#30679,#30680,#30681,#30682,#30683,#30684,#30685,#30686,#30687,#30688,#30689,
#30690,#30691,#30692,#30693,#30694,#30695,#30696,#30697,#30698,#30699,#30700,
#30701,#30702,#30703,#30704,#30705,#30706,#30707,#30708,#30709,#30710,#30711,
#30712,#30713,#30714,#30715,#30716,#30717,#30718,#30719,#30720,#30721,#30722,
#30723,#30724,#30725,#30726,#30727,#30728,#30729,#30730,#30731,#30732,#30733,
#30734,#30735,#30736,#30737,#30738,#30739,#30740,#30741,#30742,#30743,#30744,
#30745,#30746,#30747,#30748,#30749,#30750,#30751,#30752,#30753,#30754,#30755,
#30756,#30757,#30758,#30759,#30760,#30761,#30762,#30763,#30764,#30765,#30766,
#30767,#30768,#30769,#30770,#30771,#30772,#30773,#30774,#30775,#30776,#30777,
#30778,#30779,#30780,#30781,#30782,#30783,#30784,#30785,#30786,#30787,#30788,
#30789,#30790,#30791,#30792,#30793,#30794,#30795,#30796,#30797,#30798,#30799,
#30800,#30801,#30802,#30803,#30804,#30805,#30806,#30807,#30808,#30809,#30810),
(#30811,#30812,#30813,#30814,#30815,#30816,#30817,#30818,#30819,#30820,
#30821,#30822,#30823,#30824,#30825,#30826,#30827,#30828,#30829,#30830,#30831,
#30832,#30833,#30834,#30835,#30836,#30837,#30838,#30839,#30840,#30841,#30842,
#30843,#30844,#30845,#30846,#30847,#30848,#30849,#30850,#30851,#30852,#30853,
#30854,#30855,#30856,#30857,#30858,#30859,#30860,#30861,#30862,#30863,#30864,
#30865,#30866,#30867,#30868,#30869,#30870,#30871,#30872,#30873,#30874,#30875,
#30876,#30877,#30878,#30879,#30880,#30881,#30882,#30883,#30884,#30885,#30886,
#30887,#30888,#30889,#30890,#30891,#30892,#30893,#30894,#30895,#30896,#30897,
#30898,#30899,#30900,#30901,#30902,#30903,#30904,#30905,#30906,#30907,#30908,
#30909,#30910,#30911,#30912,#30913,#30914,#30915,#30916,#30917,#30918,#30919,
#30920,#30921,#30922,#30923,#30924,#30925,#30926,#30927,#30928,#30929,#30930,
#30931,#30932,#30933,#30934,#30935,#30936,#30937,#30938,#30939,#30940,#30941,
#30942,#30943,#30944,#30945,#30946,#30947,#30948,#30949,#30950,#30951,#30952,
#30953,#30954,#30955,#30956,#30957,#30958,#30959,#30960,#30961,#30962,#30963,
#30964,#30965,#30966,#30967,#30968,#30969,#30970,#30971),(#30972,#30973,
#30974,#30975,#30976,#30977,#30978,#30979,#30980,#30981,#30982,#30983,#30984,
#30985,#30986,#30987,#30988,#30989,#30990,#30991,#30992,#30993,#30994,#30995,
#30996,#30997,#30998,#30999,#31000,#31001,#31002,#31003,#31004,#31005,#31006,
#31007,#31008,#31009,#31010,#31011,#31012,#31013,#31014,#31015,#31016,#31017,
#31018,#31019,#31020,#31021,#31022,#31023,#31024,#31025,#31026,#31027,#31028,
#31029,#31030,#31031,#31032,#31033,#31034,#31035,#31036,#31037,#31038,#31039,
#31040,#31041,#31042,#31043,#31044,#31045,#31046,#31047,#31048,#31049,#31050,
#31051,#31052,#31053,#31054,#31055,#31056,#31057,#31058,#31059,#31060,#31061,
#31062,#31063,#31064,#31065,#31066,#31067,#31068,#31069,#31070,#31071,#31072,
#31073,#31074,#31075,#31076,#31077,#31078,#31079,#31080,#31081,#31082,#31083,
#31084,#31085,#31086,#31087,#31088,#31089,#31090,#31091,#31092,#31093,#31094,
#31095,#31096,#31097,#31098,#31099,#31100,#31101,#31102,#31103,#31104,#31105,
#31106,#31107,#31108,#31109,#31110,#31111,#31112,#31113,#31114,#31115,#31116,
#31117,#31118,#31119,#31120,#31121,#31122,#31123,#31124,#31125,#31126,#31127,
#31128,#31129,#31130,#31131,#31132),(#31133,#31134,#31135,#31136,#31137,
#31138,#31139,#31140,#31141,#31142,#31143,#31144,#31145,#31146,#31147,#31148,
#31149,#31150,#31151,#31152,#31153,#31154,#31155,#31156,#31157,#31158,#31159,
#31160,#31161,#31162,#31163,#31164,#31165,#31166,#31167,#31168,#31169,#31170,
#31171,#31172,#31173,#31174,#31175,#31176,#31177,#31178,#31179,#31180,#31181,
#31182,#31183,#31184,#31185,#31186,#31187,#31188,#31189,#31190,#31191,#31192,
#31193,#31194,#31195,#31196,#31197,#31198,#31199,#31200,#31201,#31202,#31203,
#31204,#31205,#31206,#31207,#31208,#31209,#31210,#31211,#31212,#31213,#31214,
#31215,#31216,#31217,#31218,#31219,#31220,#31221,#31222,#31223,#31224,#31225,
#31226,#31227,#31228,#31229,#31230,#31231,#31232,#31233,#31234,#31235,#31236,
#31237,#31238,#31239,#31240,#31241,#31242,#31243,#31244,#31245,#31246,#31247,
#31248,#31249,#31250,#31251,#31252,#31253,#31254,#31255,#31256,#31257,#31258,
#31259,#31260,#31261,#31262,#31263,#31264,#31265,#31266,#31267,#31268,#31269,
#31270,#31271,#31272,#31273,#31274,#31275,#31276,#31277,#31278,#31279,#31280,
#31281,#31282,#31283,#31284,#31285,#31286,#31287,#31288,#31289,#31290,#31291,
#31292,#31293)),.UNSPECIFIED.,.F.,.F.,.F.)
B_SPLINE_SURFACE_WITH_KNOTS((4,4),(3,2,2,2,2,2,2,2,2,2,2,2,2,2,2,2,2,2,
2,2,2,2,2,2,2,2,2,2,2,2,2,2,2,2,2,2,2,2,2,2,2,2,2,2,2,2,2,2,2,2,2,2,2,2,
2,2,2,2,2,2,2,2,2,2,2,2,2,2,2,2,2,2,2,2,2,2,2,2,2,2,3),(0.,1.),(0.,0.0125,
0.025,0.0375,0.05,0.0625,0.075,0.0875,0.1,0.1125,0.125,0.1375,0.15,0.1625,
0.175,0.1875,0.2,0.2125,0.225,0.2375,0.25,0.2625,0.275,0.2875,0.3,0.3125,
0.325,0.3375,0.35,0.3625,0.375,0.3875,0.4,0.4125,0.425,0.4375,0.45,0.4625,
0.475,0.4875,0.5,0.5125,0.525,0.5375,0.55,0.5625,0.575,0.5875,0.6,0.6125,
0.625,0.6375,0.65,0.6625,0.675,0.6875,0.7,0.7125,0.725,0.7375,0.75,0.7625,
0.775,0.7875,0.8,0.8125,0.825,0.8375,0.85,0.8625,0.875,0.8875,0.9,0.9125,
0.925,0.9375,0.95,0.9625,0.975,0.9875,1.),.UNSPECIFIED.)
GEOMETRIC_REPRESENTATION_ITEM()
RATIONAL_B_SPLINE_SURFACE(((1.,0.923879532511287,1.,0.923879532511287,1.,
0.923879532511287,1.,0.923879532511287,1.,0.923879532511287,1.,0.923879532511287,
1.,0.923879532511287,1.,0.923879532511287,1.,0.923879532511287,1.,0.923879532511287,
1.,0.923879532511287,1.,0.923879532511287,1.,0.923879532511287,1.,0.923879532511287,
1.,0.923879532511287,1.,0.923879532511287,1.,0.923879532511287,1.,0.923879532511287,
1.,0.923879532511287,1.,0.923879532511287,1.,0.923879532511287,1.,0.923879532511287,
1.,0.923879532511287,1.,0.923879532511287,1.,0.923879532511287,1.,0.923879532511287,
1.,0.923879532511287,1.,0.923879532511287,1.,0.923879532511287,1.,0.923879532511287,
1.,0.923879532511287,1.,0.923879532511287,1.,0.923879532511287,1.,0.923879532511287,
1.,0.923879532511287,1.,0.923879532511287,1.,0.923879532511287,1.,0.923879532511287,
1.,0.923879532511287,1.,0.923879532511287,1.,0.923879532511287,1.,0.923879532511287,
1.,0.923879532511287,1.,0.923879532511287,1.,0.923879532511287,1.,0.923879532511287,
1.,0.923879532511287,1.,0.923879532511287,1.,0.923879532511287,1.,0.923879532511287,
1.,0.923879532511287,1.,0.923879532511287,1.,0.923879532511287,1.,0.923879532511287,
1.,0.923879532511287,1.,0.923879532511287,1.,0.923879532511287,1.,0.923879532511287,
1.,0.923879532511287,1.,0.923879532511287,1.,0.923879532511287,1.,0.923879532511287,
1.,0.923879532511287,1.,0.923879532511287,1.,0.923879532511287,1.,0.923879532511287,
1.,0.923879532511287,1.,0.923879532511287,1.,0.923879532511287,1.,0.923879532511287,
1.,0.923879532511287,1.,0.923879532511287,1.,0.923879532511287,1.,0.923879532511287,
1.,0.923879532511287,1.,0.923879532511287,1.,0.923879532511287,1.,0.923879532511287,
1.,0.923879532511287,1.,0.923879532511287,1.),(0.998696642611305,0.922675387296324,
0.998696642611305,0.922675387296324,0.998696642611305,0.922675387296324,
0.998696642611305,0.922675387296324,0.998696642611305,0.922675387296324,
0.998696642611305,0.922675387296324,0.998696642611305,0.922675387296324,
0.998696642611305,0.922675387296324,0.998696642611305,0.922675387296324,
0.998696642611305,0.922675387296324,0.998696642611305,0.922675387296324,
0.998696642611305,0.922675387296324,0.998696642611305,0.922675387296324,
0.998696642611305,0.922675387296324,0.998696642611305,0.922675387296324,
0.998696642611305,0.922675387296324,0.998696642611305,0.922675387296324,
0.998696642611305,0.922675387296324,0.998696642611305,0.922675387296324,
0.998696642611305,0.922675387296324,0.998696642611305,0.922675387296324,
0.998696642611305,0.922675387296324,0.998696642611305,0.922675387296324,
0.998696642611305,0.922675387296324,0.998696642611305,0.922675387296324,
0.998696642611305,0.922675387296324,0.998696642611305,0.922675387296324,
0.998696642611305,0.922675387296324,0.998696642611305,0.922675387296324,
0.998696642611305,0.922675387296324,0.998696642611305,0.922675387296324,
0.998696642611305,0.922675387296324,0.998696642611305,0.922675387296324,
0.998696642611305,0.922675387296324,0.998696642611305,0.922675387296324,
0.998696642611305,0.922675387296324,0.998696642611305,0.922675387296324,
0.998696642611305,0.922675387296324,0.998696642611305,0.922675387296324,
0.998696642611305,0.922675387296324,0.998696642611305,0.922675387296324,
0.998696642611305,0.922675387296324,0.998696642611305,0.922675387296324,
0.998696642611305,0.922675387296324,0.998696642611305,0.922675387296324,
0.998696642611305,0.922675387296324,0.998696642611305,0.922675387296324,
0.998696642611305,0.922675387296324,0.998696642611305,0.922675387296324,
0.998696642611305,0.922675387296324,0.998696642611305,0.922675387296324,
0.998696642611305,0.922675387296324,0.998696642611305,0.922675387296324,
0.998696642611305,0.922675387296324,0.998696642611305,0.922675387296324,
0.998696642611305,0.922675387296324,0.998696642611305,0.922675387296324,
0.998696642611305,0.922675387296324,0.998696642611305,0.922675387296324,
0.998696642611305,0.922675387296324,0.998696642611305,0.922675387296324,
0.998696642611305,0.922675387296324,0.998696642611305,0.922675387296324,
0.998696642611305,0.922675387296324,0.998696642611305,0.922675387296324,
0.998696642611305,0.922675387296324,0.998696642611305,0.922675387296324,
0.998696642611305,0.922675387296324,0.998696642611305,0.922675387296324,
0.998696642611305,0.922675387296324,0.998696642611305,0.922675387296324,
0.998696642611305,0.922675387296324,0.998696642611305,0.922675387296324,
0.998696642611305,0.922675387296324,0.998696642611305,0.922675387296324,
0.998696642611305,0.922675387296324,0.998696642611305,0.922675387296324,
0.998696642611305,0.922675387296324,0.998696642611305,0.922675387296324,
0.998696642611305,0.922675387296324,0.998696642611305),(0.998696642611305,
0.922675387296324,0.998696642611305,0.922675387296324,0.998696642611305,
0.922675387296324,0.998696642611305,0.922675387296324,0.998696642611305,
0.922675387296324,0.998696642611305,0.922675387296324,0.998696642611305,
0.922675387296324,0.998696642611305,0.922675387296324,0.998696642611305,
0.922675387296324,0.998696642611305,0.922675387296324,0.998696642611305,
0.922675387296324,0.998696642611305,0.922675387296324,0.998696642611305,
0.922675387296324,0.998696642611305,0.922675387296324,0.998696642611305,
0.922675387296324,0.998696642611305,0.922675387296324,0.998696642611305,
0.922675387296324,0.998696642611305,0.922675387296324,0.998696642611305,
0.922675387296324,0.998696642611305,0.922675387296324,0.998696642611305,
0.922675387296324,0.998696642611305,0.922675387296324,0.998696642611305,
0.922675387296324,0.998696642611305,0.922675387296324,0.998696642611305,
0.922675387296324,0.998696642611305,0.922675387296324,0.998696642611305,
0.922675387296324,0.998696642611305,0.922675387296324,0.998696642611305,
0.922675387296324,0.998696642611305,0.922675387296324,0.998696642611305,
0.922675387296324,0.998696642611305,0.922675387296324,0.998696642611305,
0.922675387296324,0.998696642611305,0.922675387296324,0.998696642611305,
0.922675387296324,0.998696642611305,0.922675387296324,0.998696642611305,
0.922675387296324,0.998696642611305,0.922675387296324,0.998696642611305,
0.922675387296324,0.998696642611305,0.922675387296324,0.998696642611305,
0.922675387296324,0.998696642611305,0.922675387296324,0.998696642611305,
0.922675387296324,0.998696642611305,0.922675387296324,0.998696642611305,
0.922675387296324,0.998696642611305,0.922675387296324,0.998696642611305,
0.922675387296324,0.998696642611305,0.922675387296324,0.998696642611305,
0.922675387296324,0.998696642611305,0.922675387296324,0.998696642611305,
0.922675387296324,0.998696642611305,0.922675387296324,0.998696642611305,
0.922675387296324,0.998696642611305,0.922675387296324,0.998696642611305,
0.922675387296324,0.998696642611305,0.922675387296324,0.998696642611305,
0.922675387296324,0.998696642611305,0.922675387296324,0.998696642611305,
0.922675387296324,0.998696642611305,0.922675387296324,0.998696642611305,
0.922675387296324,0.998696642611305,0.922675387296324,0.998696642611305,
0.922675387296324,0.998696642611305,0.922675387296324,0.998696642611305,
0.922675387296324,0.998696642611305,0.922675387296324,0.998696642611305,
0.922675387296324,0.998696642611305,0.922675387296324,0.998696642611305,
0.922675387296324,0.998696642611305,0.922675387296324,0.998696642611305,
0.922675387296324,0.998696642611305,0.922675387296324,0.998696642611305,
0.922675387296324,0.998696642611305,0.922675387296324,0.998696642611305,
0.922675387296324,0.998696642611305,0.922675387296324,0.998696642611305,
0.922675387296324,0.998696642611305,0.922675387296324,0.998696642611305,
0.922675387296324,0.998696642611305,0.922675387296324,0.998696642611305),
(1.,0.923879532511287,1.,0.923879532511287,1.,0.923879532511287,1.,0.923879532511287,
1.,0.923879532511287,1.,0.923879532511287,1.,0.923879532511287,1.,0.923879532511287,
1.,0.923879532511287,1.,0.923879532511287,1.,0.923879532511287,1.,0.923879532511287,
1.,0.923879532511287,1.,0.923879532511287,1.,0.923879532511287,1.,0.923879532511287,
1.,0.923879532511287,1.,0.923879532511287,1.,0.923879532511287,1.,0.923879532511287,
1.,0.923879532511287,1.,0.923879532511287,1.,0.923879532511287,1.,0.923879532511287,
1.,0.923879532511287,1.,0.923879532511287,1.,0.923879532511287,1.,0.923879532511287,
1.,0.923879532511287,1.,0.923879532511287,1.,0.923879532511287,1.,0.923879532511287,
1.,0.923879532511287,1.,0.923879532511287,1.,0.923879532511287,1.,0.923879532511287,
1.,0.923879532511287,1.,0.923879532511287,1.,0.923879532511287,1.,0.923879532511287,
1.,0.923879532511287,1.,0.923879532511287,1.,0.923879532511287,1.,0.923879532511287,
1.,0.923879532511287,1.,0.923879532511287,1.,0.923879532511287,1.,0.923879532511287,
1.,0.923879532511287,1.,0.923879532511287,1.,0.923879532511287,1.,0.923879532511287,
1.,0.923879532511287,1.,0.923879532511287,1.,0.923879532511287,1.,0.923879532511287,
1.,0.923879532511287,1.,0.923879532511287,1.,0.923879532511287,1.,0.923879532511287,
1.,0.923879532511287,1.,0.923879532511287,1.,0.923879532511287,1.,0.923879532511287,
1.,0.923879532511287,1.,0.923879532511287,1.,0.923879532511287,1.,0.923879532511287,
1.,0.923879532511287,1.,0.923879532511287,1.,0.923879532511287,1.,0.923879532511287,
1.,0.923879532511287,1.,0.923879532511287,1.,0.923879532511287,1.,0.923879532511287,
1.,0.923879532511287,1.,0.923879532511287,1.,0.923879532511287,1.,0.923879532511287,
1.)))
REPRESENTATION_ITEM('')
SURFACE()
);
#581=(
BOUNDED_SURFACE()
B_SPLINE_SURFACE(1,2,((#31294,#31295,#31296,#31297,#31298,#31299,#31300,
#31301,#31302,#31303,#31304,#31305,#31306,#31307,#31308,#31309,#31310,#31311,
#31312,#31313,#31314,#31315,#31316,#31317,#31318,#31319,#31320,#31321,#31322,
#31323,#31324,#31325,#31326,#31327,#31328,#31329,#31330,#31331,#31332,#31333,
#31334,#31335,#31336,#31337,#31338,#31339,#31340,#31341,#31342,#31343,#31344,
#31345,#31346,#31347,#31348,#31349,#31350,#31351,#31352,#31353,#31354,#31355,
#31356,#31357,#31358,#31359,#31360,#31361,#31362,#31363,#31364,#31365,#31366,
#31367,#31368,#31369,#31370,#31371,#31372,#31373,#31374,#31375,#31376,#31377,
#31378,#31379,#31380,#31381,#31382,#31383,#31384,#31385,#31386,#31387,#31388,
#31389,#31390,#31391,#31392,#31393,#31394,#31395,#31396,#31397,#31398,#31399,
#31400,#31401,#31402,#31403,#31404,#31405,#31406,#31407,#31408,#31409,#31410,
#31411,#31412,#31413,#31414,#31415,#31416,#31417,#31418,#31419,#31420,#31421,
#31422,#31423,#31424,#31425,#31426,#31427,#31428,#31429,#31430,#31431,#31432,
#31433,#31434,#31435,#31436,#31437,#31438,#31439,#31440,#31441,#31442,#31443,
#31444,#31445,#31446,#31447,#31448,#31449,#31450,#31451,#31452,#31453,#31454),
(#31455,#31456,#31457,#31458,#31459,#31460,#31461,#31462,#31463,#31464,
#31465,#31466,#31467,#31468,#31469,#31470,#31471,#31472,#31473,#31474,#31475,
#31476,#31477,#31478,#31479,#31480,#31481,#31482,#31483,#31484,#31485,#31486,
#31487,#31488,#31489,#31490,#31491,#31492,#31493,#31494,#31495,#31496,#31497,
#31498,#31499,#31500,#31501,#31502,#31503,#31504,#31505,#31506,#31507,#31508,
#31509,#31510,#31511,#31512,#31513,#31514,#31515,#31516,#31517,#31518,#31519,
#31520,#31521,#31522,#31523,#31524,#31525,#31526,#31527,#31528,#31529,#31530,
#31531,#31532,#31533,#31534,#31535,#31536,#31537,#31538,#31539,#31540,#31541,
#31542,#31543,#31544,#31545,#31546,#31547,#31548,#31549,#31550,#31551,#31552,
#31553,#31554,#31555,#31556,#31557,#31558,#31559,#31560,#31561,#31562,#31563,
#31564,#31565,#31566,#31567,#31568,#31569,#31570,#31571,#31572,#31573,#31574,
#31575,#31576,#31577,#31578,#31579,#31580,#31581,#31582,#31583,#31584,#31585,
#31586,#31587,#31588,#31589,#31590,#31591,#31592,#31593,#31594,#31595,#31596,
#31597,#31598,#31599,#31600,#31601,#31602,#31603,#31604,#31605,#31606,#31607,
#31608,#31609,#31610,#31611,#31612,#31613,#31614,#31615)),.UNSPECIFIED.,
 .F.,.F.,.F.)
B_SPLINE_SURFACE_WITH_KNOTS((2,2),(3,2,2,2,2,2,2,2,2,2,2,2,2,2,2,2,2,2,
2,2,2,2,2,2,2,2,2,2,2,2,2,2,2,2,2,2,2,2,2,2,2,2,2,2,2,2,2,2,2,2,2,2,2,2,
2,2,2,2,2,2,2,2,2,2,2,2,2,2,2,2,2,2,2,2,2,2,2,2,2,2,3),(0.,1.00000731743925),
(0.,0.0125,0.025,0.0375,0.05,0.0625,0.075,0.0875,0.1,0.1125,0.125,0.1375,
0.15,0.1625,0.175,0.1875,0.2,0.2125,0.225,0.2375,0.25,0.2625,0.275,0.2875,
0.3,0.3125,0.325,0.3375,0.35,0.3625,0.375,0.3875,0.4,0.4125,0.425,0.4375,
0.45,0.4625,0.475,0.4875,0.5,0.5125,0.525,0.5375,0.55,0.5625,0.575,0.5875,
0.6,0.6125,0.625,0.6375,0.65,0.6625,0.675,0.6875,0.7,0.7125,0.725,0.7375,
0.75,0.7625,0.775,0.7875,0.8,0.8125,0.825,0.8375,0.85,0.8625,0.875,0.8875,
0.9,0.9125,0.925,0.9375,0.95,0.9625,0.975,0.9875,1.),.UNSPECIFIED.)
GEOMETRIC_REPRESENTATION_ITEM()
RATIONAL_B_SPLINE_SURFACE(((1.,0.923879532511287,1.,0.923879532511287,1.,
0.923879532511287,1.,0.923879532511287,1.,0.923879532511287,1.,0.923879532511287,
1.,0.923879532511287,1.,0.923879532511287,1.,0.923879532511287,1.,0.923879532511287,
1.,0.923879532511287,1.,0.923879532511287,1.,0.923879532511287,1.,0.923879532511287,
1.,0.923879532511287,1.,0.923879532511287,1.,0.923879532511287,1.,0.923879532511287,
1.,0.923879532511287,1.,0.923879532511287,1.,0.923879532511287,1.,0.923879532511287,
1.,0.923879532511287,1.,0.923879532511287,1.,0.923879532511287,1.,0.923879532511287,
1.,0.923879532511287,1.,0.923879532511287,1.,0.923879532511287,1.,0.923879532511287,
1.,0.923879532511287,1.,0.923879532511287,1.,0.923879532511287,1.,0.923879532511287,
1.,0.923879532511287,1.,0.923879532511287,1.,0.923879532511287,1.,0.923879532511287,
1.,0.923879532511287,1.,0.923879532511287,1.,0.923879532511287,1.,0.923879532511287,
1.,0.923879532511287,1.,0.923879532511287,1.,0.923879532511287,1.,0.923879532511287,
1.,0.923879532511287,1.,0.923879532511287,1.,0.923879532511287,1.,0.923879532511287,
1.,0.923879532511287,1.,0.923879532511287,1.,0.923879532511287,1.,0.923879532511287,
1.,0.923879532511287,1.,0.923879532511287,1.,0.923879532511287,1.,0.923879532511287,
1.,0.923879532511287,1.,0.923879532511287,1.,0.923879532511287,1.,0.923879532511287,
1.,0.923879532511287,1.,0.923879532511287,1.,0.923879532511287,1.,0.923879532511287,
1.,0.923879532511287,1.,0.923879532511287,1.,0.923879532511287,1.,0.923879532511287,
1.,0.923879532511287,1.,0.923879532511287,1.,0.923879532511287,1.,0.923879532511287,
1.,0.923879532511287,1.,0.923879532511287,1.,0.923879532511287,1.,0.923879532511287,
1.,0.923879532511287,1.,0.923879532511287,1.),(1.,0.923879532511287,1.,
0.923879532511287,1.,0.923879532511287,1.,0.923879532511287,1.,0.923879532511287,
1.,0.923879532511287,1.,0.923879532511287,1.,0.923879532511287,1.,0.923879532511287,
1.,0.923879532511287,1.,0.923879532511287,1.,0.923879532511287,1.,0.923879532511287,
1.,0.923879532511287,1.,0.923879532511287,1.,0.923879532511287,1.,0.923879532511287,
1.,0.923879532511287,1.,0.923879532511287,1.,0.923879532511287,1.,0.923879532511287,
1.,0.923879532511287,1.,0.923879532511287,1.,0.923879532511287,1.,0.923879532511287,
1.,0.923879532511287,1.,0.923879532511287,1.,0.923879532511287,1.,0.923879532511287,
1.,0.923879532511287,1.,0.923879532511287,1.,0.923879532511287,1.,0.923879532511287,
1.,0.923879532511287,1.,0.923879532511287,1.,0.923879532511287,1.,0.923879532511287,
1.,0.923879532511287,1.,0.923879532511287,1.,0.923879532511287,1.,0.923879532511287,
1.,0.923879532511287,1.,0.923879532511287,1.,0.923879532511287,1.,0.923879532511287,
1.,0.923879532511287,1.,0.923879532511287,1.,0.923879532511287,1.,0.923879532511287,
1.,0.923879532511287,1.,0.923879532511287,1.,0.923879532511287,1.,0.923879532511287,
1.,0.923879532511287,1.,0.923879532511287,1.,0.923879532511287,1.,0.923879532511287,
1.,0.923879532511287,1.,0.923879532511287,1.,0.923879532511287,1.,0.923879532511287,
1.,0.923879532511287,1.,0.923879532511287,1.,0.923879532511287,1.,0.923879532511287,
1.,0.923879532511287,1.,0.923879532511287,1.,0.923879532511287,1.,0.923879532511287,
1.,0.923879532511287,1.,0.923879532511287,1.,0.923879532511287,1.,0.923879532511287,
1.,0.923879532511287,1.,0.923879532511287,1.,0.923879532511287,1.,0.923879532511287,
1.,0.923879532511287,1.,0.923879532511287,1.,0.923879532511287,1.)))
REPRESENTATION_ITEM('')
SURFACE()
);
#582=(
BOUNDED_SURFACE()
B_SPLINE_SURFACE(3,2,((#31621,#31622,#31623,#31624,#31625,#31626,#31627,
#31628,#31629,#31630,#31631,#31632,#31633,#31634,#31635,#31636,#31637,#31638,
#31639,#31640,#31641,#31642,#31643,#31644,#31645,#31646,#31647,#31648,#31649,
#31650,#31651,#31652,#31653,#31654,#31655,#31656,#31657,#31658,#31659,#31660,
#31661,#31662,#31663,#31664,#31665,#31666,#31667,#31668,#31669,#31670,#31671,
#31672,#31673,#31674,#31675,#31676,#31677,#31678,#31679,#31680,#31681,#31682,
#31683,#31684,#31685,#31686,#31687,#31688,#31689,#31690,#31691,#31692,#31693,
#31694,#31695,#31696,#31697,#31698,#31699,#31700,#31701,#31702,#31703,#31704,
#31705,#31706,#31707,#31708,#31709,#31710,#31711,#31712,#31713,#31714,#31715,
#31716,#31717,#31718,#31719,#31720,#31721,#31722,#31723,#31724,#31725,#31726,
#31727,#31728,#31729,#31730,#31731,#31732,#31733,#31734,#31735,#31736,#31737,
#31738,#31739,#31740,#31741,#31742,#31743,#31744,#31745,#31746,#31747,#31748,
#31749,#31750,#31751,#31752,#31753,#31754,#31755,#31756,#31757,#31758,#31759,
#31760,#31761,#31762,#31763,#31764,#31765,#31766,#31767,#31768,#31769,#31770,
#31771,#31772,#31773,#31774,#31775,#31776,#31777,#31778,#31779,#31780,#31781),
(#31782,#31783,#31784,#31785,#31786,#31787,#31788,#31789,#31790,#31791,
#31792,#31793,#31794,#31795,#31796,#31797,#31798,#31799,#31800,#31801,#31802,
#31803,#31804,#31805,#31806,#31807,#31808,#31809,#31810,#31811,#31812,#31813,
#31814,#31815,#31816,#31817,#31818,#31819,#31820,#31821,#31822,#31823,#31824,
#31825,#31826,#31827,#31828,#31829,#31830,#31831,#31832,#31833,#31834,#31835,
#31836,#31837,#31838,#31839,#31840,#31841,#31842,#31843,#31844,#31845,#31846,
#31847,#31848,#31849,#31850,#31851,#31852,#31853,#31854,#31855,#31856,#31857,
#31858,#31859,#31860,#31861,#31862,#31863,#31864,#31865,#31866,#31867,#31868,
#31869,#31870,#31871,#31872,#31873,#31874,#31875,#31876,#31877,#31878,#31879,
#31880,#31881,#31882,#31883,#31884,#31885,#31886,#31887,#31888,#31889,#31890,
#31891,#31892,#31893,#31894,#31895,#31896,#31897,#31898,#31899,#31900,#31901,
#31902,#31903,#31904,#31905,#31906,#31907,#31908,#31909,#31910,#31911,#31912,
#31913,#31914,#31915,#31916,#31917,#31918,#31919,#31920,#31921,#31922,#31923,
#31924,#31925,#31926,#31927,#31928,#31929,#31930,#31931,#31932,#31933,#31934,
#31935,#31936,#31937,#31938,#31939,#31940,#31941,#31942),(#31943,#31944,
#31945,#31946,#31947,#31948,#31949,#31950,#31951,#31952,#31953,#31954,#31955,
#31956,#31957,#31958,#31959,#31960,#31961,#31962,#31963,#31964,#31965,#31966,
#31967,#31968,#31969,#31970,#31971,#31972,#31973,#31974,#31975,#31976,#31977,
#31978,#31979,#31980,#31981,#31982,#31983,#31984,#31985,#31986,#31987,#31988,
#31989,#31990,#31991,#31992,#31993,#31994,#31995,#31996,#31997,#31998,#31999,
#32000,#32001,#32002,#32003,#32004,#32005,#32006,#32007,#32008,#32009,#32010,
#32011,#32012,#32013,#32014,#32015,#32016,#32017,#32018,#32019,#32020,#32021,
#32022,#32023,#32024,#32025,#32026,#32027,#32028,#32029,#32030,#32031,#32032,
#32033,#32034,#32035,#32036,#32037,#32038,#32039,#32040,#32041,#32042,#32043,
#32044,#32045,#32046,#32047,#32048,#32049,#32050,#32051,#32052,#32053,#32054,
#32055,#32056,#32057,#32058,#32059,#32060,#32061,#32062,#32063,#32064,#32065,
#32066,#32067,#32068,#32069,#32070,#32071,#32072,#32073,#32074,#32075,#32076,
#32077,#32078,#32079,#32080,#32081,#32082,#32083,#32084,#32085,#32086,#32087,
#32088,#32089,#32090,#32091,#32092,#32093,#32094,#32095,#32096,#32097,#32098,
#32099,#32100,#32101,#32102,#32103),(#32104,#32105,#32106,#32107,#32108,
#32109,#32110,#32111,#32112,#32113,#32114,#32115,#32116,#32117,#32118,#32119,
#32120,#32121,#32122,#32123,#32124,#32125,#32126,#32127,#32128,#32129,#32130,
#32131,#32132,#32133,#32134,#32135,#32136,#32137,#32138,#32139,#32140,#32141,
#32142,#32143,#32144,#32145,#32146,#32147,#32148,#32149,#32150,#32151,#32152,
#32153,#32154,#32155,#32156,#32157,#32158,#32159,#32160,#32161,#32162,#32163,
#32164,#32165,#32166,#32167,#32168,#32169,#32170,#32171,#32172,#32173,#32174,
#32175,#32176,#32177,#32178,#32179,#32180,#32181,#32182,#32183,#32184,#32185,
#32186,#32187,#32188,#32189,#32190,#32191,#32192,#32193,#32194,#32195,#32196,
#32197,#32198,#32199,#32200,#32201,#32202,#32203,#32204,#32205,#32206,#32207,
#32208,#32209,#32210,#32211,#32212,#32213,#32214,#32215,#32216,#32217,#32218,
#32219,#32220,#32221,#32222,#32223,#32224,#32225,#32226,#32227,#32228,#32229,
#32230,#32231,#32232,#32233,#32234,#32235,#32236,#32237,#32238,#32239,#32240,
#32241,#32242,#32243,#32244,#32245,#32246,#32247,#32248,#32249,#32250,#32251,
#32252,#32253,#32254,#32255,#32256,#32257,#32258,#32259,#32260,#32261,#32262,
#32263,#32264)),.UNSPECIFIED.,.F.,.F.,.F.)
B_SPLINE_SURFACE_WITH_KNOTS((4,4),(3,2,2,2,2,2,2,2,2,2,2,2,2,2,2,2,2,2,
2,2,2,2,2,2,2,2,2,2,2,2,2,2,2,2,2,2,2,2,2,2,2,2,2,2,2,2,2,2,2,2,2,2,2,2,
2,2,2,2,2,2,2,2,2,2,2,2,2,2,2,2,2,2,2,2,2,2,2,2,2,2,3),(0.,1.),(0.,0.0125,
0.025,0.0375,0.05,0.0625,0.075,0.0875,0.1,0.1125,0.125,0.1375,0.15,0.1625,
0.175,0.1875,0.2,0.2125,0.225,0.2375,0.25,0.2625,0.275,0.2875,0.3,0.3125,
0.325,0.3375,0.35,0.3625,0.375,0.3875,0.4,0.4125,0.425,0.4375,0.45,0.4625,
0.475,0.4875,0.5,0.5125,0.525,0.5375,0.55,0.5625,0.575,0.5875,0.6,0.6125,
0.625,0.6375,0.65,0.6625,0.675,0.6875,0.7,0.7125,0.725,0.7375,0.75,0.7625,
0.775,0.7875,0.8,0.8125,0.825,0.8375,0.85,0.8625,0.875,0.8875,0.9,0.9125,
0.925,0.9375,0.95,0.9625,0.975,0.9875,1.),.UNSPECIFIED.)
GEOMETRIC_REPRESENTATION_ITEM()
RATIONAL_B_SPLINE_SURFACE(((1.,0.923879532511287,1.,0.923879532511287,1.,
0.923879532511287,1.,0.923879532511287,1.,0.923879532511287,1.,0.923879532511287,
1.,0.923879532511287,1.,0.923879532511287,1.,0.923879532511287,1.,0.923879532511287,
1.,0.923879532511287,1.,0.923879532511287,1.,0.923879532511287,1.,0.923879532511287,
1.,0.923879532511287,1.,0.923879532511287,1.,0.923879532511287,1.,0.923879532511287,
1.,0.923879532511287,1.,0.923879532511287,1.,0.923879532511287,1.,0.923879532511287,
1.,0.923879532511287,1.,0.923879532511287,1.,0.923879532511287,1.,0.923879532511287,
1.,0.923879532511287,1.,0.923879532511287,1.,0.923879532511287,1.,0.923879532511287,
1.,0.923879532511287,1.,0.923879532511287,1.,0.923879532511287,1.,0.923879532511287,
1.,0.923879532511287,1.,0.923879532511287,1.,0.923879532511287,1.,0.923879532511287,
1.,0.923879532511287,1.,0.923879532511287,1.,0.923879532511287,1.,0.923879532511287,
1.,0.923879532511287,1.,0.923879532511287,1.,0.923879532511287,1.,0.923879532511287,
1.,0.923879532511287,1.,0.923879532511287,1.,0.923879532511287,1.,0.923879532511287,
1.,0.923879532511287,1.,0.923879532511287,1.,0.923879532511287,1.,0.923879532511287,
1.,0.923879532511287,1.,0.923879532511287,1.,0.923879532511287,1.,0.923879532511287,
1.,0.923879532511287,1.,0.923879532511287,1.,0.923879532511287,1.,0.923879532511287,
1.,0.923879532511287,1.,0.923879532511287,1.,0.923879532511287,1.,0.923879532511287,
1.,0.923879532511287,1.,0.923879532511287,1.,0.923879532511287,1.,0.923879532511287,
1.,0.923879532511287,1.,0.923879532511287,1.,0.923879532511287,1.,0.923879532511287,
1.,0.923879532511287,1.,0.923879532511287,1.,0.923879532511287,1.,0.923879532511287,
1.,0.923879532511287,1.,0.923879532511287,1.),(0.998696642611305,0.922675387296324,
0.998696642611305,0.922675387296324,0.998696642611305,0.922675387296324,
0.998696642611305,0.922675387296324,0.998696642611305,0.922675387296324,
0.998696642611305,0.922675387296324,0.998696642611305,0.922675387296324,
0.998696642611305,0.922675387296324,0.998696642611305,0.922675387296324,
0.998696642611305,0.922675387296324,0.998696642611305,0.922675387296324,
0.998696642611305,0.922675387296324,0.998696642611305,0.922675387296324,
0.998696642611305,0.922675387296324,0.998696642611305,0.922675387296324,
0.998696642611305,0.922675387296324,0.998696642611305,0.922675387296324,
0.998696642611305,0.922675387296324,0.998696642611305,0.922675387296324,
0.998696642611305,0.922675387296324,0.998696642611305,0.922675387296324,
0.998696642611305,0.922675387296324,0.998696642611305,0.922675387296324,
0.998696642611305,0.922675387296324,0.998696642611305,0.922675387296324,
0.998696642611305,0.922675387296324,0.998696642611305,0.922675387296324,
0.998696642611305,0.922675387296324,0.998696642611305,0.922675387296324,
0.998696642611305,0.922675387296324,0.998696642611305,0.922675387296324,
0.998696642611305,0.922675387296324,0.998696642611305,0.922675387296324,
0.998696642611305,0.922675387296324,0.998696642611305,0.922675387296324,
0.998696642611305,0.922675387296324,0.998696642611305,0.922675387296324,
0.998696642611305,0.922675387296324,0.998696642611305,0.922675387296324,
0.998696642611305,0.922675387296324,0.998696642611305,0.922675387296324,
0.998696642611305,0.922675387296324,0.998696642611305,0.922675387296324,
0.998696642611305,0.922675387296324,0.998696642611305,0.922675387296324,
0.998696642611305,0.922675387296324,0.998696642611305,0.922675387296324,
0.998696642611305,0.922675387296324,0.998696642611305,0.922675387296324,
0.998696642611305,0.922675387296324,0.998696642611305,0.922675387296324,
0.998696642611305,0.922675387296324,0.998696642611305,0.922675387296324,
0.998696642611305,0.922675387296324,0.998696642611305,0.922675387296324,
0.998696642611305,0.922675387296324,0.998696642611305,0.922675387296324,
0.998696642611305,0.922675387296324,0.998696642611305,0.922675387296324,
0.998696642611305,0.922675387296324,0.998696642611305,0.922675387296324,
0.998696642611305,0.922675387296324,0.998696642611305,0.922675387296324,
0.998696642611305,0.922675387296324,0.998696642611305,0.922675387296324,
0.998696642611305,0.922675387296324,0.998696642611305,0.922675387296324,
0.998696642611305,0.922675387296324,0.998696642611305,0.922675387296324,
0.998696642611305,0.922675387296324,0.998696642611305,0.922675387296324,
0.998696642611305,0.922675387296324,0.998696642611305,0.922675387296324,
0.998696642611305,0.922675387296324,0.998696642611305,0.922675387296324,
0.998696642611305,0.922675387296324,0.998696642611305,0.922675387296324,
0.998696642611305,0.922675387296324,0.998696642611305,0.922675387296324,
0.998696642611305,0.922675387296324,0.998696642611305),(0.998696642611305,
0.922675387296324,0.998696642611305,0.922675387296324,0.998696642611305,
0.922675387296324,0.998696642611305,0.922675387296324,0.998696642611305,
0.922675387296324,0.998696642611305,0.922675387296324,0.998696642611305,
0.922675387296324,0.998696642611305,0.922675387296324,0.998696642611305,
0.922675387296324,0.998696642611305,0.922675387296324,0.998696642611305,
0.922675387296324,0.998696642611305,0.922675387296324,0.998696642611305,
0.922675387296324,0.998696642611305,0.922675387296324,0.998696642611305,
0.922675387296324,0.998696642611305,0.922675387296324,0.998696642611305,
0.922675387296324,0.998696642611305,0.922675387296324,0.998696642611305,
0.922675387296324,0.998696642611305,0.922675387296324,0.998696642611305,
0.922675387296324,0.998696642611305,0.922675387296324,0.998696642611305,
0.922675387296324,0.998696642611305,0.922675387296324,0.998696642611305,
0.922675387296324,0.998696642611305,0.922675387296324,0.998696642611305,
0.922675387296324,0.998696642611305,0.922675387296324,0.998696642611305,
0.922675387296324,0.998696642611305,0.922675387296324,0.998696642611305,
0.922675387296324,0.998696642611305,0.922675387296324,0.998696642611305,
0.922675387296324,0.998696642611305,0.922675387296324,0.998696642611305,
0.922675387296324,0.998696642611305,0.922675387296324,0.998696642611305,
0.922675387296324,0.998696642611305,0.922675387296324,0.998696642611305,
0.922675387296324,0.998696642611305,0.922675387296324,0.998696642611305,
0.922675387296324,0.998696642611305,0.922675387296324,0.998696642611305,
0.922675387296324,0.998696642611305,0.922675387296324,0.998696642611305,
0.922675387296324,0.998696642611305,0.922675387296324,0.998696642611305,
0.922675387296324,0.998696642611305,0.922675387296324,0.998696642611305,
0.922675387296324,0.998696642611305,0.922675387296324,0.998696642611305,
0.922675387296324,0.998696642611305,0.922675387296324,0.998696642611305,
0.922675387296324,0.998696642611305,0.922675387296324,0.998696642611305,
0.922675387296324,0.998696642611305,0.922675387296324,0.998696642611305,
0.922675387296324,0.998696642611305,0.922675387296324,0.998696642611305,
0.922675387296324,0.998696642611305,0.922675387296324,0.998696642611305,
0.922675387296324,0.998696642611305,0.922675387296324,0.998696642611305,
0.922675387296324,0.998696642611305,0.922675387296324,0.998696642611305,
0.922675387296324,0.998696642611305,0.922675387296324,0.998696642611305,
0.922675387296324,0.998696642611305,0.922675387296324,0.998696642611305,
0.922675387296324,0.998696642611305,0.922675387296324,0.998696642611305,
0.922675387296324,0.998696642611305,0.922675387296324,0.998696642611305,
0.922675387296324,0.998696642611305,0.922675387296324,0.998696642611305,
0.922675387296324,0.998696642611305,0.922675387296324,0.998696642611305,
0.922675387296324,0.998696642611305,0.922675387296324,0.998696642611305,
0.922675387296324,0.998696642611305,0.922675387296324,0.998696642611305),
(1.,0.923879532511287,1.,0.923879532511287,1.,0.923879532511287,1.,0.923879532511287,
1.,0.923879532511287,1.,0.923879532511287,1.,0.923879532511287,1.,0.923879532511287,
1.,0.923879532511287,1.,0.923879532511287,1.,0.923879532511287,1.,0.923879532511287,
1.,0.923879532511287,1.,0.923879532511287,1.,0.923879532511287,1.,0.923879532511287,
1.,0.923879532511287,1.,0.923879532511287,1.,0.923879532511287,1.,0.923879532511287,
1.,0.923879532511287,1.,0.923879532511287,1.,0.923879532511287,1.,0.923879532511287,
1.,0.923879532511287,1.,0.923879532511287,1.,0.923879532511287,1.,0.923879532511287,
1.,0.923879532511287,1.,0.923879532511287,1.,0.923879532511287,1.,0.923879532511287,
1.,0.923879532511287,1.,0.923879532511287,1.,0.923879532511287,1.,0.923879532511287,
1.,0.923879532511287,1.,0.923879532511287,1.,0.923879532511287,1.,0.923879532511287,
1.,0.923879532511287,1.,0.923879532511287,1.,0.923879532511287,1.,0.923879532511287,
1.,0.923879532511287,1.,0.923879532511287,1.,0.923879532511287,1.,0.923879532511287,
1.,0.923879532511287,1.,0.923879532511287,1.,0.923879532511287,1.,0.923879532511287,
1.,0.923879532511287,1.,0.923879532511287,1.,0.923879532511287,1.,0.923879532511287,
1.,0.923879532511287,1.,0.923879532511287,1.,0.923879532511287,1.,0.923879532511287,
1.,0.923879532511287,1.,0.923879532511287,1.,0.923879532511287,1.,0.923879532511287,
1.,0.923879532511287,1.,0.923879532511287,1.,0.923879532511287,1.,0.923879532511287,
1.,0.923879532511287,1.,0.923879532511287,1.,0.923879532511287,1.,0.923879532511287,
1.,0.923879532511287,1.,0.923879532511287,1.,0.923879532511287,1.,0.923879532511287,
1.,0.923879532511287,1.,0.923879532511287,1.,0.923879532511287,1.,0.923879532511287,
1.)))
REPRESENTATION_ITEM('')
SURFACE()
);
#583=(
BOUNDED_SURFACE()
B_SPLINE_SURFACE(3,2,((#32268,#32269,#32270),(#32271,#32272,#32273),(#32274,
#32275,#32276),(#32277,#32278,#32279)),.UNSPECIFIED.,.F.,.F.,.F.)
B_SPLINE_SURFACE_WITH_KNOTS((4,4),(3,3),(-8.67361737988404E-18,0.00176076821392877),
(0.,1.),.UNSPECIFIED.)
GEOMETRIC_REPRESENTATION_ITEM()
RATIONAL_B_SPLINE_SURFACE(((1.,0.605017435075385,1.),(1.,0.607455453482648,
1.),(1.,0.609590739470685,1.),(1.,0.611227253379469,1.)))
REPRESENTATION_ITEM('')
SURFACE()
);
#584=(
BOUNDED_SURFACE()
B_SPLINE_SURFACE(3,2,((#32281,#32282,#32283),(#32284,#32285,#32286),(#32287,
#32288,#32289),(#32290,#32291,#32292),(#32293,#32294,#32295),(#32296,#32297,
#32298)),.UNSPECIFIED.,.F.,.F.,.F.)
B_SPLINE_SURFACE_WITH_KNOTS((4,2,4),(3,3),(3.35018471298021E-17,0.000541903658604953,
0.00108380731720987),(0.,1.),.UNSPECIFIED.)
GEOMETRIC_REPRESENTATION_ITEM()
RATIONAL_B_SPLINE_SURFACE(((1.,0.707106781186545,1.),(1.,0.687098191636224,
1.),(1.,0.66678877037223,1.),(1.,0.631310893346957,1.),(1.,0.615653630066085,
1.),(1.,0.605017435075385,1.)))
REPRESENTATION_ITEM('')
SURFACE()
);
#585=(
BOUNDED_SURFACE()
B_SPLINE_SURFACE(3,2,((#32311,#32312,#32313),(#32314,#32315,#32316),(#32317,
#32318,#32319),(#32320,#32321,#32322),(#32323,#32324,#32325),(#32326,#32327,
#32328)),.UNSPECIFIED.,.F.,.F.,.F.)
B_SPLINE_SURFACE_WITH_KNOTS((4,2,4),(3,3),(-2.0870891820346E-17,0.000541486237413509,
0.00108297247482704),(0.,1.),.UNSPECIFIED.)
GEOMETRIC_REPRESENTATION_ITEM()
RATIONAL_B_SPLINE_SURFACE(((1.,0.605017435075385,1.),(1.,0.615653519651203,
1.),(1.,0.631258339490859,1.),(1.,0.666776937440384,1.),(1.,0.687023379357965,
1.),(1.,0.707106781186545,1.)))
REPRESENTATION_ITEM('')
SURFACE()
);
#586=(
BOUNDED_SURFACE()
B_SPLINE_SURFACE(3,2,((#32330,#32331,#32332),(#32333,#32334,#32335),(#32336,
#32337,#32338),(#32339,#32340,#32341)),.UNSPECIFIED.,.F.,.F.,.F.)
B_SPLINE_SURFACE_WITH_KNOTS((4,4),(3,3),(1.47451495458029E-17,0.00176076821392879),
(0.,1.),.UNSPECIFIED.)
GEOMETRIC_REPRESENTATION_ITEM()
RATIONAL_B_SPLINE_SURFACE(((1.,0.605017435075385,1.),(1.,0.607455453482656,
1.),(1.,0.609590739470667,1.),(1.,0.611227253379484,1.)))
REPRESENTATION_ITEM('')
SURFACE()
);
#587=(
BOUNDED_SURFACE()
B_SPLINE_SURFACE(1,2,((#37408,#37409,#37410,#37411,#37412,#37413,#37414,
#37415,#37416,#37417,#37418,#37419,#37420,#37421,#37422,#37423,#37424,#37425,
#37426,#37427,#37428,#37429,#37430,#37431,#37432,#37433,#37434,#37435,#37436,
#37437,#37438,#37439,#37440,#37441,#37442,#37443,#37444,#37445,#37446,#37447,
#37448,#37449,#37450,#37451,#37452,#37453,#37454,#37455,#37456,#37457,#37458,
#37459,#37460,#37461,#37462,#37463,#37464,#37465,#37466,#37467,#37468,#37469,
#37470,#37471,#37472,#37473,#37474,#37475,#37476,#37477,#37478,#37479,#37480,
#37481,#37482,#37483,#37484,#37485,#37486,#37487,#37488,#37489,#37490,#37491,
#37492,#37493,#37494,#37495,#37496,#37497,#37498,#37499,#37500,#37501,#37502,
#37503,#37504,#37505,#37506,#37507,#37508,#37509,#37510,#37511,#37512,#37513,
#37514,#37515,#37516,#37517,#37518,#37519,#37520,#37521,#37522,#37523,#37524,
#37525,#37526,#37527,#37528,#37529,#37530,#37531,#37532,#37533,#37534,#37535,
#37536,#37537,#37538,#37539,#37540,#37541,#37542,#37543,#37544,#37545,#37546,
#37547,#37548,#37549,#37550,#37551,#37552,#37553,#37554,#37555,#37556,#37557,
#37558,#37559,#37560,#37561,#37562,#37563,#37564,#37565,#37566,#37567,#37568,
#37569,#37570,#37571,#37572,#37573,#37574,#37575,#37576,#37577,#37578,#37579,
#37580,#37581,#37582,#37583,#37584,#37585,#37586,#37587,#37588,#37589,#37590,
#37591,#37592,#37593,#37594,#37595,#37596,#37597,#37598,#37599,#37600,#37601,
#37602,#37603,#37604,#37605,#37606,#37607,#37608,#37609,#37610,#37611,#37612,
#37613,#37614,#37615,#37616,#37617,#37618,#37619,#37620,#37621,#37622,#37623,
#37624,#37625,#37626,#37627,#37628,#37629,#37630,#37631,#37632,#37633,#37634,
#37635,#37636,#37637,#37638,#37639,#37640,#37641,#37642,#37643,#37644,#37645,
#37646,#37647,#37648,#37649,#37650,#37651,#37652,#37653,#37654,#37655,#37656,
#37657,#37658,#37659,#37660,#37661,#37662,#37663,#37664,#37665,#37666,#37667,
#37668,#37669,#37670,#37671,#37672,#37673,#37674,#37675,#37676,#37677,#37678,
#37679,#37680,#37681,#37682,#37683,#37684,#37685,#37686,#37687,#37688,#37689,
#37690,#37691,#37692,#37693,#37694,#37695,#37696,#37697,#37698,#37699,#37700,
#37701,#37702,#37703,#37704,#37705,#37706,#37707,#37708,#37709,#37710,#37711,
#37712,#37713,#37714,#37715,#37716,#37717,#37718,#37719,#37720,#37721,#37722,
#37723,#37724,#37725,#37726,#37727,#37728,#37729,#37730,#37731,#37732,#37733,
#37734,#37735,#37736,#37737,#37738,#37739,#37740,#37741,#37742,#37743,#37744,
#37745,#37746,#37747,#37748,#37749,#37750,#37751,#37752,#37753,#37754,#37755,
#37756,#37757,#37758,#37759,#37760,#37761,#37762,#37763,#37764,#37765,#37766,
#37767,#37768,#37769,#37770,#37771,#37772,#37773,#37774,#37775,#37776,#37777,
#37778,#37779,#37780,#37781,#37782,#37783,#37784,#37785,#37786,#37787,#37788,
#37789,#37790,#37791,#37792,#37793,#37794,#37795,#37796,#37797,#37798,#37799,
#37800,#37801,#37802,#37803,#37804,#37805,#37806,#37807,#37808,#37809,#37810,
#37811,#37812,#37813,#37814,#37815,#37816,#37817,#37818,#37819,#37820,#37821,
#37822,#37823,#37824,#37825,#37826,#37827,#37828,#37829,#37830,#37831,#37832,
#37833,#37834,#37835,#37836,#37837,#37838,#37839,#37840,#37841,#37842,#37843,
#37844,#37845,#37846,#37847,#37848,#37849,#37850,#37851,#37852,#37853,#37854,
#37855,#37856,#37857,#37858,#37859,#37860,#37861,#37862,#37863,#37864,#37865,
#37866,#37867,#37868,#37869,#37870,#37871,#37872,#37873,#37874,#37875,#37876,
#37877,#37878,#37879,#37880,#37881,#37882,#37883,#37884,#37885,#37886,#37887,
#37888,#37889,#37890,#37891,#37892,#37893,#37894,#37895,#37896,#37897,#37898,
#37899,#37900,#37901,#37902,#37903,#37904,#37905,#37906,#37907,#37908,#37909,
#37910,#37911,#37912,#37913,#37914,#37915,#37916,#37917,#37918,#37919,#37920,
#37921,#37922,#37923,#37924,#37925,#37926,#37927,#37928,#37929,#37930,#37931,
#37932,#37933,#37934,#37935,#37936,#37937,#37938,#37939,#37940,#37941,#37942,
#37943,#37944,#37945,#37946,#37947,#37948,#37949,#37950,#37951,#37952,#37953,
#37954,#37955,#37956,#37957,#37958,#37959,#37960,#37961,#37962,#37963,#37964,
#37965,#37966,#37967,#37968,#37969,#37970,#37971,#37972,#37973,#37974,#37975,
#37976,#37977,#37978,#37979,#37980,#37981,#37982,#37983,#37984,#37985,#37986,
#37987,#37988,#37989,#37990,#37991,#37992,#37993,#37994,#37995,#37996,#37997,
#37998,#37999,#38000,#38001,#38002,#38003,#38004,#38005,#38006,#38007,#38008,
#38009,#38010,#38011,#38012,#38013,#38014,#38015,#38016,#38017,#38018,#38019,
#38020,#38021,#38022,#38023,#38024,#38025,#38026,#38027,#38028,#38029,#38030,
#38031,#38032,#38033,#38034,#38035,#38036,#38037,#38038,#38039,#38040,#38041,
#38042,#38043,#38044,#38045,#38046,#38047,#38048,#38049,#38050,#38051,#38052,
#38053,#38054,#38055,#38056,#38057,#38058,#38059,#38060,#38061,#38062,#38063,
#38064,#38065,#38066,#38067,#38068,#38069,#38070,#38071,#38072,#38073,#38074,
#38075,#38076,#38077,#38078,#38079,#38080,#38081,#38082,#38083,#38084,#38085,
#38086,#38087,#38088,#38089,#38090,#38091,#38092,#38093,#38094,#38095,#38096,
#38097,#38098,#38099,#38100,#38101,#38102,#38103,#38104),(#38105,#38106,
#38107,#38108,#38109,#38110,#38111,#38112,#38113,#38114,#38115,#38116,#38117,
#38118,#38119,#38120,#38121,#38122,#38123,#38124,#38125,#38126,#38127,#38128,
#38129,#38130,#38131,#38132,#38133,#38134,#38135,#38136,#38137,#38138,#38139,
#38140,#38141,#38142,#38143,#38144,#38145,#38146,#38147,#38148,#38149,#38150,
#38151,#38152,#38153,#38154,#38155,#38156,#38157,#38158,#38159,#38160,#38161,
#38162,#38163,#38164,#38165,#38166,#38167,#38168,#38169,#38170,#38171,#38172,
#38173,#38174,#38175,#38176,#38177,#38178,#38179,#38180,#38181,#38182,#38183,
#38184,#38185,#38186,#38187,#38188,#38189,#38190,#38191,#38192,#38193,#38194,
#38195,#38196,#38197,#38198,#38199,#38200,#38201,#38202,#38203,#38204,#38205,
#38206,#38207,#38208,#38209,#38210,#38211,#38212,#38213,#38214,#38215,#38216,
#38217,#38218,#38219,#38220,#38221,#38222,#38223,#38224,#38225,#38226,#38227,
#38228,#38229,#38230,#38231,#38232,#38233,#38234,#38235,#38236,#38237,#38238,
#38239,#38240,#38241,#38242,#38243,#38244,#38245,#38246,#38247,#38248,#38249,
#38250,#38251,#38252,#38253,#38254,#38255,#38256,#38257,#38258,#38259,#38260,
#38261,#38262,#38263,#38264,#38265,#38266,#38267,#38268,#38269,#38270,#38271,
#38272,#38273,#38274,#38275,#38276,#38277,#38278,#38279,#38280,#38281,#38282,
#38283,#38284,#38285,#38286,#38287,#38288,#38289,#38290,#38291,#38292,#38293,
#38294,#38295,#38296,#38297,#38298,#38299,#38300,#38301,#38302,#38303,#38304,
#38305,#38306,#38307,#38308,#38309,#38310,#38311,#38312,#38313,#38314,#38315,
#38316,#38317,#38318,#38319,#38320,#38321,#38322,#38323,#38324,#38325,#38326,
#38327,#38328,#38329,#38330,#38331,#38332,#38333,#38334,#38335,#38336,#38337,
#38338,#38339,#38340,#38341,#38342,#38343,#38344,#38345,#38346,#38347,#38348,
#38349,#38350,#38351,#38352,#38353,#38354,#38355,#38356,#38357,#38358,#38359,
#38360,#38361,#38362,#38363,#38364,#38365,#38366,#38367,#38368,#38369,#38370,
#38371,#38372,#38373,#38374,#38375,#38376,#38377,#38378,#38379,#38380,#38381,
#38382,#38383,#38384,#38385,#38386,#38387,#38388,#38389,#38390,#38391,#38392,
#38393,#38394,#38395,#38396,#38397,#38398,#38399,#38400,#38401,#38402,#38403,
#38404,#38405,#38406,#38407,#38408,#38409,#38410,#38411,#38412,#38413,#38414,
#38415,#38416,#38417,#38418,#38419,#38420,#38421,#38422,#38423,#38424,#38425,
#38426,#38427,#38428,#38429,#38430,#38431,#38432,#38433,#38434,#38435,#38436,
#38437,#38438,#38439,#38440,#38441,#38442,#38443,#38444,#38445,#38446,#38447,
#38448,#38449,#38450,#38451,#38452,#38453,#38454,#38455,#38456,#38457,#38458,
#38459,#38460,#38461,#38462,#38463,#38464,#38465,#38466,#38467,#38468,#38469,
#38470,#38471,#38472,#38473,#38474,#38475,#38476,#38477,#38478,#38479,#38480,
#38481,#38482,#38483,#38484,#38485,#38486,#38487,#38488,#38489,#38490,#38491,
#38492,#38493,#38494,#38495,#38496,#38497,#38498,#38499,#38500,#38501,#38502,
#38503,#38504,#38505,#38506,#38507,#38508,#38509,#38510,#38511,#38512,#38513,
#38514,#38515,#38516,#38517,#38518,#38519,#38520,#38521,#38522,#38523,#38524,
#38525,#38526,#38527,#38528,#38529,#38530,#38531,#38532,#38533,#38534,#38535,
#38536,#38537,#38538,#38539,#38540,#38541,#38542,#38543,#38544,#38545,#38546,
#38547,#38548,#38549,#38550,#38551,#38552,#38553,#38554,#38555,#38556,#38557,
#38558,#38559,#38560,#38561,#38562,#38563,#38564,#38565,#38566,#38567,#38568,
#38569,#38570,#38571,#38572,#38573,#38574,#38575,#38576,#38577,#38578,#38579,
#38580,#38581,#38582,#38583,#38584,#38585,#38586,#38587,#38588,#38589,#38590,
#38591,#38592,#38593,#38594,#38595,#38596,#38597,#38598,#38599,#38600,#38601,
#38602,#38603,#38604,#38605,#38606,#38607,#38608,#38609,#38610,#38611,#38612,
#38613,#38614,#38615,#38616,#38617,#38618,#38619,#38620,#38621,#38622,#38623,
#38624,#38625,#38626,#38627,#38628,#38629,#38630,#38631,#38632,#38633,#38634,
#38635,#38636,#38637,#38638,#38639,#38640,#38641,#38642,#38643,#38644,#38645,
#38646,#38647,#38648,#38649,#38650,#38651,#38652,#38653,#38654,#38655,#38656,
#38657,#38658,#38659,#38660,#38661,#38662,#38663,#38664,#38665,#38666,#38667,
#38668,#38669,#38670,#38671,#38672,#38673,#38674,#38675,#38676,#38677,#38678,
#38679,#38680,#38681,#38682,#38683,#38684,#38685,#38686,#38687,#38688,#38689,
#38690,#38691,#38692,#38693,#38694,#38695,#38696,#38697,#38698,#38699,#38700,
#38701,#38702,#38703,#38704,#38705,#38706,#38707,#38708,#38709,#38710,#38711,
#38712,#38713,#38714,#38715,#38716,#38717,#38718,#38719,#38720,#38721,#38722,
#38723,#38724,#38725,#38726,#38727,#38728,#38729,#38730,#38731,#38732,#38733,
#38734,#38735,#38736,#38737,#38738,#38739,#38740,#38741,#38742,#38743,#38744,
#38745,#38746,#38747,#38748,#38749,#38750,#38751,#38752,#38753,#38754,#38755,
#38756,#38757,#38758,#38759,#38760,#38761,#38762,#38763,#38764,#38765,#38766,
#38767,#38768,#38769,#38770,#38771,#38772,#38773,#38774,#38775,#38776,#38777,
#38778,#38779,#38780,#38781,#38782,#38783,#38784,#38785,#38786,#38787,#38788,
#38789,#38790,#38791,#38792,#38793,#38794,#38795,#38796,#38797,#38798,#38799,
#38800,#38801)),.UNSPECIFIED.,.F.,.F.,.F.)
B_SPLINE_SURFACE_WITH_KNOTS((2,2),(3,2,2,2,2,2,2,2,2,2,2,2,2,2,2,2,2,2,
2,2,2,2,2,2,2,2,2,2,2,2,2,2,2,2,2,2,2,2,2,2,2,2,2,2,2,2,2,2,2,2,2,2,2,2,
2,2,2,2,2,2,2,2,2,2,2,2,2,2,2,2,2,2,2,2,2,2,2,2,2,2,2,2,2,2,2,2,2,2,2,2,
2,2,2,2,2,2,2,2,2,2,2,2,2,2,2,2,2,2,2,2,2,2,2,2,2,2,2,2,2,2,2,2,2,2,2,2,
2,2,2,2,2,2,2,2,2,2,2,2,2,2,2,2,2,2,2,2,2,2,2,2,2,2,2,2,2,2,2,2,2,2,2,2,
2,2,2,2,2,2,2,2,2,2,2,2,2,2,2,2,2,2,2,2,2,2,2,2,2,2,2,2,2,2,2,2,2,2,2,2,
2,2,2,2,2,2,2,2,2,2,2,2,2,2,2,2,2,2,2,2,2,2,2,2,2,2,2,2,2,2,2,2,2,2,2,2,
2,2,2,2,2,2,2,2,2,2,2,2,2,2,2,2,2,2,2,2,2,2,2,2,2,2,2,2,2,2,2,2,2,2,2,2,
2,2,2,2,2,2,2,2,2,2,2,2,2,2,2,2,2,2,2,2,2,2,2,2,2,2,2,2,2,2,2,2,2,2,2,2,
2,2,2,2,2,2,2,2,2,2,2,2,2,2,2,2,2,2,2,2,2,2,2,2,2,2,2,2,2,2,2,2,2,2,2,2,
2,2,2,2,2,2,3),(0.,1.),(0.,0.00284090909090909,0.00568181818181818,0.00852272727272727,
0.0113636363636364,0.0142045454545455,0.0170454545454545,0.0198863636363636,
0.0227272727272727,0.0255681818181818,0.0284090909090909,0.03125,0.0340909090909091,
0.0369318181818182,0.0397727272727273,0.0426136363636364,0.0454545454545455,
0.0482954545454545,0.0511363636363636,0.0539772727272727,0.0568181818181818,
0.0596590909090909,0.0625,0.0653409090909091,0.0681818181818182,0.0710227272727273,
0.0738636363636364,0.0767045454545455,0.0795454545454545,0.0823863636363636,
0.0852272727272727,0.0880681818181818,0.0909090909090909,0.09375,0.0965909090909091,
0.0994318181818182,0.102272727272727,0.105113636363636,0.107954545454545,
0.110795454545455,0.113636363636364,0.116477272727273,0.119318181818182,
0.122159090909091,0.125,0.127840909090909,0.130681818181818,0.133522727272727,
0.136363636363636,0.139204545454545,0.142045454545455,0.144886363636364,
0.147727272727273,0.150568181818182,0.153409090909091,0.15625,0.159090909090909,
0.161931818181818,0.164772727272727,0.167613636363636,0.170454545454545,
0.173295454545455,0.176136363636364,0.178977272727273,0.181818181818182,
0.184659090909091,0.1875,0.190340909090909,0.193181818181818,0.196022727272727,
0.198863636363636,0.201704545454545,0.204545454545455,0.207386363636364,
0.210227272727273,0.213068181818182,0.215909090909091,0.21875,0.221590909090909,
0.224431818181818,0.227272727272727,0.230113636363636,0.232954545454545,
0.235795454545455,0.238636363636364,0.241477272727273,0.244318181818182,
0.247159090909091,0.25,0.252840909090909,0.255681818181818,0.258522727272727,
0.261363636363636,0.264204545454545,0.267045454545455,0.269886363636364,
0.272727272727273,0.275568181818182,0.278409090909091,0.28125,0.284090909090909,
0.286931818181818,0.289772727272727,0.292613636363636,0.295454545454545,
0.298295454545455,0.301136363636364,0.303977272727273,0.306818181818182,
0.309659090909091,0.3125,0.315340909090909,0.318181818181818,0.321022727272727,
0.323863636363636,0.326704545454545,0.329545454545455,0.332386363636364,
0.335227272727273,0.338068181818182,0.340909090909091,0.34375,0.346590909090909,
0.349431818181818,0.352272727272727,0.355113636363636,0.357954545454545,
0.360795454545455,0.363636363636364,0.366477272727273,0.369318181818182,
0.372159090909091,0.375,0.377840909090909,0.380681818181818,0.383522727272727,
0.386363636363636,0.389204545454545,0.392045454545455,0.394886363636364,
0.397727272727273,0.400568181818182,0.403409090909091,0.40625,0.409090909090909,
0.411931818181818,0.414772727272727,0.417613636363636,0.420454545454545,
0.423295454545455,0.426136363636364,0.428977272727273,0.431818181818182,
0.434659090909091,0.4375,0.440340909090909,0.443181818181818,0.446022727272727,
0.448863636363636,0.451704545454545,0.454545454545455,0.457386363636364,
0.460227272727273,0.463068181818182,0.465909090909091,0.46875,0.471590909090909,
0.474431818181818,0.477272727272727,0.480113636363636,0.482954545454545,
0.485795454545455,0.488636363636364,0.491477272727273,0.494318181818182,
0.497159090909091,0.5,0.502840909090909,0.505681818181818,0.508522727272727,
0.511363636363636,0.514204545454545,0.517045454545455,0.519886363636364,
0.522727272727273,0.525568181818182,0.528409090909091,0.53125,0.534090909090909,
0.536931818181818,0.539772727272727,0.542613636363636,0.545454545454545,
0.548295454545455,0.551136363636364,0.553977272727273,0.556818181818182,
0.559659090909091,0.5625,0.565340909090909,0.568181818181818,0.571022727272727,
0.573863636363636,0.576704545454545,0.579545454545455,0.582386363636364,
0.585227272727273,0.588068181818182,0.590909090909091,0.59375,0.596590909090909,
0.599431818181818,0.602272727272727,0.605113636363636,0.607954545454545,
0.610795454545455,0.613636363636364,0.616477272727273,0.619318181818182,
0.622159090909091,0.625,0.627840909090909,0.630681818181818,0.633522727272727,
0.636363636363636,0.639204545454545,0.642045454545455,0.644886363636364,
0.647727272727273,0.650568181818182,0.653409090909091,0.65625,0.659090909090909,
0.661931818181818,0.664772727272727,0.667613636363636,0.670454545454545,
0.673295454545455,0.676136363636364,0.678977272727273,0.681818181818182,
0.684659090909091,0.6875,0.690340909090909,0.693181818181818,0.696022727272727,
0.698863636363636,0.701704545454545,0.704545454545455,0.707386363636364,
0.710227272727273,0.713068181818182,0.715909090909091,0.71875,0.721590909090909,
0.724431818181818,0.727272727272727,0.730113636363636,0.732954545454545,
0.735795454545455,0.738636363636364,0.741477272727273,0.744318181818182,
0.747159090909091,0.75,0.752840909090909,0.755681818181818,0.758522727272727,
0.761363636363636,0.764204545454545,0.767045454545455,0.769886363636364,
0.772727272727273,0.775568181818182,0.778409090909091,0.78125,0.784090909090909,
0.786931818181818,0.789772727272727,0.792613636363636,0.795454545454545,
0.798295454545455,0.801136363636364,0.803977272727273,0.806818181818182,
0.809659090909091,0.8125,0.815340909090909,0.818181818181818,0.821022727272727,
0.823863636363636,0.826704545454545,0.829545454545455,0.832386363636364,
0.835227272727273,0.838068181818182,0.840909090909091,0.84375,0.846590909090909,
0.849431818181818,0.852272727272727,0.855113636363636,0.857954545454545,
0.860795454545455,0.863636363636364,0.866477272727273,0.869318181818182,
0.872159090909091,0.875,0.877840909090909,0.880681818181818,0.883522727272727,
0.886363636363636,0.889204545454545,0.892045454545455,0.894886363636364,
0.897727272727273,0.900568181818182,0.903409090909091,0.90625,0.909090909090909,
0.911931818181818,0.914772727272727,0.917613636363636,0.920454545454545,
0.923295454545455,0.926136363636364,0.928977272727273,0.931818181818182,
0.934659090909091,0.9375,0.940340909090909,0.943181818181818,0.946022727272727,
0.948863636363636,0.951704545454545,0.954545454545455,0.957386363636364,
0.960227272727273,0.963068181818182,0.965909090909091,0.96875,0.971590909090909,
0.974431818181818,0.977272727272727,0.980113636363636,0.982954545454545,
0.984842983060018,0.994691412890618),.UNSPECIFIED.)
GEOMETRIC_REPRESENTATION_ITEM()
RATIONAL_B_SPLINE_SURFACE(((1.,0.923879532511287,1.,0.923879532511287,1.,
0.923879532511287,1.,0.923879532511287,1.,0.923879532511287,1.,0.923879532511287,
1.,0.923879532511287,1.,0.923879532511287,1.,0.923879532511287,1.,0.923879532511287,
1.,0.923879532511287,1.,0.923879532511287,1.,0.923879532511287,1.,0.923879532511287,
1.,0.923879532511287,1.,0.923879532511287,1.,0.923879532511287,1.,0.923879532511287,
1.,0.923879532511287,1.,0.923879532511287,1.,0.923879532511287,1.,0.923879532511287,
1.,0.923879532511287,1.,0.923879532511287,1.,0.923879532511287,1.,0.923879532511287,
1.,0.923879532511287,1.,0.923879532511287,1.,0.923879532511287,1.,0.923879532511287,
1.,0.923879532511287,1.,0.923879532511287,1.,0.923879532511287,1.,0.923879532511287,
1.,0.923879532511287,1.,0.923879532511287,1.,0.923879532511287,1.,0.923879532511287,
1.,0.923879532511287,1.,0.923879532511287,1.,0.923879532511287,1.,0.923879532511287,
1.,0.923879532511287,1.,0.923879532511287,1.,0.923879532511287,1.,0.923879532511287,
1.,0.923879532511287,1.,0.923879532511287,1.,0.923879532511287,1.,0.923879532511287,
1.,0.923879532511287,1.,0.923879532511287,1.,0.923879532511287,1.,0.923879532511287,
1.,0.923879532511287,1.,0.923879532511287,1.,0.923879532511287,1.,0.923879532511287,
1.,0.923879532511287,1.,0.923879532511287,1.,0.923879532511287,1.,0.923879532511287,
1.,0.923879532511287,1.,0.923879532511287,1.,0.923879532511287,1.,0.923879532511287,
1.,0.923879532511287,1.,0.923879532511287,1.,0.923879532511287,1.,0.923879532511287,
1.,0.923879532511287,1.,0.923879532511287,1.,0.923879532511287,1.,0.923879532511287,
1.,0.923879532511287,1.,0.923879532511287,1.,0.923879532511287,1.,0.923879532511287,
1.,0.923879532511287,1.,0.923879532511287,1.,0.923879532511287,1.,0.923879532511287,
1.,0.923879532511287,1.,0.923879532511287,1.,0.923879532511287,1.,0.923879532511287,
1.,0.923879532511287,1.,0.923879532511287,1.,0.923879532511287,1.,0.923879532511287,
1.,0.923879532511287,1.,0.923879532511287,1.,0.923879532511287,1.,0.923879532511287,
1.,0.923879532511287,1.,0.923879532511287,1.,0.923879532511287,1.,0.923879532511287,
1.,0.923879532511287,1.,0.923879532511287,1.,0.923879532511287,1.,0.923879532511287,
1.,0.923879532511287,1.,0.923879532511287,1.,0.923879532511287,1.,0.923879532511287,
1.,0.923879532511287,1.,0.923879532511287,1.,0.923879532511287,1.,0.923879532511287,
1.,0.923879532511287,1.,0.923879532511287,1.,0.923879532511287,1.,0.923879532511287,
1.,0.923879532511287,1.,0.923879532511287,1.,0.923879532511287,1.,0.923879532511287,
1.,0.923879532511287,1.,0.923879532511287,1.,0.923879532511287,1.,0.923879532511287,
1.,0.923879532511287,1.,0.923879532511287,1.,0.923879532511287,1.,0.923879532511287,
1.,0.923879532511287,1.,0.923879532511287,1.,0.923879532511287,1.,0.923879532511287,
1.,0.923879532511287,1.,0.923879532511287,1.,0.923879532511287,1.,0.923879532511287,
1.,0.923879532511287,1.,0.923879532511287,1.,0.923879532511287,1.,0.923879532511287,
1.,0.923879532511287,1.,0.923879532511287,1.,0.923879532511287,1.,0.923879532511287,
1.,0.923879532511287,1.,0.923879532511287,1.,0.923879532511287,1.,0.923879532511287,
1.,0.923879532511287,1.,0.923879532511287,1.,0.923879532511287,1.,0.923879532511287,
1.,0.923879532511287,1.,0.923879532511287,1.,0.923879532511287,1.,0.923879532511287,
1.,0.923879532511287,1.,0.923879532511287,1.,0.923879532511287,1.,0.923879532511287,
1.,0.923879532511287,1.,0.923879532511287,1.,0.923879532511287,1.,0.923879532511287,
1.,0.923879532511287,1.,0.923879532511287,1.,0.923879532511287,1.,0.923879532511287,
1.,0.923879532511287,1.,0.923879532511287,1.,0.923879532511287,1.,0.923879532511287,
1.,0.923879532511287,1.,0.923879532511287,1.,0.923879532511287,1.,0.923879532511287,
1.,0.923879532511287,1.,0.923879532511287,1.,0.923879532511287,1.,0.923879532511287,
1.,0.923879532511287,1.,0.923879532511287,1.,0.923879532511287,1.,0.923879532511287,
1.,0.923879532511287,1.,0.923879532511287,1.,0.923879532511287,1.,0.923879532511287,
1.,0.923879532511287,1.,0.923879532511287,1.,0.923879532511287,1.,0.923879532511287,
1.,0.923879532511287,1.,0.923879532511287,1.,0.923879532511287,1.,0.923879532511287,
1.,0.923879532511287,1.,0.923879532511287,1.,0.923879532511287,1.,0.923879532511287,
1.,0.923879532511287,1.,0.923879532511287,1.,0.923879532511287,1.,0.923879532511287,
1.,0.923879532511287,1.,0.923879532511287,1.,0.923879532511287,1.,0.923879532511287,
1.,0.923879532511287,1.,0.923879532511287,1.,0.923879532511287,1.,0.923879532511287,
1.,0.923879532511287,1.,0.923879532511287,1.,0.923879532511287,1.,0.923879532511287,
1.,0.923879532511287,1.,0.923879532511287,1.,0.923879532511287,1.,0.923879532511287,
1.,0.923879532511287,1.,0.923879532511287,1.,0.923879532511287,1.,0.923879532511287,
1.,0.923879532511287,1.,0.923879532511287,1.,0.923879532511287,1.,0.923879532511287,
1.,0.923879532511287,1.,0.923879532511287,1.,0.923879532511287,1.,0.923879532511287,
1.,0.923879532511287,1.,0.923879532511287,1.,0.923879532511287,1.,0.923879532511287,
1.,0.923879532511287,1.,0.923879532511287,1.,0.923879532511287,1.,0.923879532511287,
1.,0.923879532511287,1.,0.923879532511287,1.,0.923879532511287,1.,0.923879532511287,
1.,0.923879532511287,1.,0.923879532511287,1.,0.923879532511287,1.,0.923879532511287,
1.,0.923879532511287,1.,0.923879532511287,1.,0.923879532511287,1.,0.923879532511287,
1.,0.923879532511287,1.,0.923879532511287,1.,0.923879532511287,1.,0.923879532511287,
1.,0.923879532511287,1.,0.923879532511287,1.,0.923879532511287,1.,0.923879532511287,
1.,0.923879532511287,1.,0.923879532511287,1.,0.923879532511287,1.,0.923879532511287,
1.,0.923879532511287,1.,0.923879532511287,1.,0.923879532511287,1.,0.923879532511287,
1.,0.923879532511287,1.,0.923879532511287,1.,0.923879532511287,1.,0.923879532511287,
1.,0.923879532511287,1.,0.923879532511287,1.,0.923879532511287,1.,0.923879532511287,
1.,0.923879532511287,1.,0.923879532511287,1.,0.923879532511287,1.,0.923879532511287,
1.,0.923879532511287,1.,0.923879532511287,1.,0.923879532511287,1.,0.923879532511287,
1.,0.923879532511287,1.,0.923879532511287,1.,0.923879532511287,1.,0.923879532511287,
1.,0.923879532511287,1.,0.923879532511287,1.,0.923879532511287,1.,0.923879532511287,
1.,0.923879532511287,1.,0.923879532511287,1.,0.923879532511287,1.,0.923879532511287,
1.,0.923879532511287,1.,0.923879532511287,1.,0.923879532511287,1.,0.923879532511287,
1.,0.923879532511287,1.,0.923879532511287,1.,0.923879532511287,1.,0.923879532511287,
1.,0.923879532511287,1.,0.923879532511287,1.,0.923879532511287,1.,0.923879532511287,
1.,0.923879532511287,1.,0.923879532511287,1.,0.923879532511287,1.,0.923879532511287,
1.,0.923879532511287,1.,0.923879532511287,1.,0.923879532511287,1.,0.923879532511287,
1.,0.923879532511287,1.,0.923879532511287,1.,0.923879532511287,1.,0.923879532511287,
1.,0.923879532511287,1.,0.923879532511287,1.,0.923879532511287,1.,0.923879532511287,
1.,0.923879532511287,1.,0.923879532511287,1.,0.923879532511287,1.,0.923879532511287,
1.,0.923879532511287,1.,0.923879532511287,1.,0.923879532511287,1.,0.923879532511287,
1.,0.923879532511287,1.,0.923879532511287,1.,0.923879532511287,1.,0.923879532511287,
1.,0.923879532511287,1.,0.923879532511287,1.,0.923879532511287,1.,0.923879532511287,
1.,0.923879532511287,1.,0.923879532511287,1.,0.923879532511287,1.,0.923879532511287,
1.,0.923879532511287,1.,0.923879532511287,1.,0.923879532511287,1.,0.923879532511287,
1.,0.949400438820153,0.966070974003619,0.966070974003619,0.966070974003619),
(1.,0.923879532511287,1.,0.923879532511287,1.,0.923879532511287,1.,0.923879532511287,
1.,0.923879532511287,1.,0.923879532511287,1.,0.923879532511287,1.,0.923879532511287,
1.,0.923879532511287,1.,0.923879532511287,1.,0.923879532511287,1.,0.923879532511287,
1.,0.923879532511287,1.,0.923879532511287,1.,0.923879532511287,1.,0.923879532511287,
1.,0.923879532511287,1.,0.923879532511287,1.,0.923879532511287,1.,0.923879532511287,
1.,0.923879532511287,1.,0.923879532511287,1.,0.923879532511287,1.,0.923879532511287,
1.,0.923879532511287,1.,0.923879532511287,1.,0.923879532511287,1.,0.923879532511287,
1.,0.923879532511287,1.,0.923879532511287,1.,0.923879532511287,1.,0.923879532511287,
1.,0.923879532511287,1.,0.923879532511287,1.,0.923879532511287,1.,0.923879532511287,
1.,0.923879532511287,1.,0.923879532511287,1.,0.923879532511287,1.,0.923879532511287,
1.,0.923879532511287,1.,0.923879532511287,1.,0.923879532511287,1.,0.923879532511287,
1.,0.923879532511287,1.,0.923879532511287,1.,0.923879532511287,1.,0.923879532511287,
1.,0.923879532511287,1.,0.923879532511287,1.,0.923879532511287,1.,0.923879532511287,
1.,0.923879532511287,1.,0.923879532511287,1.,0.923879532511287,1.,0.923879532511287,
1.,0.923879532511287,1.,0.923879532511287,1.,0.923879532511287,1.,0.923879532511287,
1.,0.923879532511287,1.,0.923879532511287,1.,0.923879532511287,1.,0.923879532511287,
1.,0.923879532511287,1.,0.923879532511287,1.,0.923879532511287,1.,0.923879532511287,
1.,0.923879532511287,1.,0.923879532511287,1.,0.923879532511287,1.,0.923879532511287,
1.,0.923879532511287,1.,0.923879532511287,1.,0.923879532511287,1.,0.923879532511287,
1.,0.923879532511287,1.,0.923879532511287,1.,0.923879532511287,1.,0.923879532511287,
1.,0.923879532511287,1.,0.923879532511287,1.,0.923879532511287,1.,0.923879532511287,
1.,0.923879532511287,1.,0.923879532511287,1.,0.923879532511287,1.,0.923879532511287,
1.,0.923879532511287,1.,0.923879532511287,1.,0.923879532511287,1.,0.923879532511287,
1.,0.923879532511287,1.,0.923879532511287,1.,0.923879532511287,1.,0.923879532511287,
1.,0.923879532511287,1.,0.923879532511287,1.,0.923879532511287,1.,0.923879532511287,
1.,0.923879532511287,1.,0.923879532511287,1.,0.923879532511287,1.,0.923879532511287,
1.,0.923879532511287,1.,0.923879532511287,1.,0.923879532511287,1.,0.923879532511287,
1.,0.923879532511287,1.,0.923879532511287,1.,0.923879532511287,1.,0.923879532511287,
1.,0.923879532511287,1.,0.923879532511287,1.,0.923879532511287,1.,0.923879532511287,
1.,0.923879532511287,1.,0.923879532511287,1.,0.923879532511287,1.,0.923879532511287,
1.,0.923879532511287,1.,0.923879532511287,1.,0.923879532511287,1.,0.923879532511287,
1.,0.923879532511287,1.,0.923879532511287,1.,0.923879532511287,1.,0.923879532511287,
1.,0.923879532511287,1.,0.923879532511287,1.,0.923879532511287,1.,0.923879532511287,
1.,0.923879532511287,1.,0.923879532511287,1.,0.923879532511287,1.,0.923879532511287,
1.,0.923879532511287,1.,0.923879532511287,1.,0.923879532511287,1.,0.923879532511287,
1.,0.923879532511287,1.,0.923879532511287,1.,0.923879532511287,1.,0.923879532511287,
1.,0.923879532511287,1.,0.923879532511287,1.,0.923879532511287,1.,0.923879532511287,
1.,0.923879532511287,1.,0.923879532511287,1.,0.923879532511287,1.,0.923879532511287,
1.,0.923879532511287,1.,0.923879532511287,1.,0.923879532511287,1.,0.923879532511287,
1.,0.923879532511287,1.,0.923879532511287,1.,0.923879532511287,1.,0.923879532511287,
1.,0.923879532511287,1.,0.923879532511287,1.,0.923879532511287,1.,0.923879532511287,
1.,0.923879532511287,1.,0.923879532511287,1.,0.923879532511287,1.,0.923879532511287,
1.,0.923879532511287,1.,0.923879532511287,1.,0.923879532511287,1.,0.923879532511287,
1.,0.923879532511287,1.,0.923879532511287,1.,0.923879532511287,1.,0.923879532511287,
1.,0.923879532511287,1.,0.923879532511287,1.,0.923879532511287,1.,0.923879532511287,
1.,0.923879532511287,1.,0.923879532511287,1.,0.923879532511287,1.,0.923879532511287,
1.,0.923879532511287,1.,0.923879532511287,1.,0.923879532511287,1.,0.923879532511287,
1.,0.923879532511287,1.,0.923879532511287,1.,0.923879532511287,1.,0.923879532511287,
1.,0.923879532511287,1.,0.923879532511287,1.,0.923879532511287,1.,0.923879532511287,
1.,0.923879532511287,1.,0.923879532511287,1.,0.923879532511287,1.,0.923879532511287,
1.,0.923879532511287,1.,0.923879532511287,1.,0.923879532511287,1.,0.923879532511287,
1.,0.923879532511287,1.,0.923879532511287,1.,0.923879532511287,1.,0.923879532511287,
1.,0.923879532511287,1.,0.923879532511287,1.,0.923879532511287,1.,0.923879532511287,
1.,0.923879532511287,1.,0.923879532511287,1.,0.923879532511287,1.,0.923879532511287,
1.,0.923879532511287,1.,0.923879532511287,1.,0.923879532511287,1.,0.923879532511287,
1.,0.923879532511287,1.,0.923879532511287,1.,0.923879532511287,1.,0.923879532511287,
1.,0.923879532511287,1.,0.923879532511287,1.,0.923879532511287,1.,0.923879532511287,
1.,0.923879532511287,1.,0.923879532511287,1.,0.923879532511287,1.,0.923879532511287,
1.,0.923879532511287,1.,0.923879532511287,1.,0.923879532511287,1.,0.923879532511287,
1.,0.923879532511287,1.,0.923879532511287,1.,0.923879532511287,1.,0.923879532511287,
1.,0.923879532511287,1.,0.923879532511287,1.,0.923879532511287,1.,0.923879532511287,
1.,0.923879532511287,1.,0.923879532511287,1.,0.923879532511287,1.,0.923879532511287,
1.,0.923879532511287,1.,0.923879532511287,1.,0.923879532511287,1.,0.923879532511287,
1.,0.923879532511287,1.,0.923879532511287,1.,0.923879532511287,1.,0.923879532511287,
1.,0.923879532511287,1.,0.923879532511287,1.,0.923879532511287,1.,0.923879532511287,
1.,0.923879532511287,1.,0.923879532511287,1.,0.923879532511287,1.,0.923879532511287,
1.,0.923879532511287,1.,0.923879532511287,1.,0.923879532511287,1.,0.923879532511287,
1.,0.923879532511287,1.,0.923879532511287,1.,0.923879532511287,1.,0.923879532511287,
1.,0.923879532511287,1.,0.923879532511287,1.,0.923879532511287,1.,0.923879532511287,
1.,0.923879532511287,1.,0.923879532511287,1.,0.923879532511287,1.,0.923879532511287,
1.,0.923879532511287,1.,0.923879532511287,1.,0.923879532511287,1.,0.923879532511287,
1.,0.923879532511287,1.,0.923879532511287,1.,0.923879532511287,1.,0.923879532511287,
1.,0.923879532511287,1.,0.923879532511287,1.,0.923879532511287,1.,0.923879532511287,
1.,0.923879532511287,1.,0.923879532511287,1.,0.923879532511287,1.,0.923879532511287,
1.,0.923879532511287,1.,0.923879532511287,1.,0.923879532511287,1.,0.923879532511287,
1.,0.923879532511287,1.,0.923879532511287,1.,0.923879532511287,1.,0.923879532511287,
1.,0.923879532511287,1.,0.923879532511287,1.,0.923879532511287,1.,0.923879532511287,
1.,0.923879532511287,1.,0.923879532511287,1.,0.923879532511287,1.,0.923879532511287,
1.,0.923879532511287,1.,0.923879532511287,1.,0.923879532511287,1.,0.923879532511287,
1.,0.923879532511287,1.,0.923879532511287,1.,0.923879532511287,1.,0.923879532511287,
1.,0.923879532511287,1.,0.923879532511287,1.,0.923879532511287,1.,0.923879532511287,
1.,0.923879532511287,1.,0.923879532511287,1.,0.923879532511287,1.,0.923879532511287,
1.,0.923879532511287,1.,0.923879532511287,1.,0.923879532511287,1.,0.923879532511287,
1.,0.923879532511287,1.,0.923879532511287,1.,0.923879532511287,1.,0.923879532511287,
1.,0.923879532511287,1.,0.923879532511287,1.,0.923879532511287,1.,0.923879532511287,
1.,0.923879532511287,1.,0.923879532511287,1.,0.923879532511287,1.,0.923879532511287,
1.,0.923879532511287,1.,0.923879532511287,1.,0.949400438820153,0.966070974003619,
0.966070974003619,0.966070974003619)))
REPRESENTATION_ITEM('')
SURFACE()
);
#588=(
BOUNDED_SURFACE()
B_SPLINE_SURFACE(1,2,((#39445,#39446,#39447,#39448,#39449,#39450,#39451,
#39452,#39453,#39454,#39455,#39456,#39457,#39458,#39459,#39460,#39461,#39462,
#39463,#39464,#39465,#39466,#39467,#39468,#39469,#39470,#39471,#39472,#39473,
#39474,#39475,#39476,#39477,#39478,#39479,#39480,#39481,#39482,#39483,#39484,
#39485,#39486,#39487,#39488,#39489,#39490,#39491,#39492,#39493,#39494,#39495,
#39496,#39497,#39498,#39499,#39500,#39501,#39502,#39503,#39504,#39505,#39506,
#39507,#39508,#39509,#39510,#39511,#39512,#39513,#39514,#39515,#39516,#39517,
#39518,#39519,#39520,#39521,#39522,#39523,#39524,#39525,#39526,#39527,#39528,
#39529,#39530,#39531,#39532,#39533,#39534,#39535,#39536,#39537,#39538,#39539,
#39540,#39541,#39542,#39543,#39544,#39545,#39546,#39547,#39548,#39549,#39550,
#39551,#39552,#39553,#39554,#39555,#39556,#39557,#39558,#39559,#39560,#39561,
#39562,#39563,#39564,#39565,#39566,#39567,#39568,#39569,#39570,#39571,#39572,
#39573,#39574,#39575,#39576,#39577,#39578,#39579,#39580,#39581,#39582,#39583,
#39584,#39585,#39586,#39587,#39588,#39589,#39590,#39591,#39592,#39593,#39594,
#39595,#39596,#39597,#39598,#39599,#39600,#39601,#39602,#39603,#39604,#39605,
#39606,#39607,#39608,#39609,#39610,#39611,#39612,#39613,#39614,#39615,#39616,
#39617,#39618,#39619,#39620,#39621,#39622,#39623,#39624,#39625,#39626,#39627,
#39628,#39629,#39630,#39631,#39632,#39633,#39634,#39635,#39636,#39637,#39638,
#39639,#39640,#39641,#39642,#39643,#39644,#39645,#39646,#39647,#39648,#39649,
#39650,#39651,#39652,#39653,#39654,#39655,#39656,#39657,#39658,#39659,#39660,
#39661,#39662,#39663,#39664,#39665,#39666,#39667,#39668,#39669,#39670,#39671,
#39672,#39673,#39674,#39675,#39676,#39677,#39678,#39679,#39680,#39681,#39682,
#39683,#39684,#39685,#39686,#39687,#39688,#39689,#39690,#39691,#39692,#39693,
#39694,#39695,#39696,#39697,#39698,#39699,#39700,#39701,#39702,#39703,#39704,
#39705,#39706,#39707,#39708,#39709,#39710,#39711,#39712,#39713,#39714,#39715,
#39716,#39717,#39718,#39719,#39720,#39721,#39722,#39723,#39724,#39725,#39726,
#39727,#39728,#39729,#39730,#39731,#39732,#39733,#39734,#39735,#39736,#39737,
#39738,#39739,#39740,#39741,#39742,#39743,#39744,#39745,#39746,#39747,#39748,
#39749,#39750,#39751,#39752,#39753,#39754,#39755,#39756,#39757,#39758,#39759,
#39760,#39761,#39762,#39763,#39764,#39765,#39766,#39767,#39768,#39769,#39770,
#39771,#39772,#39773,#39774,#39775,#39776,#39777,#39778,#39779,#39780,#39781,
#39782,#39783,#39784,#39785,#39786,#39787,#39788,#39789,#39790,#39791,#39792,
#39793,#39794,#39795,#39796,#39797,#39798,#39799,#39800,#39801,#39802,#39803,
#39804,#39805,#39806,#39807,#39808,#39809,#39810,#39811,#39812,#39813,#39814,
#39815,#39816,#39817,#39818,#39819,#39820,#39821,#39822,#39823,#39824,#39825,
#39826,#39827,#39828,#39829,#39830,#39831,#39832,#39833,#39834,#39835,#39836,
#39837,#39838,#39839,#39840,#39841,#39842,#39843,#39844,#39845,#39846,#39847,
#39848,#39849,#39850,#39851,#39852,#39853,#39854,#39855,#39856,#39857,#39858,
#39859,#39860,#39861,#39862,#39863,#39864,#39865,#39866,#39867,#39868,#39869,
#39870,#39871,#39872,#39873,#39874,#39875,#39876,#39877,#39878,#39879,#39880,
#39881,#39882,#39883,#39884,#39885,#39886,#39887,#39888,#39889,#39890,#39891,
#39892,#39893,#39894,#39895,#39896,#39897,#39898,#39899,#39900,#39901,#39902,
#39903,#39904,#39905,#39906,#39907,#39908,#39909,#39910,#39911,#39912,#39913,
#39914,#39915,#39916,#39917,#39918,#39919,#39920,#39921,#39922,#39923,#39924,
#39925,#39926,#39927,#39928,#39929,#39930,#39931,#39932,#39933,#39934,#39935,
#39936,#39937,#39938,#39939,#39940,#39941,#39942,#39943,#39944,#39945,#39946,
#39947,#39948,#39949,#39950,#39951,#39952,#39953,#39954,#39955,#39956,#39957,
#39958,#39959,#39960,#39961,#39962,#39963,#39964,#39965,#39966,#39967,#39968,
#39969,#39970,#39971,#39972,#39973,#39974,#39975,#39976,#39977,#39978,#39979,
#39980,#39981,#39982,#39983,#39984,#39985,#39986,#39987,#39988,#39989,#39990,
#39991,#39992,#39993,#39994,#39995,#39996,#39997,#39998,#39999,#40000,#40001,
#40002,#40003,#40004,#40005,#40006,#40007,#40008,#40009,#40010,#40011,#40012,
#40013,#40014,#40015,#40016,#40017,#40018,#40019,#40020,#40021,#40022,#40023,
#40024,#40025,#40026,#40027,#40028,#40029,#40030,#40031,#40032,#40033,#40034,
#40035,#40036,#40037,#40038,#40039,#40040,#40041,#40042,#40043,#40044,#40045,
#40046,#40047,#40048,#40049,#40050,#40051,#40052,#40053,#40054,#40055,#40056,
#40057,#40058,#40059,#40060,#40061,#40062,#40063,#40064,#40065,#40066,#40067,
#40068,#40069,#40070,#40071,#40072,#40073,#40074,#40075,#40076,#40077,#40078,
#40079,#40080,#40081,#40082,#40083,#40084,#40085,#40086,#40087,#40088,#40089,
#40090,#40091,#40092,#40093,#40094,#40095,#40096,#40097,#40098,#40099,#40100,
#40101,#40102,#40103,#40104,#40105,#40106,#40107,#40108,#40109,#40110,#40111,
#40112,#40113,#40114,#40115,#40116,#40117,#40118,#40119,#40120,#40121,#40122,
#40123,#40124,#40125,#40126,#40127,#40128,#40129,#40130,#40131,#40132,#40133,
#40134,#40135,#40136,#40137,#40138,#40139),(#40140,#40141,#40142,#40143,
#40144,#40145,#40146,#40147,#40148,#40149,#40150,#40151,#40152,#40153,#40154,
#40155,#40156,#40157,#40158,#40159,#40160,#40161,#40162,#40163,#40164,#40165,
#40166,#40167,#40168,#40169,#40170,#40171,#40172,#40173,#40174,#40175,#40176,
#40177,#40178,#40179,#40180,#40181,#40182,#40183,#40184,#40185,#40186,#40187,
#40188,#40189,#40190,#40191,#40192,#40193,#40194,#40195,#40196,#40197,#40198,
#40199,#40200,#40201,#40202,#40203,#40204,#40205,#40206,#40207,#40208,#40209,
#40210,#40211,#40212,#40213,#40214,#40215,#40216,#40217,#40218,#40219,#40220,
#40221,#40222,#40223,#40224,#40225,#40226,#40227,#40228,#40229,#40230,#40231,
#40232,#40233,#40234,#40235,#40236,#40237,#40238,#40239,#40240,#40241,#40242,
#40243,#40244,#40245,#40246,#40247,#40248,#40249,#40250,#40251,#40252,#40253,
#40254,#40255,#40256,#40257,#40258,#40259,#40260,#40261,#40262,#40263,#40264,
#40265,#40266,#40267,#40268,#40269,#40270,#40271,#40272,#40273,#40274,#40275,
#40276,#40277,#40278,#40279,#40280,#40281,#40282,#40283,#40284,#40285,#40286,
#40287,#40288,#40289,#40290,#40291,#40292,#40293,#40294,#40295,#40296,#40297,
#40298,#40299,#40300,#40301,#40302,#40303,#40304,#40305,#40306,#40307,#40308,
#40309,#40310,#40311,#40312,#40313,#40314,#40315,#40316,#40317,#40318,#40319,
#40320,#40321,#40322,#40323,#40324,#40325,#40326,#40327,#40328,#40329,#40330,
#40331,#40332,#40333,#40334,#40335,#40336,#40337,#40338,#40339,#40340,#40341,
#40342,#40343,#40344,#40345,#40346,#40347,#40348,#40349,#40350,#40351,#40352,
#40353,#40354,#40355,#40356,#40357,#40358,#40359,#40360,#40361,#40362,#40363,
#40364,#40365,#40366,#40367,#40368,#40369,#40370,#40371,#40372,#40373,#40374,
#40375,#40376,#40377,#40378,#40379,#40380,#40381,#40382,#40383,#40384,#40385,
#40386,#40387,#40388,#40389,#40390,#40391,#40392,#40393,#40394,#40395,#40396,
#40397,#40398,#40399,#40400,#40401,#40402,#40403,#40404,#40405,#40406,#40407,
#40408,#40409,#40410,#40411,#40412,#40413,#40414,#40415,#40416,#40417,#40418,
#40419,#40420,#40421,#40422,#40423,#40424,#40425,#40426,#40427,#40428,#40429,
#40430,#40431,#40432,#40433,#40434,#40435,#40436,#40437,#40438,#40439,#40440,
#40441,#40442,#40443,#40444,#40445,#40446,#40447,#40448,#40449,#40450,#40451,
#40452,#40453,#40454,#40455,#40456,#40457,#40458,#40459,#40460,#40461,#40462,
#40463,#40464,#40465,#40466,#40467,#40468,#40469,#40470,#40471,#40472,#40473,
#40474,#40475,#40476,#40477,#40478,#40479,#40480,#40481,#40482,#40483,#40484,
#40485,#40486,#40487,#40488,#40489,#40490,#40491,#40492,#40493,#40494,#40495,
#40496,#40497,#40498,#40499,#40500,#40501,#40502,#40503,#40504,#40505,#40506,
#40507,#40508,#40509,#40510,#40511,#40512,#40513,#40514,#40515,#40516,#40517,
#40518,#40519,#40520,#40521,#40522,#40523,#40524,#40525,#40526,#40527,#40528,
#40529,#40530,#40531,#40532,#40533,#40534,#40535,#40536,#40537,#40538,#40539,
#40540,#40541,#40542,#40543,#40544,#40545,#40546,#40547,#40548,#40549,#40550,
#40551,#40552,#40553,#40554,#40555,#40556,#40557,#40558,#40559,#40560,#40561,
#40562,#40563,#40564,#40565,#40566,#40567,#40568,#40569,#40570,#40571,#40572,
#40573,#40574,#40575,#40576,#40577,#40578,#40579,#40580,#40581,#40582,#40583,
#40584,#40585,#40586,#40587,#40588,#40589,#40590,#40591,#40592,#40593,#40594,
#40595,#40596,#40597,#40598,#40599,#40600,#40601,#40602,#40603,#40604,#40605,
#40606,#40607,#40608,#40609,#40610,#40611,#40612,#40613,#40614,#40615,#40616,
#40617,#40618,#40619,#40620,#40621,#40622,#40623,#40624,#40625,#40626,#40627,
#40628,#40629,#40630,#40631,#40632,#40633,#40634,#40635,#40636,#40637,#40638,
#40639,#40640,#40641,#40642,#40643,#40644,#40645,#40646,#40647,#40648,#40649,
#40650,#40651,#40652,#40653,#40654,#40655,#40656,#40657,#40658,#40659,#40660,
#40661,#40662,#40663,#40664,#40665,#40666,#40667,#40668,#40669,#40670,#40671,
#40672,#40673,#40674,#40675,#40676,#40677,#40678,#40679,#40680,#40681,#40682,
#40683,#40684,#40685,#40686,#40687,#40688,#40689,#40690,#40691,#40692,#40693,
#40694,#40695,#40696,#40697,#40698,#40699,#40700,#40701,#40702,#40703,#40704,
#40705,#40706,#40707,#40708,#40709,#40710,#40711,#40712,#40713,#40714,#40715,
#40716,#40717,#40718,#40719,#40720,#40721,#40722,#40723,#40724,#40725,#40726,
#40727,#40728,#40729,#40730,#40731,#40732,#40733,#40734,#40735,#40736,#40737,
#40738,#40739,#40740,#40741,#40742,#40743,#40744,#40745,#40746,#40747,#40748,
#40749,#40750,#40751,#40752,#40753,#40754,#40755,#40756,#40757,#40758,#40759,
#40760,#40761,#40762,#40763,#40764,#40765,#40766,#40767,#40768,#40769,#40770,
#40771,#40772,#40773,#40774,#40775,#40776,#40777,#40778,#40779,#40780,#40781,
#40782,#40783,#40784,#40785,#40786,#40787,#40788,#40789,#40790,#40791,#40792,
#40793,#40794,#40795,#40796,#40797,#40798,#40799,#40800,#40801,#40802,#40803,
#40804,#40805,#40806,#40807,#40808,#40809,#40810,#40811,#40812,#40813,#40814,
#40815,#40816,#40817,#40818,#40819,#40820,#40821,#40822,#40823,#40824,#40825,
#40826,#40827,#40828,#40829,#40830,#40831,#40832,#40833,#40834)),
 .UNSPECIFIED.,.F.,.F.,.F.)
B_SPLINE_SURFACE_WITH_KNOTS((2,2),(3,2,2,2,2,2,2,2,2,2,2,2,2,2,2,2,2,2,
2,2,2,2,2,2,2,2,2,2,2,2,2,2,2,2,2,2,2,2,2,2,2,2,2,2,2,2,2,2,2,2,2,2,2,2,
2,2,2,2,2,2,2,2,2,2,2,2,2,2,2,2,2,2,2,2,2,2,2,2,2,2,2,2,2,2,2,2,2,2,2,2,
2,2,2,2,2,2,2,2,2,2,2,2,2,2,2,2,2,2,2,2,2,2,2,2,2,2,2,2,2,2,2,2,2,2,2,2,
2,2,2,2,2,2,2,2,2,2,2,2,2,2,2,2,2,2,2,2,2,2,2,2,2,2,2,2,2,2,2,2,2,2,2,2,
2,2,2,2,2,2,2,2,2,2,2,2,2,2,2,2,2,2,2,2,2,2,2,2,2,2,2,2,2,2,2,2,2,2,2,2,
2,2,2,2,2,2,2,2,2,2,2,2,2,2,2,2,2,2,2,2,2,2,2,2,2,2,2,2,2,2,2,2,2,2,2,2,
2,2,2,2,2,2,2,2,2,2,2,2,2,2,2,2,2,2,2,2,2,2,2,2,2,2,2,2,2,2,2,2,2,2,2,2,
2,2,2,2,2,2,2,2,2,2,2,2,2,2,2,2,2,2,2,2,2,2,2,2,2,2,2,2,2,2,2,2,2,2,2,2,
2,2,2,2,2,2,2,2,2,2,2,2,2,2,2,2,2,2,2,2,2,2,2,2,2,2,2,2,2,2,2,2,2,2,2,2,
2,2,2,2,2,3),(-3.10535428298811E-6,1.00000310535428),(0.,0.00284090909090909,
0.00568181818181818,0.00852272727272727,0.0113636363636364,0.0142045454545455,
0.0170454545454545,0.0198863636363636,0.0227272727272727,0.0255681818181818,
0.0284090909090909,0.03125,0.0340909090909091,0.0369318181818182,0.0397727272727273,
0.0426136363636364,0.0454545454545455,0.0482954545454545,0.0511363636363636,
0.0539772727272727,0.0568181818181818,0.0596590909090909,0.0625,0.0653409090909091,
0.0681818181818182,0.0710227272727273,0.0738636363636364,0.0767045454545455,
0.0795454545454545,0.0823863636363636,0.0852272727272727,0.0880681818181818,
0.0909090909090909,0.09375,0.0965909090909091,0.0994318181818182,0.102272727272727,
0.105113636363636,0.107954545454545,0.110795454545455,0.113636363636364,
0.116477272727273,0.119318181818182,0.122159090909091,0.125,0.127840909090909,
0.130681818181818,0.133522727272727,0.136363636363636,0.139204545454545,
0.142045454545455,0.144886363636364,0.147727272727273,0.150568181818182,
0.153409090909091,0.15625,0.159090909090909,0.161931818181818,0.164772727272727,
0.167613636363636,0.170454545454545,0.173295454545455,0.176136363636364,
0.178977272727273,0.181818181818182,0.184659090909091,0.1875,0.190340909090909,
0.193181818181818,0.196022727272727,0.198863636363636,0.201704545454545,
0.204545454545455,0.207386363636364,0.210227272727273,0.213068181818182,
0.215909090909091,0.21875,0.221590909090909,0.224431818181818,0.227272727272727,
0.230113636363636,0.232954545454545,0.235795454545455,0.238636363636364,
0.241477272727273,0.244318181818182,0.247159090909091,0.25,0.252840909090909,
0.255681818181818,0.258522727272727,0.261363636363636,0.264204545454545,
0.267045454545455,0.269886363636364,0.272727272727273,0.275568181818182,
0.278409090909091,0.28125,0.284090909090909,0.286931818181818,0.289772727272727,
0.292613636363636,0.295454545454545,0.298295454545455,0.301136363636364,
0.303977272727273,0.306818181818182,0.309659090909091,0.3125,0.315340909090909,
0.318181818181818,0.321022727272727,0.323863636363636,0.326704545454545,
0.329545454545455,0.332386363636364,0.335227272727273,0.338068181818182,
0.340909090909091,0.34375,0.346590909090909,0.349431818181818,0.352272727272727,
0.355113636363636,0.357954545454545,0.360795454545455,0.363636363636364,
0.366477272727273,0.369318181818182,0.372159090909091,0.375,0.377840909090909,
0.380681818181818,0.383522727272727,0.386363636363636,0.389204545454545,
0.392045454545455,0.394886363636364,0.397727272727273,0.400568181818182,
0.403409090909091,0.40625,0.409090909090909,0.411931818181818,0.414772727272727,
0.417613636363636,0.420454545454545,0.423295454545455,0.426136363636364,
0.428977272727273,0.431818181818182,0.434659090909091,0.4375,0.440340909090909,
0.443181818181818,0.446022727272727,0.448863636363636,0.451704545454545,
0.454545454545455,0.457386363636364,0.460227272727273,0.463068181818182,
0.465909090909091,0.46875,0.471590909090909,0.474431818181818,0.477272727272727,
0.480113636363636,0.482954545454545,0.485795454545455,0.488636363636364,
0.491477272727273,0.494318181818182,0.497159090909091,0.5,0.502840909090909,
0.505681818181818,0.508522727272727,0.511363636363636,0.514204545454545,
0.517045454545455,0.519886363636364,0.522727272727273,0.525568181818182,
0.528409090909091,0.53125,0.534090909090909,0.536931818181818,0.539772727272727,
0.542613636363636,0.545454545454545,0.548295454545455,0.551136363636364,
0.553977272727273,0.556818181818182,0.559659090909091,0.5625,0.565340909090909,
0.568181818181818,0.571022727272727,0.573863636363636,0.576704545454545,
0.579545454545455,0.582386363636364,0.585227272727273,0.588068181818182,
0.590909090909091,0.59375,0.596590909090909,0.599431818181818,0.602272727272727,
0.605113636363636,0.607954545454545,0.610795454545455,0.613636363636364,
0.616477272727273,0.619318181818182,0.622159090909091,0.625,0.627840909090909,
0.630681818181818,0.633522727272727,0.636363636363636,0.639204545454545,
0.642045454545455,0.644886363636364,0.647727272727273,0.650568181818182,
0.653409090909091,0.65625,0.659090909090909,0.661931818181818,0.664772727272727,
0.667613636363636,0.670454545454545,0.673295454545455,0.676136363636364,
0.678977272727273,0.681818181818182,0.684659090909091,0.6875,0.690340909090909,
0.693181818181818,0.696022727272727,0.698863636363636,0.701704545454545,
0.704545454545455,0.707386363636364,0.710227272727273,0.713068181818182,
0.715909090909091,0.71875,0.721590909090909,0.724431818181818,0.727272727272727,
0.730113636363636,0.732954545454545,0.735795454545455,0.738636363636364,
0.741477272727273,0.744318181818182,0.747159090909091,0.75,0.752840909090909,
0.755681818181818,0.758522727272727,0.761363636363636,0.764204545454545,
0.767045454545455,0.769886363636364,0.772727272727273,0.775568181818182,
0.778409090909091,0.78125,0.784090909090909,0.786931818181818,0.789772727272727,
0.792613636363636,0.795454545454545,0.798295454545455,0.801136363636364,
0.803977272727273,0.806818181818182,0.809659090909091,0.8125,0.815340909090909,
0.818181818181818,0.821022727272727,0.823863636363636,0.826704545454545,
0.829545454545455,0.832386363636364,0.835227272727273,0.838068181818182,
0.840909090909091,0.84375,0.846590909090909,0.849431818181818,0.852272727272727,
0.855113636363636,0.857954545454545,0.860795454545455,0.863636363636364,
0.866477272727273,0.869318181818182,0.872159090909091,0.875,0.877840909090909,
0.880681818181818,0.883522727272727,0.886363636363636,0.889204545454545,
0.892045454545455,0.894886363636364,0.897727272727273,0.900568181818182,
0.903409090909091,0.90625,0.909090909090909,0.911931818181818,0.914772727272727,
0.917613636363636,0.920454545454545,0.923295454545455,0.926136363636364,
0.928977272727273,0.931818181818182,0.934659090909091,0.9375,0.940340909090909,
0.943181818181818,0.946022727272727,0.948863636363636,0.951704545454545,
0.954545454545455,0.957386363636364,0.960227272727273,0.963068181818182,
0.965909090909091,0.96875,0.971590909090909,0.974431818181818,0.977272727272727,
0.980113636363636,0.982954545454545,0.984843013501228),.UNSPECIFIED.)
GEOMETRIC_REPRESENTATION_ITEM()
RATIONAL_B_SPLINE_SURFACE(((1.,0.923879532511287,1.,0.923879532511287,1.,
0.923879532511287,1.,0.923879532511287,1.,0.923879532511287,1.,0.923879532511287,
1.,0.923879532511287,1.,0.923879532511287,1.,0.923879532511287,1.,0.923879532511287,
1.,0.923879532511287,1.,0.923879532511287,1.,0.923879532511287,1.,0.923879532511287,
1.,0.923879532511287,1.,0.923879532511287,1.,0.923879532511287,1.,0.923879532511287,
1.,0.923879532511287,1.,0.923879532511287,1.,0.923879532511287,1.,0.923879532511287,
1.,0.923879532511287,1.,0.923879532511287,1.,0.923879532511287,1.,0.923879532511287,
1.,0.923879532511287,1.,0.923879532511287,1.,0.923879532511287,1.,0.923879532511287,
1.,0.923879532511287,1.,0.923879532511287,1.,0.923879532511287,1.,0.923879532511287,
1.,0.923879532511287,1.,0.923879532511287,1.,0.923879532511287,1.,0.923879532511287,
1.,0.923879532511287,1.,0.923879532511287,1.,0.923879532511287,1.,0.923879532511287,
1.,0.923879532511287,1.,0.923879532511287,1.,0.923879532511287,1.,0.923879532511287,
1.,0.923879532511287,1.,0.923879532511287,1.,0.923879532511287,1.,0.923879532511287,
1.,0.923879532511287,1.,0.923879532511287,1.,0.923879532511287,1.,0.923879532511287,
1.,0.923879532511287,1.,0.923879532511287,1.,0.923879532511287,1.,0.923879532511287,
1.,0.923879532511287,1.,0.923879532511287,1.,0.923879532511287,1.,0.923879532511287,
1.,0.923879532511287,1.,0.923879532511287,1.,0.923879532511287,1.,0.923879532511287,
1.,0.923879532511287,1.,0.923879532511287,1.,0.923879532511287,1.,0.923879532511287,
1.,0.923879532511287,1.,0.923879532511287,1.,0.923879532511287,1.,0.923879532511287,
1.,0.923879532511287,1.,0.923879532511287,1.,0.923879532511287,1.,0.923879532511287,
1.,0.923879532511287,1.,0.923879532511287,1.,0.923879532511287,1.,0.923879532511287,
1.,0.923879532511287,1.,0.923879532511287,1.,0.923879532511287,1.,0.923879532511287,
1.,0.923879532511287,1.,0.923879532511287,1.,0.923879532511287,1.,0.923879532511287,
1.,0.923879532511287,1.,0.923879532511287,1.,0.923879532511287,1.,0.923879532511287,
1.,0.923879532511287,1.,0.923879532511287,1.,0.923879532511287,1.,0.923879532511287,
1.,0.923879532511287,1.,0.923879532511287,1.,0.923879532511287,1.,0.923879532511287,
1.,0.923879532511287,1.,0.923879532511287,1.,0.923879532511287,1.,0.923879532511287,
1.,0.923879532511287,1.,0.923879532511287,1.,0.923879532511287,1.,0.923879532511287,
1.,0.923879532511287,1.,0.923879532511287,1.,0.923879532511287,1.,0.923879532511287,
1.,0.923879532511287,1.,0.923879532511287,1.,0.923879532511287,1.,0.923879532511287,
1.,0.923879532511287,1.,0.923879532511287,1.,0.923879532511287,1.,0.923879532511287,
1.,0.923879532511287,1.,0.923879532511287,1.,0.923879532511287,1.,0.923879532511287,
1.,0.923879532511287,1.,0.923879532511287,1.,0.923879532511287,1.,0.923879532511287,
1.,0.923879532511287,1.,0.923879532511287,1.,0.923879532511287,1.,0.923879532511287,
1.,0.923879532511287,1.,0.923879532511287,1.,0.923879532511287,1.,0.923879532511287,
1.,0.923879532511287,1.,0.923879532511287,1.,0.923879532511287,1.,0.923879532511287,
1.,0.923879532511287,1.,0.923879532511287,1.,0.923879532511287,1.,0.923879532511287,
1.,0.923879532511287,1.,0.923879532511287,1.,0.923879532511287,1.,0.923879532511287,
1.,0.923879532511287,1.,0.923879532511287,1.,0.923879532511287,1.,0.923879532511287,
1.,0.923879532511287,1.,0.923879532511287,1.,0.923879532511287,1.,0.923879532511287,
1.,0.923879532511287,1.,0.923879532511287,1.,0.923879532511287,1.,0.923879532511287,
1.,0.923879532511287,1.,0.923879532511287,1.,0.923879532511287,1.,0.923879532511287,
1.,0.923879532511287,1.,0.923879532511287,1.,0.923879532511287,1.,0.923879532511287,
1.,0.923879532511287,1.,0.923879532511287,1.,0.923879532511287,1.,0.923879532511287,
1.,0.923879532511287,1.,0.923879532511287,1.,0.923879532511287,1.,0.923879532511287,
1.,0.923879532511287,1.,0.923879532511287,1.,0.923879532511287,1.,0.923879532511287,
1.,0.923879532511287,1.,0.923879532511287,1.,0.923879532511287,1.,0.923879532511287,
1.,0.923879532511287,1.,0.923879532511287,1.,0.923879532511287,1.,0.923879532511287,
1.,0.923879532511287,1.,0.923879532511287,1.,0.923879532511287,1.,0.923879532511287,
1.,0.923879532511287,1.,0.923879532511287,1.,0.923879532511287,1.,0.923879532511287,
1.,0.923879532511287,1.,0.923879532511287,1.,0.923879532511287,1.,0.923879532511287,
1.,0.923879532511287,1.,0.923879532511287,1.,0.923879532511287,1.,0.923879532511287,
1.,0.923879532511287,1.,0.923879532511287,1.,0.923879532511287,1.,0.923879532511287,
1.,0.923879532511287,1.,0.923879532511287,1.,0.923879532511287,1.,0.923879532511287,
1.,0.923879532511287,1.,0.923879532511287,1.,0.923879532511287,1.,0.923879532511287,
1.,0.923879532511287,1.,0.923879532511287,1.,0.923879532511287,1.,0.923879532511287,
1.,0.923879532511287,1.,0.923879532511287,1.,0.923879532511287,1.,0.923879532511287,
1.,0.923879532511287,1.,0.923879532511287,1.,0.923879532511287,1.,0.923879532511287,
1.,0.923879532511287,1.,0.923879532511287,1.,0.923879532511287,1.,0.923879532511287,
1.,0.923879532511287,1.,0.923879532511287,1.,0.923879532511287,1.,0.923879532511287,
1.,0.923879532511287,1.,0.923879532511287,1.,0.923879532511287,1.,0.923879532511287,
1.,0.923879532511287,1.,0.923879532511287,1.,0.923879532511287,1.,0.923879532511287,
1.,0.923879532511287,1.,0.923879532511287,1.,0.923879532511287,1.,0.923879532511287,
1.,0.923879532511287,1.,0.923879532511287,1.,0.923879532511287,1.,0.923879532511287,
1.,0.923879532511287,1.,0.923879532511287,1.,0.923879532511287,1.,0.923879532511287,
1.,0.923879532511287,1.,0.923879532511287,1.,0.923879532511287,1.,0.923879532511287,
1.,0.923879532511287,1.,0.923879532511287,1.,0.923879532511287,1.,0.923879532511287,
1.,0.923879532511287,1.,0.923879532511287,1.,0.923879532511287,1.,0.923879532511287,
1.,0.923879532511287,1.,0.923879532511287,1.,0.923879532511287,1.,0.923879532511287,
1.,0.923879532511287,1.,0.923879532511287,1.,0.923879532511287,1.,0.923879532511287,
1.,0.923879532511287,1.,0.923879532511287,1.,0.923879532511287,1.,0.923879532511287,
1.,0.923879532511287,1.,0.923879532511287,1.,0.923879532511287,1.,0.923879532511287,
1.,0.923879532511287,1.,0.923879532511287,1.,0.923879532511287,1.,0.923879532511287,
1.,0.923879532511287,1.,0.923879532511287,1.,0.923879532511287,1.,0.923879532511287,
1.,0.923879532511287,1.,0.923879532511287,1.,0.923879532511287,1.,0.923879532511287,
1.,0.923879532511287,1.,0.923879532511287,1.,0.923879532511287,1.,0.923879532511287,
1.,0.923879532511287,1.,0.923879532511287,1.,0.923879532511287,1.,0.923879532511287,
1.,0.923879532511287,1.,0.923879532511287,1.,0.923879532511287,1.,0.923879532511287,
1.,0.923879532511287,1.,0.923879532511287,1.,0.923879532511287,1.,0.923879532511287,
1.,0.923879532511287,1.,0.923879532511287,1.,0.923879532511287,1.,0.923879532511287,
1.,0.923879532511287,1.,0.923879532511287,1.,0.923879532511287,1.,0.923879532511287,
1.,0.923879532511287,1.,0.923879532511287,1.,0.923879532511287,1.,0.923879532511287,
1.,0.923879532511287,1.,0.923879532511287,1.,0.923879532511287,1.,0.923879532511287,
1.,0.923879532511287,1.,0.923879532511287,1.,0.923879532511287,1.,0.923879532511287,
1.,0.923879532511287,1.,0.923879532511287,1.,0.923879532511287,1.,0.923879532511287,
1.,0.923879532511287,1.,0.923879532511287,1.,0.923879532511287,1.,0.923879532511287,
1.,0.923879532511287,1.,0.923879532511287,1.,0.923879532511287,1.,0.923879532511287,
1.,0.949399623166069,0.966071511472009),(1.,0.923879532511287,1.,0.923879532511287,
1.,0.923879532511287,1.,0.923879532511287,1.,0.923879532511287,1.,0.923879532511287,
1.,0.923879532511287,1.,0.923879532511287,1.,0.923879532511287,1.,0.923879532511287,
1.,0.923879532511287,1.,0.923879532511287,1.,0.923879532511287,1.,0.923879532511287,
1.,0.923879532511287,1.,0.923879532511287,1.,0.923879532511287,1.,0.923879532511287,
1.,0.923879532511287,1.,0.923879532511287,1.,0.923879532511287,1.,0.923879532511287,
1.,0.923879532511287,1.,0.923879532511287,1.,0.923879532511287,1.,0.923879532511287,
1.,0.923879532511287,1.,0.923879532511287,1.,0.923879532511287,1.,0.923879532511287,
1.,0.923879532511287,1.,0.923879532511287,1.,0.923879532511287,1.,0.923879532511287,
1.,0.923879532511287,1.,0.923879532511287,1.,0.923879532511287,1.,0.923879532511287,
1.,0.923879532511287,1.,0.923879532511287,1.,0.923879532511287,1.,0.923879532511287,
1.,0.923879532511287,1.,0.923879532511287,1.,0.923879532511287,1.,0.923879532511287,
1.,0.923879532511287,1.,0.923879532511287,1.,0.923879532511287,1.,0.923879532511287,
1.,0.923879532511287,1.,0.923879532511287,1.,0.923879532511287,1.,0.923879532511287,
1.,0.923879532511287,1.,0.923879532511287,1.,0.923879532511287,1.,0.923879532511287,
1.,0.923879532511287,1.,0.923879532511287,1.,0.923879532511287,1.,0.923879532511287,
1.,0.923879532511287,1.,0.923879532511287,1.,0.923879532511287,1.,0.923879532511287,
1.,0.923879532511287,1.,0.923879532511287,1.,0.923879532511287,1.,0.923879532511287,
1.,0.923879532511287,1.,0.923879532511287,1.,0.923879532511287,1.,0.923879532511287,
1.,0.923879532511287,1.,0.923879532511287,1.,0.923879532511287,1.,0.923879532511287,
1.,0.923879532511287,1.,0.923879532511287,1.,0.923879532511287,1.,0.923879532511287,
1.,0.923879532511287,1.,0.923879532511287,1.,0.923879532511287,1.,0.923879532511287,
1.,0.923879532511287,1.,0.923879532511287,1.,0.923879532511287,1.,0.923879532511287,
1.,0.923879532511287,1.,0.923879532511287,1.,0.923879532511287,1.,0.923879532511287,
1.,0.923879532511287,1.,0.923879532511287,1.,0.923879532511287,1.,0.923879532511287,
1.,0.923879532511287,1.,0.923879532511287,1.,0.923879532511287,1.,0.923879532511287,
1.,0.923879532511287,1.,0.923879532511287,1.,0.923879532511287,1.,0.923879532511287,
1.,0.923879532511287,1.,0.923879532511287,1.,0.923879532511287,1.,0.923879532511287,
1.,0.923879532511287,1.,0.923879532511287,1.,0.923879532511287,1.,0.923879532511287,
1.,0.923879532511287,1.,0.923879532511287,1.,0.923879532511287,1.,0.923879532511287,
1.,0.923879532511287,1.,0.923879532511287,1.,0.923879532511287,1.,0.923879532511287,
1.,0.923879532511287,1.,0.923879532511287,1.,0.923879532511287,1.,0.923879532511287,
1.,0.923879532511287,1.,0.923879532511287,1.,0.923879532511287,1.,0.923879532511287,
1.,0.923879532511287,1.,0.923879532511287,1.,0.923879532511287,1.,0.923879532511287,
1.,0.923879532511287,1.,0.923879532511287,1.,0.923879532511287,1.,0.923879532511287,
1.,0.923879532511287,1.,0.923879532511287,1.,0.923879532511287,1.,0.923879532511287,
1.,0.923879532511287,1.,0.923879532511287,1.,0.923879532511287,1.,0.923879532511287,
1.,0.923879532511287,1.,0.923879532511287,1.,0.923879532511287,1.,0.923879532511287,
1.,0.923879532511287,1.,0.923879532511287,1.,0.923879532511287,1.,0.923879532511287,
1.,0.923879532511287,1.,0.923879532511287,1.,0.923879532511287,1.,0.923879532511287,
1.,0.923879532511287,1.,0.923879532511287,1.,0.923879532511287,1.,0.923879532511287,
1.,0.923879532511287,1.,0.923879532511287,1.,0.923879532511287,1.,0.923879532511287,
1.,0.923879532511287,1.,0.923879532511287,1.,0.923879532511287,1.,0.923879532511287,
1.,0.923879532511287,1.,0.923879532511287,1.,0.923879532511287,1.,0.923879532511287,
1.,0.923879532511287,1.,0.923879532511287,1.,0.923879532511287,1.,0.923879532511287,
1.,0.923879532511287,1.,0.923879532511287,1.,0.923879532511287,1.,0.923879532511287,
1.,0.923879532511287,1.,0.923879532511287,1.,0.923879532511287,1.,0.923879532511287,
1.,0.923879532511287,1.,0.923879532511287,1.,0.923879532511287,1.,0.923879532511287,
1.,0.923879532511287,1.,0.923879532511287,1.,0.923879532511287,1.,0.923879532511287,
1.,0.923879532511287,1.,0.923879532511287,1.,0.923879532511287,1.,0.923879532511287,
1.,0.923879532511287,1.,0.923879532511287,1.,0.923879532511287,1.,0.923879532511287,
1.,0.923879532511287,1.,0.923879532511287,1.,0.923879532511287,1.,0.923879532511287,
1.,0.923879532511287,1.,0.923879532511287,1.,0.923879532511287,1.,0.923879532511287,
1.,0.923879532511287,1.,0.923879532511287,1.,0.923879532511287,1.,0.923879532511287,
1.,0.923879532511287,1.,0.923879532511287,1.,0.923879532511287,1.,0.923879532511287,
1.,0.923879532511287,1.,0.923879532511287,1.,0.923879532511287,1.,0.923879532511287,
1.,0.923879532511287,1.,0.923879532511287,1.,0.923879532511287,1.,0.923879532511287,
1.,0.923879532511287,1.,0.923879532511287,1.,0.923879532511287,1.,0.923879532511287,
1.,0.923879532511287,1.,0.923879532511287,1.,0.923879532511287,1.,0.923879532511287,
1.,0.923879532511287,1.,0.923879532511287,1.,0.923879532511287,1.,0.923879532511287,
1.,0.923879532511287,1.,0.923879532511287,1.,0.923879532511287,1.,0.923879532511287,
1.,0.923879532511287,1.,0.923879532511287,1.,0.923879532511287,1.,0.923879532511287,
1.,0.923879532511287,1.,0.923879532511287,1.,0.923879532511287,1.,0.923879532511287,
1.,0.923879532511287,1.,0.923879532511287,1.,0.923879532511287,1.,0.923879532511287,
1.,0.923879532511287,1.,0.923879532511287,1.,0.923879532511287,1.,0.923879532511287,
1.,0.923879532511287,1.,0.923879532511287,1.,0.923879532511287,1.,0.923879532511287,
1.,0.923879532511287,1.,0.923879532511287,1.,0.923879532511287,1.,0.923879532511287,
1.,0.923879532511287,1.,0.923879532511287,1.,0.923879532511287,1.,0.923879532511287,
1.,0.923879532511287,1.,0.923879532511287,1.,0.923879532511287,1.,0.923879532511287,
1.,0.923879532511287,1.,0.923879532511287,1.,0.923879532511287,1.,0.923879532511287,
1.,0.923879532511287,1.,0.923879532511287,1.,0.923879532511287,1.,0.923879532511287,
1.,0.923879532511287,1.,0.923879532511287,1.,0.923879532511287,1.,0.923879532511287,
1.,0.923879532511287,1.,0.923879532511287,1.,0.923879532511287,1.,0.923879532511287,
1.,0.923879532511287,1.,0.923879532511287,1.,0.923879532511287,1.,0.923879532511287,
1.,0.923879532511287,1.,0.923879532511287,1.,0.923879532511287,1.,0.923879532511287,
1.,0.923879532511287,1.,0.923879532511287,1.,0.923879532511287,1.,0.923879532511287,
1.,0.923879532511287,1.,0.923879532511287,1.,0.923879532511287,1.,0.923879532511287,
1.,0.923879532511287,1.,0.923879532511287,1.,0.923879532511287,1.,0.923879532511287,
1.,0.923879532511287,1.,0.923879532511287,1.,0.923879532511287,1.,0.923879532511287,
1.,0.923879532511287,1.,0.923879532511287,1.,0.923879532511287,1.,0.923879532511287,
1.,0.923879532511287,1.,0.923879532511287,1.,0.923879532511287,1.,0.923879532511287,
1.,0.923879532511287,1.,0.923879532511287,1.,0.923879532511287,1.,0.923879532511287,
1.,0.923879532511287,1.,0.923879532511287,1.,0.923879532511287,1.,0.923879532511287,
1.,0.923879532511287,1.,0.923879532511287,1.,0.923879532511287,1.,0.923879532511287,
1.,0.923879532511287,1.,0.923879532511287,1.,0.923879532511287,1.,0.923879532511287,
1.,0.923879532511287,1.,0.923879532511287,1.,0.923879532511287,1.,0.923879532511287,
1.,0.923879532511287,1.,0.923879532511287,1.,0.923879532511287,1.,0.923879532511287,
1.,0.949399623166069,0.966071511472009)))
REPRESENTATION_ITEM('')
SURFACE()
);
#589=(
BOUNDED_SURFACE()
B_SPLINE_SURFACE(3,2,((#41478,#41479,#41480,#41481,#41482,#41483,#41484,
#41485,#41486,#41487,#41488,#41489,#41490,#41491,#41492,#41493,#41494,#41495,
#41496,#41497,#41498,#41499,#41500,#41501,#41502,#41503,#41504,#41505,#41506,
#41507,#41508,#41509,#41510,#41511,#41512,#41513,#41514,#41515,#41516,#41517,
#41518,#41519,#41520,#41521,#41522,#41523,#41524,#41525,#41526,#41527,#41528,
#41529,#41530,#41531,#41532,#41533,#41534,#41535,#41536,#41537,#41538,#41539,
#41540,#41541,#41542,#41543,#41544,#41545,#41546,#41547,#41548,#41549,#41550,
#41551,#41552,#41553,#41554,#41555,#41556,#41557,#41558,#41559,#41560,#41561,
#41562,#41563,#41564,#41565,#41566,#41567,#41568,#41569,#41570,#41571,#41572,
#41573,#41574,#41575,#41576,#41577,#41578,#41579,#41580,#41581,#41582,#41583,
#41584,#41585,#41586,#41587,#41588,#41589,#41590,#41591,#41592,#41593,#41594,
#41595,#41596,#41597,#41598,#41599,#41600,#41601,#41602,#41603,#41604,#41605,
#41606,#41607,#41608,#41609,#41610,#41611,#41612,#41613,#41614,#41615,#41616,
#41617,#41618,#41619,#41620,#41621,#41622,#41623,#41624,#41625,#41626,#41627,
#41628,#41629,#41630,#41631,#41632,#41633,#41634,#41635,#41636,#41637,#41638,
#41639,#41640,#41641,#41642,#41643,#41644,#41645,#41646,#41647,#41648,#41649,
#41650,#41651,#41652,#41653,#41654,#41655,#41656,#41657,#41658,#41659,#41660,
#41661,#41662,#41663,#41664,#41665,#41666,#41667,#41668,#41669,#41670,#41671,
#41672,#41673,#41674,#41675,#41676,#41677,#41678,#41679,#41680,#41681,#41682,
#41683,#41684,#41685,#41686,#41687,#41688,#41689,#41690,#41691,#41692,#41693,
#41694,#41695,#41696,#41697,#41698,#41699,#41700,#41701,#41702,#41703,#41704,
#41705,#41706,#41707,#41708,#41709,#41710,#41711,#41712,#41713,#41714,#41715,
#41716,#41717,#41718,#41719,#41720,#41721,#41722,#41723,#41724,#41725,#41726,
#41727,#41728,#41729,#41730,#41731,#41732,#41733,#41734,#41735,#41736,#41737,
#41738,#41739,#41740,#41741,#41742,#41743,#41744,#41745,#41746,#41747,#41748,
#41749,#41750,#41751,#41752,#41753,#41754,#41755,#41756,#41757,#41758,#41759,
#41760,#41761,#41762,#41763,#41764,#41765,#41766,#41767,#41768,#41769,#41770,
#41771,#41772,#41773,#41774,#41775,#41776,#41777,#41778,#41779,#41780,#41781,
#41782,#41783,#41784,#41785,#41786,#41787,#41788,#41789,#41790,#41791,#41792,
#41793,#41794,#41795,#41796,#41797,#41798,#41799,#41800,#41801,#41802,#41803,
#41804,#41805,#41806,#41807,#41808,#41809,#41810,#41811,#41812,#41813,#41814,
#41815,#41816,#41817,#41818,#41819,#41820,#41821,#41822,#41823,#41824,#41825,
#41826,#41827,#41828,#41829,#41830,#41831,#41832,#41833,#41834,#41835,#41836,
#41837,#41838,#41839,#41840,#41841,#41842,#41843,#41844,#41845,#41846,#41847,
#41848,#41849,#41850,#41851,#41852,#41853,#41854,#41855,#41856,#41857,#41858,
#41859,#41860,#41861,#41862,#41863,#41864,#41865,#41866,#41867,#41868,#41869,
#41870,#41871,#41872,#41873,#41874,#41875,#41876,#41877,#41878,#41879,#41880,
#41881,#41882,#41883,#41884,#41885,#41886,#41887,#41888,#41889,#41890,#41891,
#41892,#41893,#41894,#41895,#41896,#41897,#41898,#41899,#41900,#41901,#41902,
#41903,#41904,#41905,#41906,#41907,#41908,#41909,#41910,#41911,#41912,#41913,
#41914,#41915,#41916,#41917,#41918,#41919,#41920,#41921,#41922,#41923,#41924,
#41925,#41926,#41927,#41928,#41929,#41930,#41931,#41932,#41933,#41934,#41935,
#41936,#41937,#41938,#41939,#41940,#41941,#41942,#41943,#41944,#41945,#41946,
#41947,#41948,#41949,#41950,#41951,#41952,#41953,#41954,#41955,#41956,#41957,
#41958,#41959,#41960,#41961,#41962,#41963,#41964,#41965,#41966,#41967,#41968,
#41969,#41970,#41971,#41972,#41973,#41974,#41975,#41976,#41977,#41978,#41979,
#41980,#41981,#41982,#41983,#41984,#41985,#41986,#41987,#41988,#41989,#41990,
#41991,#41992,#41993,#41994,#41995,#41996,#41997,#41998,#41999,#42000,#42001,
#42002,#42003,#42004,#42005,#42006,#42007,#42008,#42009,#42010,#42011,#42012,
#42013,#42014,#42015,#42016,#42017,#42018,#42019,#42020,#42021,#42022,#42023,
#42024,#42025,#42026,#42027,#42028,#42029,#42030,#42031,#42032,#42033,#42034,
#42035,#42036,#42037,#42038,#42039,#42040,#42041,#42042,#42043,#42044,#42045,
#42046,#42047,#42048,#42049,#42050,#42051,#42052,#42053,#42054,#42055,#42056,
#42057,#42058,#42059,#42060,#42061,#42062,#42063,#42064,#42065,#42066,#42067,
#42068,#42069,#42070,#42071,#42072,#42073,#42074,#42075,#42076,#42077,#42078,
#42079,#42080,#42081,#42082,#42083,#42084,#42085,#42086,#42087,#42088,#42089,
#42090,#42091,#42092,#42093,#42094,#42095,#42096,#42097,#42098,#42099,#42100,
#42101,#42102,#42103,#42104,#42105,#42106,#42107,#42108,#42109,#42110,#42111,
#42112,#42113,#42114,#42115,#42116,#42117,#42118,#42119,#42120,#42121,#42122,
#42123,#42124,#42125,#42126,#42127,#42128,#42129,#42130,#42131,#42132,#42133,
#42134,#42135,#42136,#42137,#42138,#42139,#42140,#42141,#42142,#42143,#42144,
#42145,#42146,#42147,#42148,#42149,#42150,#42151,#42152,#42153,#42154,#42155,
#42156,#42157,#42158,#42159,#42160,#42161,#42162,#42163,#42164,#42165,#42166,
#42167,#42168,#42169,#42170,#42171,#42172),(#42173,#42174,#42175,#42176,
#42177,#42178,#42179,#42180,#42181,#42182,#42183,#42184,#42185,#42186,#42187,
#42188,#42189,#42190,#42191,#42192,#42193,#42194,#42195,#42196,#42197,#42198,
#42199,#42200,#42201,#42202,#42203,#42204,#42205,#42206,#42207,#42208,#42209,
#42210,#42211,#42212,#42213,#42214,#42215,#42216,#42217,#42218,#42219,#42220,
#42221,#42222,#42223,#42224,#42225,#42226,#42227,#42228,#42229,#42230,#42231,
#42232,#42233,#42234,#42235,#42236,#42237,#42238,#42239,#42240,#42241,#42242,
#42243,#42244,#42245,#42246,#42247,#42248,#42249,#42250,#42251,#42252,#42253,
#42254,#42255,#42256,#42257,#42258,#42259,#42260,#42261,#42262,#42263,#42264,
#42265,#42266,#42267,#42268,#42269,#42270,#42271,#42272,#42273,#42274,#42275,
#42276,#42277,#42278,#42279,#42280,#42281,#42282,#42283,#42284,#42285,#42286,
#42287,#42288,#42289,#42290,#42291,#42292,#42293,#42294,#42295,#42296,#42297,
#42298,#42299,#42300,#42301,#42302,#42303,#42304,#42305,#42306,#42307,#42308,
#42309,#42310,#42311,#42312,#42313,#42314,#42315,#42316,#42317,#42318,#42319,
#42320,#42321,#42322,#42323,#42324,#42325,#42326,#42327,#42328,#42329,#42330,
#42331,#42332,#42333,#42334,#42335,#42336,#42337,#42338,#42339,#42340,#42341,
#42342,#42343,#42344,#42345,#42346,#42347,#42348,#42349,#42350,#42351,#42352,
#42353,#42354,#42355,#42356,#42357,#42358,#42359,#42360,#42361,#42362,#42363,
#42364,#42365,#42366,#42367,#42368,#42369,#42370,#42371,#42372,#42373,#42374,
#42375,#42376,#42377,#42378,#42379,#42380,#42381,#42382,#42383,#42384,#42385,
#42386,#42387,#42388,#42389,#42390,#42391,#42392,#42393,#42394,#42395,#42396,
#42397,#42398,#42399,#42400,#42401,#42402,#42403,#42404,#42405,#42406,#42407,
#42408,#42409,#42410,#42411,#42412,#42413,#42414,#42415,#42416,#42417,#42418,
#42419,#42420,#42421,#42422,#42423,#42424,#42425,#42426,#42427,#42428,#42429,
#42430,#42431,#42432,#42433,#42434,#42435,#42436,#42437,#42438,#42439,#42440,
#42441,#42442,#42443,#42444,#42445,#42446,#42447,#42448,#42449,#42450,#42451,
#42452,#42453,#42454,#42455,#42456,#42457,#42458,#42459,#42460,#42461,#42462,
#42463,#42464,#42465,#42466,#42467,#42468,#42469,#42470,#42471,#42472,#42473,
#42474,#42475,#42476,#42477,#42478,#42479,#42480,#42481,#42482,#42483,#42484,
#42485,#42486,#42487,#42488,#42489,#42490,#42491,#42492,#42493,#42494,#42495,
#42496,#42497,#42498,#42499,#42500,#42501,#42502,#42503,#42504,#42505,#42506,
#42507,#42508,#42509,#42510,#42511,#42512,#42513,#42514,#42515,#42516,#42517,
#42518,#42519,#42520,#42521,#42522,#42523,#42524,#42525,#42526,#42527,#42528,
#42529,#42530,#42531,#42532,#42533,#42534,#42535,#42536,#42537,#42538,#42539,
#42540,#42541,#42542,#42543,#42544,#42545,#42546,#42547,#42548,#42549,#42550,
#42551,#42552,#42553,#42554,#42555,#42556,#42557,#42558,#42559,#42560,#42561,
#42562,#42563,#42564,#42565,#42566,#42567,#42568,#42569,#42570,#42571,#42572,
#42573,#42574,#42575,#42576,#42577,#42578,#42579,#42580,#42581,#42582,#42583,
#42584,#42585,#42586,#42587,#42588,#42589,#42590,#42591,#42592,#42593,#42594,
#42595,#42596,#42597,#42598,#42599,#42600,#42601,#42602,#42603,#42604,#42605,
#42606,#42607,#42608,#42609,#42610,#42611,#42612,#42613,#42614,#42615,#42616,
#42617,#42618,#42619,#42620,#42621,#42622,#42623,#42624,#42625,#42626,#42627,
#42628,#42629,#42630,#42631,#42632,#42633,#42634,#42635,#42636,#42637,#42638,
#42639,#42640,#42641,#42642,#42643,#42644,#42645,#42646,#42647,#42648,#42649,
#42650,#42651,#42652,#42653,#42654,#42655,#42656,#42657,#42658,#42659,#42660,
#42661,#42662,#42663,#42664,#42665,#42666,#42667,#42668,#42669,#42670,#42671,
#42672,#42673,#42674,#42675,#42676,#42677,#42678,#42679,#42680,#42681,#42682,
#42683,#42684,#42685,#42686,#42687,#42688,#42689,#42690,#42691,#42692,#42693,
#42694,#42695,#42696,#42697,#42698,#42699,#42700,#42701,#42702,#42703,#42704,
#42705,#42706,#42707,#42708,#42709,#42710,#42711,#42712,#42713,#42714,#42715,
#42716,#42717,#42718,#42719,#42720,#42721,#42722,#42723,#42724,#42725,#42726,
#42727,#42728,#42729,#42730,#42731,#42732,#42733,#42734,#42735,#42736,#42737,
#42738,#42739,#42740,#42741,#42742,#42743,#42744,#42745,#42746,#42747,#42748,
#42749,#42750,#42751,#42752,#42753,#42754,#42755,#42756,#42757,#42758,#42759,
#42760,#42761,#42762,#42763,#42764,#42765,#42766,#42767,#42768,#42769,#42770,
#42771,#42772,#42773,#42774,#42775,#42776,#42777,#42778,#42779,#42780,#42781,
#42782,#42783,#42784,#42785,#42786,#42787,#42788,#42789,#42790,#42791,#42792,
#42793,#42794,#42795,#42796,#42797,#42798,#42799,#42800,#42801,#42802,#42803,
#42804,#42805,#42806,#42807,#42808,#42809,#42810,#42811,#42812,#42813,#42814,
#42815,#42816,#42817,#42818,#42819,#42820,#42821,#42822,#42823,#42824,#42825,
#42826,#42827,#42828,#42829,#42830,#42831,#42832,#42833,#42834,#42835,#42836,
#42837,#42838,#42839,#42840,#42841,#42842,#42843,#42844,#42845,#42846,#42847,
#42848,#42849,#42850,#42851,#42852,#42853,#42854,#42855,#42856,#42857,#42858,
#42859,#42860,#42861,#42862,#42863,#42864,#42865,#42866,#42867),(#42868,
#42869,#42870,#42871,#42872,#42873,#42874,#42875,#42876,#42877,#42878,#42879,
#42880,#42881,#42882,#42883,#42884,#42885,#42886,#42887,#42888,#42889,#42890,
#42891,#42892,#42893,#42894,#42895,#42896,#42897,#42898,#42899,#42900,#42901,
#42902,#42903,#42904,#42905,#42906,#42907,#42908,#42909,#42910,#42911,#42912,
#42913,#42914,#42915,#42916,#42917,#42918,#42919,#42920,#42921,#42922,#42923,
#42924,#42925,#42926,#42927,#42928,#42929,#42930,#42931,#42932,#42933,#42934,
#42935,#42936,#42937,#42938,#42939,#42940,#42941,#42942,#42943,#42944,#42945,
#42946,#42947,#42948,#42949,#42950,#42951,#42952,#42953,#42954,#42955,#42956,
#42957,#42958,#42959,#42960,#42961,#42962,#42963,#42964,#42965,#42966,#42967,
#42968,#42969,#42970,#42971,#42972,#42973,#42974,#42975,#42976,#42977,#42978,
#42979,#42980,#42981,#42982,#42983,#42984,#42985,#42986,#42987,#42988,#42989,
#42990,#42991,#42992,#42993,#42994,#42995,#42996,#42997,#42998,#42999,#43000,
#43001,#43002,#43003,#43004,#43005,#43006,#43007,#43008,#43009,#43010,#43011,
#43012,#43013,#43014,#43015,#43016,#43017,#43018,#43019,#43020,#43021,#43022,
#43023,#43024,#43025,#43026,#43027,#43028,#43029,#43030,#43031,#43032,#43033,
#43034,#43035,#43036,#43037,#43038,#43039,#43040,#43041,#43042,#43043,#43044,
#43045,#43046,#43047,#43048,#43049,#43050,#43051,#43052,#43053,#43054,#43055,
#43056,#43057,#43058,#43059,#43060,#43061,#43062,#43063,#43064,#43065,#43066,
#43067,#43068,#43069,#43070,#43071,#43072,#43073,#43074,#43075,#43076,#43077,
#43078,#43079,#43080,#43081,#43082,#43083,#43084,#43085,#43086,#43087,#43088,
#43089,#43090,#43091,#43092,#43093,#43094,#43095,#43096,#43097,#43098,#43099,
#43100,#43101,#43102,#43103,#43104,#43105,#43106,#43107,#43108,#43109,#43110,
#43111,#43112,#43113,#43114,#43115,#43116,#43117,#43118,#43119,#43120,#43121,
#43122,#43123,#43124,#43125,#43126,#43127,#43128,#43129,#43130,#43131,#43132,
#43133,#43134,#43135,#43136,#43137,#43138,#43139,#43140,#43141,#43142,#43143,
#43144,#43145,#43146,#43147,#43148,#43149,#43150,#43151,#43152,#43153,#43154,
#43155,#43156,#43157,#43158,#43159,#43160,#43161,#43162,#43163,#43164,#43165,
#43166,#43167,#43168,#43169,#43170,#43171,#43172,#43173,#43174,#43175,#43176,
#43177,#43178,#43179,#43180,#43181,#43182,#43183,#43184,#43185,#43186,#43187,
#43188,#43189,#43190,#43191,#43192,#43193,#43194,#43195,#43196,#43197,#43198,
#43199,#43200,#43201,#43202,#43203,#43204,#43205,#43206,#43207,#43208,#43209,
#43210,#43211,#43212,#43213,#43214,#43215,#43216,#43217,#43218,#43219,#43220,
#43221,#43222,#43223,#43224,#43225,#43226,#43227,#43228,#43229,#43230,#43231,
#43232,#43233,#43234,#43235,#43236,#43237,#43238,#43239,#43240,#43241,#43242,
#43243,#43244,#43245,#43246,#43247,#43248,#43249,#43250,#43251,#43252,#43253,
#43254,#43255,#43256,#43257,#43258,#43259,#43260,#43261,#43262,#43263,#43264,
#43265,#43266,#43267,#43268,#43269,#43270,#43271,#43272,#43273,#43274,#43275,
#43276,#43277,#43278,#43279,#43280,#43281,#43282,#43283,#43284,#43285,#43286,
#43287,#43288,#43289,#43290,#43291,#43292,#43293,#43294,#43295,#43296,#43297,
#43298,#43299,#43300,#43301,#43302,#43303,#43304,#43305,#43306,#43307,#43308,
#43309,#43310,#43311,#43312,#43313,#43314,#43315,#43316,#43317,#43318,#43319,
#43320,#43321,#43322,#43323,#43324,#43325,#43326,#43327,#43328,#43329,#43330,
#43331,#43332,#43333,#43334,#43335,#43336,#43337,#43338,#43339,#43340,#43341,
#43342,#43343,#43344,#43345,#43346,#43347,#43348,#43349,#43350,#43351,#43352,
#43353,#43354,#43355,#43356,#43357,#43358,#43359,#43360,#43361,#43362,#43363,
#43364,#43365,#43366,#43367,#43368,#43369,#43370,#43371,#43372,#43373,#43374,
#43375,#43376,#43377,#43378,#43379,#43380,#43381,#43382,#43383,#43384,#43385,
#43386,#43387,#43388,#43389,#43390,#43391,#43392,#43393,#43394,#43395,#43396,
#43397,#43398,#43399,#43400,#43401,#43402,#43403,#43404,#43405,#43406,#43407,
#43408,#43409,#43410,#43411,#43412,#43413,#43414,#43415,#43416,#43417,#43418,
#43419,#43420,#43421,#43422,#43423,#43424,#43425,#43426,#43427,#43428,#43429,
#43430,#43431,#43432,#43433,#43434,#43435,#43436,#43437,#43438,#43439,#43440,
#43441,#43442,#43443,#43444,#43445,#43446,#43447,#43448,#43449,#43450,#43451,
#43452,#43453,#43454,#43455,#43456,#43457,#43458,#43459,#43460,#43461,#43462,
#43463,#43464,#43465,#43466,#43467,#43468,#43469,#43470,#43471,#43472,#43473,
#43474,#43475,#43476,#43477,#43478,#43479,#43480,#43481,#43482,#43483,#43484,
#43485,#43486,#43487,#43488,#43489,#43490,#43491,#43492,#43493,#43494,#43495,
#43496,#43497,#43498,#43499,#43500,#43501,#43502,#43503,#43504,#43505,#43506,
#43507,#43508,#43509,#43510,#43511,#43512,#43513,#43514,#43515,#43516,#43517,
#43518,#43519,#43520,#43521,#43522,#43523,#43524,#43525,#43526,#43527,#43528,
#43529,#43530,#43531,#43532,#43533,#43534,#43535,#43536,#43537,#43538,#43539,
#43540,#43541,#43542,#43543,#43544,#43545,#43546,#43547,#43548,#43549,#43550,
#43551,#43552,#43553,#43554,#43555,#43556,#43557,#43558,#43559,#43560,#43561,
#43562),(#43563,#43564,#43565,#43566,#43567,#43568,#43569,#43570,#43571,
#43572,#43573,#43574,#43575,#43576,#43577,#43578,#43579,#43580,#43581,#43582,
#43583,#43584,#43585,#43586,#43587,#43588,#43589,#43590,#43591,#43592,#43593,
#43594,#43595,#43596,#43597,#43598,#43599,#43600,#43601,#43602,#43603,#43604,
#43605,#43606,#43607,#43608,#43609,#43610,#43611,#43612,#43613,#43614,#43615,
#43616,#43617,#43618,#43619,#43620,#43621,#43622,#43623,#43624,#43625,#43626,
#43627,#43628,#43629,#43630,#43631,#43632,#43633,#43634,#43635,#43636,#43637,
#43638,#43639,#43640,#43641,#43642,#43643,#43644,#43645,#43646,#43647,#43648,
#43649,#43650,#43651,#43652,#43653,#43654,#43655,#43656,#43657,#43658,#43659,
#43660,#43661,#43662,#43663,#43664,#43665,#43666,#43667,#43668,#43669,#43670,
#43671,#43672,#43673,#43674,#43675,#43676,#43677,#43678,#43679,#43680,#43681,
#43682,#43683,#43684,#43685,#43686,#43687,#43688,#43689,#43690,#43691,#43692,
#43693,#43694,#43695,#43696,#43697,#43698,#43699,#43700,#43701,#43702,#43703,
#43704,#43705,#43706,#43707,#43708,#43709,#43710,#43711,#43712,#43713,#43714,
#43715,#43716,#43717,#43718,#43719,#43720,#43721,#43722,#43723,#43724,#43725,
#43726,#43727,#43728,#43729,#43730,#43731,#43732,#43733,#43734,#43735,#43736,
#43737,#43738,#43739,#43740,#43741,#43742,#43743,#43744,#43745,#43746,#43747,
#43748,#43749,#43750,#43751,#43752,#43753,#43754,#43755,#43756,#43757,#43758,
#43759,#43760,#43761,#43762,#43763,#43764,#43765,#43766,#43767,#43768,#43769,
#43770,#43771,#43772,#43773,#43774,#43775,#43776,#43777,#43778,#43779,#43780,
#43781,#43782,#43783,#43784,#43785,#43786,#43787,#43788,#43789,#43790,#43791,
#43792,#43793,#43794,#43795,#43796,#43797,#43798,#43799,#43800,#43801,#43802,
#43803,#43804,#43805,#43806,#43807,#43808,#43809,#43810,#43811,#43812,#43813,
#43814,#43815,#43816,#43817,#43818,#43819,#43820,#43821,#43822,#43823,#43824,
#43825,#43826,#43827,#43828,#43829,#43830,#43831,#43832,#43833,#43834,#43835,
#43836,#43837,#43838,#43839,#43840,#43841,#43842,#43843,#43844,#43845,#43846,
#43847,#43848,#43849,#43850,#43851,#43852,#43853,#43854,#43855,#43856,#43857,
#43858,#43859,#43860,#43861,#43862,#43863,#43864,#43865,#43866,#43867,#43868,
#43869,#43870,#43871,#43872,#43873,#43874,#43875,#43876,#43877,#43878,#43879,
#43880,#43881,#43882,#43883,#43884,#43885,#43886,#43887,#43888,#43889,#43890,
#43891,#43892,#43893,#43894,#43895,#43896,#43897,#43898,#43899,#43900,#43901,
#43902,#43903,#43904,#43905,#43906,#43907,#43908,#43909,#43910,#43911,#43912,
#43913,#43914,#43915,#43916,#43917,#43918,#43919,#43920,#43921,#43922,#43923,
#43924,#43925,#43926,#43927,#43928,#43929,#43930,#43931,#43932,#43933,#43934,
#43935,#43936,#43937,#43938,#43939,#43940,#43941,#43942,#43943,#43944,#43945,
#43946,#43947,#43948,#43949,#43950,#43951,#43952,#43953,#43954,#43955,#43956,
#43957,#43958,#43959,#43960,#43961,#43962,#43963,#43964,#43965,#43966,#43967,
#43968,#43969,#43970,#43971,#43972,#43973,#43974,#43975,#43976,#43977,#43978,
#43979,#43980,#43981,#43982,#43983,#43984,#43985,#43986,#43987,#43988,#43989,
#43990,#43991,#43992,#43993,#43994,#43995,#43996,#43997,#43998,#43999,#44000,
#44001,#44002,#44003,#44004,#44005,#44006,#44007,#44008,#44009,#44010,#44011,
#44012,#44013,#44014,#44015,#44016,#44017,#44018,#44019,#44020,#44021,#44022,
#44023,#44024,#44025,#44026,#44027,#44028,#44029,#44030,#44031,#44032,#44033,
#44034,#44035,#44036,#44037,#44038,#44039,#44040,#44041,#44042,#44043,#44044,
#44045,#44046,#44047,#44048,#44049,#44050,#44051,#44052,#44053,#44054,#44055,
#44056,#44057,#44058,#44059,#44060,#44061,#44062,#44063,#44064,#44065,#44066,
#44067,#44068,#44069,#44070,#44071,#44072,#44073,#44074,#44075,#44076,#44077,
#44078,#44079,#44080,#44081,#44082,#44083,#44084,#44085,#44086,#44087,#44088,
#44089,#44090,#44091,#44092,#44093,#44094,#44095,#44096,#44097,#44098,#44099,
#44100,#44101,#44102,#44103,#44104,#44105,#44106,#44107,#44108,#44109,#44110,
#44111,#44112,#44113,#44114,#44115,#44116,#44117,#44118,#44119,#44120,#44121,
#44122,#44123,#44124,#44125,#44126,#44127,#44128,#44129,#44130,#44131,#44132,
#44133,#44134,#44135,#44136,#44137,#44138,#44139,#44140,#44141,#44142,#44143,
#44144,#44145,#44146,#44147,#44148,#44149,#44150,#44151,#44152,#44153,#44154,
#44155,#44156,#44157,#44158,#44159,#44160,#44161,#44162,#44163,#44164,#44165,
#44166,#44167,#44168,#44169,#44170,#44171,#44172,#44173,#44174,#44175,#44176,
#44177,#44178,#44179,#44180,#44181,#44182,#44183,#44184,#44185,#44186,#44187,
#44188,#44189,#44190,#44191,#44192,#44193,#44194,#44195,#44196,#44197,#44198,
#44199,#44200,#44201,#44202,#44203,#44204,#44205,#44206,#44207,#44208,#44209,
#44210,#44211,#44212,#44213,#44214,#44215,#44216,#44217,#44218,#44219,#44220,
#44221,#44222,#44223,#44224,#44225,#44226,#44227,#44228,#44229,#44230,#44231,
#44232,#44233,#44234,#44235,#44236,#44237,#44238,#44239,#44240,#44241,#44242,
#44243,#44244,#44245,#44246,#44247,#44248,#44249,#44250,#44251,#44252,#44253,
#44254,#44255,#44256,#44257)),.UNSPECIFIED.,.F.,.F.,.F.)
B_SPLINE_SURFACE_WITH_KNOTS((4,4),(3,2,2,2,2,2,2,2,2,2,2,2,2,2,2,2,2,2,
2,2,2,2,2,2,2,2,2,2,2,2,2,2,2,2,2,2,2,2,2,2,2,2,2,2,2,2,2,2,2,2,2,2,2,2,
2,2,2,2,2,2,2,2,2,2,2,2,2,2,2,2,2,2,2,2,2,2,2,2,2,2,2,2,2,2,2,2,2,2,2,2,
2,2,2,2,2,2,2,2,2,2,2,2,2,2,2,2,2,2,2,2,2,2,2,2,2,2,2,2,2,2,2,2,2,2,2,2,
2,2,2,2,2,2,2,2,2,2,2,2,2,2,2,2,2,2,2,2,2,2,2,2,2,2,2,2,2,2,2,2,2,2,2,2,
2,2,2,2,2,2,2,2,2,2,2,2,2,2,2,2,2,2,2,2,2,2,2,2,2,2,2,2,2,2,2,2,2,2,2,2,
2,2,2,2,2,2,2,2,2,2,2,2,2,2,2,2,2,2,2,2,2,2,2,2,2,2,2,2,2,2,2,2,2,2,2,2,
2,2,2,2,2,2,2,2,2,2,2,2,2,2,2,2,2,2,2,2,2,2,2,2,2,2,2,2,2,2,2,2,2,2,2,2,
2,2,2,2,2,2,2,2,2,2,2,2,2,2,2,2,2,2,2,2,2,2,2,2,2,2,2,2,2,2,2,2,2,2,2,2,
2,2,2,2,2,2,2,2,2,2,2,2,2,2,2,2,2,2,2,2,2,2,2,2,2,2,2,2,2,2,2,2,2,2,2,2,
2,2,2,2,2,3),(0.,1.),(0.,0.00284090909090909,0.00568181818181818,0.00852272727272727,
0.0113636363636364,0.0142045454545455,0.0170454545454545,0.0198863636363636,
0.0227272727272727,0.0255681818181818,0.0284090909090909,0.03125,0.0340909090909091,
0.0369318181818182,0.0397727272727273,0.0426136363636364,0.0454545454545455,
0.0482954545454545,0.0511363636363636,0.0539772727272727,0.0568181818181818,
0.0596590909090909,0.0625,0.0653409090909091,0.0681818181818182,0.0710227272727273,
0.0738636363636364,0.0767045454545455,0.0795454545454545,0.0823863636363636,
0.0852272727272727,0.0880681818181818,0.0909090909090909,0.09375,0.0965909090909091,
0.0994318181818182,0.102272727272727,0.105113636363636,0.107954545454545,
0.110795454545455,0.113636363636364,0.116477272727273,0.119318181818182,
0.122159090909091,0.125,0.127840909090909,0.130681818181818,0.133522727272727,
0.136363636363636,0.139204545454545,0.142045454545455,0.144886363636364,
0.147727272727273,0.150568181818182,0.153409090909091,0.15625,0.159090909090909,
0.161931818181818,0.164772727272727,0.167613636363636,0.170454545454545,
0.173295454545455,0.176136363636364,0.178977272727273,0.181818181818182,
0.184659090909091,0.1875,0.190340909090909,0.193181818181818,0.196022727272727,
0.198863636363636,0.201704545454545,0.204545454545455,0.207386363636364,
0.210227272727273,0.213068181818182,0.215909090909091,0.21875,0.221590909090909,
0.224431818181818,0.227272727272727,0.230113636363636,0.232954545454545,
0.235795454545455,0.238636363636364,0.241477272727273,0.244318181818182,
0.247159090909091,0.25,0.252840909090909,0.255681818181818,0.258522727272727,
0.261363636363636,0.264204545454545,0.267045454545455,0.269886363636364,
0.272727272727273,0.275568181818182,0.278409090909091,0.28125,0.284090909090909,
0.286931818181818,0.289772727272727,0.292613636363636,0.295454545454545,
0.298295454545455,0.301136363636364,0.303977272727273,0.306818181818182,
0.309659090909091,0.3125,0.315340909090909,0.318181818181818,0.321022727272727,
0.323863636363636,0.326704545454545,0.329545454545455,0.332386363636364,
0.335227272727273,0.338068181818182,0.340909090909091,0.34375,0.346590909090909,
0.349431818181818,0.352272727272727,0.355113636363636,0.357954545454545,
0.360795454545455,0.363636363636364,0.366477272727273,0.369318181818182,
0.372159090909091,0.375,0.377840909090909,0.380681818181818,0.383522727272727,
0.386363636363636,0.389204545454545,0.392045454545455,0.394886363636364,
0.397727272727273,0.400568181818182,0.403409090909091,0.40625,0.409090909090909,
0.411931818181818,0.414772727272727,0.417613636363636,0.420454545454545,
0.423295454545455,0.426136363636364,0.428977272727273,0.431818181818182,
0.434659090909091,0.4375,0.440340909090909,0.443181818181818,0.446022727272727,
0.448863636363636,0.451704545454545,0.454545454545455,0.457386363636364,
0.460227272727273,0.463068181818182,0.465909090909091,0.46875,0.471590909090909,
0.474431818181818,0.477272727272727,0.480113636363636,0.482954545454545,
0.485795454545455,0.488636363636364,0.491477272727273,0.494318181818182,
0.497159090909091,0.5,0.502840909090909,0.505681818181818,0.508522727272727,
0.511363636363636,0.514204545454545,0.517045454545455,0.519886363636364,
0.522727272727273,0.525568181818182,0.528409090909091,0.53125,0.534090909090909,
0.536931818181818,0.539772727272727,0.542613636363636,0.545454545454545,
0.548295454545455,0.551136363636364,0.553977272727273,0.556818181818182,
0.559659090909091,0.5625,0.565340909090909,0.568181818181818,0.571022727272727,
0.573863636363636,0.576704545454545,0.579545454545455,0.582386363636364,
0.585227272727273,0.588068181818182,0.590909090909091,0.59375,0.596590909090909,
0.599431818181818,0.602272727272727,0.605113636363636,0.607954545454545,
0.610795454545455,0.613636363636364,0.616477272727273,0.619318181818182,
0.622159090909091,0.625,0.627840909090909,0.630681818181818,0.633522727272727,
0.636363636363636,0.639204545454545,0.642045454545455,0.644886363636364,
0.647727272727273,0.650568181818182,0.653409090909091,0.65625,0.659090909090909,
0.661931818181818,0.664772727272727,0.667613636363636,0.670454545454545,
0.673295454545455,0.676136363636364,0.678977272727273,0.681818181818182,
0.684659090909091,0.6875,0.690340909090909,0.693181818181818,0.696022727272727,
0.698863636363636,0.701704545454545,0.704545454545455,0.707386363636364,
0.710227272727273,0.713068181818182,0.715909090909091,0.71875,0.721590909090909,
0.724431818181818,0.727272727272727,0.730113636363636,0.732954545454545,
0.735795454545455,0.738636363636364,0.741477272727273,0.744318181818182,
0.747159090909091,0.75,0.752840909090909,0.755681818181818,0.758522727272727,
0.761363636363636,0.764204545454545,0.767045454545455,0.769886363636364,
0.772727272727273,0.775568181818182,0.778409090909091,0.78125,0.784090909090909,
0.786931818181818,0.789772727272727,0.792613636363636,0.795454545454545,
0.798295454545455,0.801136363636364,0.803977272727273,0.806818181818182,
0.809659090909091,0.8125,0.815340909090909,0.818181818181818,0.821022727272727,
0.823863636363636,0.826704545454545,0.829545454545455,0.832386363636364,
0.835227272727273,0.838068181818182,0.840909090909091,0.84375,0.846590909090909,
0.849431818181818,0.852272727272727,0.855113636363636,0.857954545454545,
0.860795454545455,0.863636363636364,0.866477272727273,0.869318181818182,
0.872159090909091,0.875,0.877840909090909,0.880681818181818,0.883522727272727,
0.886363636363636,0.889204545454545,0.892045454545455,0.894886363636364,
0.897727272727273,0.900568181818182,0.903409090909091,0.90625,0.909090909090909,
0.911931818181818,0.914772727272727,0.917613636363636,0.920454545454545,
0.923295454545455,0.926136363636364,0.928977272727273,0.931818181818182,
0.934659090909091,0.9375,0.940340909090909,0.943181818181818,0.946022727272727,
0.948863636363636,0.951704545454545,0.954545454545455,0.957386363636364,
0.960227272727273,0.963068181818182,0.965909090909091,0.96875,0.971590909090909,
0.974431818181818,0.977272727272727,0.980113636363636,0.982954545454545,
0.98484301350122),.UNSPECIFIED.)
GEOMETRIC_REPRESENTATION_ITEM()
RATIONAL_B_SPLINE_SURFACE(((1.,0.923879532511287,1.,0.923879532511287,1.,
0.923879532511287,1.,0.923879532511287,1.,0.923879532511287,1.,0.923879532511287,
1.,0.923879532511287,1.,0.923879532511287,1.,0.923879532511287,1.,0.923879532511287,
1.,0.923879532511287,1.,0.923879532511287,1.,0.923879532511287,1.,0.923879532511287,
1.,0.923879532511287,1.,0.923879532511287,1.,0.923879532511287,1.,0.923879532511287,
1.,0.923879532511287,1.,0.923879532511287,1.,0.923879532511287,1.,0.923879532511287,
1.,0.923879532511287,1.,0.923879532511287,1.,0.923879532511287,1.,0.923879532511287,
1.,0.923879532511287,1.,0.923879532511287,1.,0.923879532511287,1.,0.923879532511287,
1.,0.923879532511287,1.,0.923879532511287,1.,0.923879532511287,1.,0.923879532511287,
1.,0.923879532511287,1.,0.923879532511287,1.,0.923879532511287,1.,0.923879532511287,
1.,0.923879532511287,1.,0.923879532511287,1.,0.923879532511287,1.,0.923879532511287,
1.,0.923879532511287,1.,0.923879532511287,1.,0.923879532511287,1.,0.923879532511287,
1.,0.923879532511287,1.,0.923879532511287,1.,0.923879532511287,1.,0.923879532511287,
1.,0.923879532511287,1.,0.923879532511287,1.,0.923879532511287,1.,0.923879532511287,
1.,0.923879532511287,1.,0.923879532511287,1.,0.923879532511287,1.,0.923879532511287,
1.,0.923879532511287,1.,0.923879532511287,1.,0.923879532511287,1.,0.923879532511287,
1.,0.923879532511287,1.,0.923879532511287,1.,0.923879532511287,1.,0.923879532511287,
1.,0.923879532511287,1.,0.923879532511287,1.,0.923879532511287,1.,0.923879532511287,
1.,0.923879532511287,1.,0.923879532511287,1.,0.923879532511287,1.,0.923879532511287,
1.,0.923879532511287,1.,0.923879532511287,1.,0.923879532511287,1.,0.923879532511287,
1.,0.923879532511287,1.,0.923879532511287,1.,0.923879532511287,1.,0.923879532511287,
1.,0.923879532511287,1.,0.923879532511287,1.,0.923879532511287,1.,0.923879532511287,
1.,0.923879532511287,1.,0.923879532511287,1.,0.923879532511287,1.,0.923879532511287,
1.,0.923879532511287,1.,0.923879532511287,1.,0.923879532511287,1.,0.923879532511287,
1.,0.923879532511287,1.,0.923879532511287,1.,0.923879532511287,1.,0.923879532511287,
1.,0.923879532511287,1.,0.923879532511287,1.,0.923879532511287,1.,0.923879532511287,
1.,0.923879532511287,1.,0.923879532511287,1.,0.923879532511287,1.,0.923879532511287,
1.,0.923879532511287,1.,0.923879532511287,1.,0.923879532511287,1.,0.923879532511287,
1.,0.923879532511287,1.,0.923879532511287,1.,0.923879532511287,1.,0.923879532511287,
1.,0.923879532511287,1.,0.923879532511287,1.,0.923879532511287,1.,0.923879532511287,
1.,0.923879532511287,1.,0.923879532511287,1.,0.923879532511287,1.,0.923879532511287,
1.,0.923879532511287,1.,0.923879532511287,1.,0.923879532511287,1.,0.923879532511287,
1.,0.923879532511287,1.,0.923879532511287,1.,0.923879532511287,1.,0.923879532511287,
1.,0.923879532511287,1.,0.923879532511287,1.,0.923879532511287,1.,0.923879532511287,
1.,0.923879532511287,1.,0.923879532511287,1.,0.923879532511287,1.,0.923879532511287,
1.,0.923879532511287,1.,0.923879532511287,1.,0.923879532511287,1.,0.923879532511287,
1.,0.923879532511287,1.,0.923879532511287,1.,0.923879532511287,1.,0.923879532511287,
1.,0.923879532511287,1.,0.923879532511287,1.,0.923879532511287,1.,0.923879532511287,
1.,0.923879532511287,1.,0.923879532511287,1.,0.923879532511287,1.,0.923879532511287,
1.,0.923879532511287,1.,0.923879532511287,1.,0.923879532511287,1.,0.923879532511287,
1.,0.923879532511287,1.,0.923879532511287,1.,0.923879532511287,1.,0.923879532511287,
1.,0.923879532511287,1.,0.923879532511287,1.,0.923879532511287,1.,0.923879532511287,
1.,0.923879532511287,1.,0.923879532511287,1.,0.923879532511287,1.,0.923879532511287,
1.,0.923879532511287,1.,0.923879532511287,1.,0.923879532511287,1.,0.923879532511287,
1.,0.923879532511287,1.,0.923879532511287,1.,0.923879532511287,1.,0.923879532511287,
1.,0.923879532511287,1.,0.923879532511287,1.,0.923879532511287,1.,0.923879532511287,
1.,0.923879532511287,1.,0.923879532511287,1.,0.923879532511287,1.,0.923879532511287,
1.,0.923879532511287,1.,0.923879532511287,1.,0.923879532511287,1.,0.923879532511287,
1.,0.923879532511287,1.,0.923879532511287,1.,0.923879532511287,1.,0.923879532511287,
1.,0.923879532511287,1.,0.923879532511287,1.,0.923879532511287,1.,0.923879532511287,
1.,0.923879532511287,1.,0.923879532511287,1.,0.923879532511287,1.,0.923879532511287,
1.,0.923879532511287,1.,0.923879532511287,1.,0.923879532511287,1.,0.923879532511287,
1.,0.923879532511287,1.,0.923879532511287,1.,0.923879532511287,1.,0.923879532511287,
1.,0.923879532511287,1.,0.923879532511287,1.,0.923879532511287,1.,0.923879532511287,
1.,0.923879532511287,1.,0.923879532511287,1.,0.923879532511287,1.,0.923879532511287,
1.,0.923879532511287,1.,0.923879532511287,1.,0.923879532511287,1.,0.923879532511287,
1.,0.923879532511287,1.,0.923879532511287,1.,0.923879532511287,1.,0.923879532511287,
1.,0.923879532511287,1.,0.923879532511287,1.,0.923879532511287,1.,0.923879532511287,
1.,0.923879532511287,1.,0.923879532511287,1.,0.923879532511287,1.,0.923879532511287,
1.,0.923879532511287,1.,0.923879532511287,1.,0.923879532511287,1.,0.923879532511287,
1.,0.923879532511287,1.,0.923879532511287,1.,0.923879532511287,1.,0.923879532511287,
1.,0.923879532511287,1.,0.923879532511287,1.,0.923879532511287,1.,0.923879532511287,
1.,0.923879532511287,1.,0.923879532511287,1.,0.923879532511287,1.,0.923879532511287,
1.,0.923879532511287,1.,0.923879532511287,1.,0.923879532511287,1.,0.923879532511287,
1.,0.923879532511287,1.,0.923879532511287,1.,0.923879532511287,1.,0.923879532511287,
1.,0.923879532511287,1.,0.923879532511287,1.,0.923879532511287,1.,0.923879532511287,
1.,0.923879532511287,1.,0.923879532511287,1.,0.923879532511287,1.,0.923879532511287,
1.,0.923879532511287,1.,0.923879532511287,1.,0.923879532511287,1.,0.923879532511287,
1.,0.923879532511287,1.,0.923879532511287,1.,0.923879532511287,1.,0.923879532511287,
1.,0.923879532511287,1.,0.923879532511287,1.,0.923879532511287,1.,0.923879532511287,
1.,0.923879532511287,1.,0.923879532511287,1.,0.923879532511287,1.,0.923879532511287,
1.,0.923879532511287,1.,0.923879532511287,1.,0.923879532511287,1.,0.923879532511287,
1.,0.923879532511287,1.,0.923879532511287,1.,0.923879532511287,1.,0.923879532511287,
1.,0.923879532511287,1.,0.923879532511287,1.,0.923879532511287,1.,0.923879532511287,
1.,0.923879532511287,1.,0.923879532511287,1.,0.923879532511287,1.,0.923879532511287,
1.,0.923879532511287,1.,0.923879532511287,1.,0.923879532511287,1.,0.923879532511287,
1.,0.923879532511287,1.,0.923879532511287,1.,0.923879532511287,1.,0.923879532511287,
1.,0.923879532511287,1.,0.923879532511287,1.,0.923879532511287,1.,0.923879532511287,
1.,0.923879532511287,1.,0.923879532511287,1.,0.923879532511287,1.,0.923879532511287,
1.,0.923879532511287,1.,0.923879532511287,1.,0.923879532511287,1.,0.923879532511287,
1.,0.923879532511287,1.,0.923879532511287,1.,0.923879532511287,1.,0.923879532511287,
1.,0.923879532511287,1.,0.923879532511287,1.,0.923879532511287,1.,0.923879532511287,
1.,0.923879532511287,1.,0.923879532511287,1.,0.923879532511287,1.,0.923879532511287,
1.,0.923879532511287,1.,0.923879532511287,1.,0.923879532511287,1.,0.923879532511287,
1.,0.923879532511287,1.,0.923879532511287,1.,0.923879532511287,1.,0.923879532511287,
1.,0.923879532511287,1.,0.923879532511287,1.,0.923879532511287,1.,0.923879532511287,
1.,0.923879532511287,1.,0.923879532511287,1.,0.923879532511287,1.,0.923879532511287,
1.,0.949399623166265,0.96607151147188),(0.994771161099481,0.919048715272298,
0.994771161099481,0.919048715272298,0.994771161099481,0.919048715272298,
0.994771161099481,0.919048715272298,0.994771161099481,0.919048715272298,
0.994771161099481,0.919048715272298,0.994771161099481,0.919048715272298,
0.994771161099481,0.919048715272298,0.994771161099481,0.919048715272298,
0.994771161099481,0.919048715272298,0.994771161099481,0.919048715272298,
0.994771161099481,0.919048715272298,0.994771161099481,0.919048715272298,
0.994771161099481,0.919048715272298,0.994771161099481,0.919048715272298,
0.994771161099481,0.919048715272298,0.994771161099481,0.919048715272298,
0.994771161099481,0.919048715272298,0.994771161099481,0.919048715272298,
0.994771161099481,0.919048715272298,0.994771161099481,0.919048715272298,
0.994771161099481,0.919048715272298,0.994771161099481,0.919048715272298,
0.994771161099481,0.919048715272298,0.994771161099481,0.919048715272298,
0.994771161099481,0.919048715272298,0.994771161099481,0.919048715272298,
0.994771161099481,0.919048715272298,0.994771161099481,0.919048715272298,
0.994771161099481,0.919048715272298,0.994771161099481,0.919048715272298,
0.994771161099481,0.919048715272298,0.994771161099481,0.919048715272298,
0.994771161099481,0.919048715272298,0.994771161099481,0.919048715272298,
0.994771161099481,0.919048715272298,0.994771161099481,0.919048715272298,
0.994771161099481,0.919048715272298,0.994771161099481,0.919048715272298,
0.994771161099481,0.919048715272298,0.994771161099481,0.919048715272298,
0.994771161099481,0.919048715272298,0.994771161099481,0.919048715272298,
0.994771161099481,0.919048715272298,0.994771161099481,0.919048715272298,
0.994771161099481,0.919048715272298,0.994771161099481,0.919048715272298,
0.994771161099481,0.919048715272298,0.994771161099481,0.919048715272298,
0.994771161099481,0.919048715272298,0.994771161099481,0.919048715272298,
0.994771161099481,0.919048715272298,0.994771161099481,0.919048715272298,
0.994771161099481,0.919048715272298,0.994771161099481,0.919048715272298,
0.994771161099481,0.919048715272298,0.994771161099481,0.919048715272298,
0.994771161099481,0.919048715272298,0.994771161099481,0.919048715272298,
0.994771161099481,0.919048715272298,0.994771161099481,0.919048715272298,
0.994771161099481,0.919048715272298,0.994771161099481,0.919048715272298,
0.994771161099481,0.919048715272298,0.994771161099481,0.919048715272298,
0.994771161099481,0.919048715272298,0.994771161099481,0.919048715272298,
0.994771161099481,0.919048715272298,0.994771161099481,0.919048715272298,
0.994771161099481,0.919048715272298,0.994771161099481,0.919048715272298,
0.994771161099481,0.919048715272298,0.994771161099481,0.919048715272298,
0.994771161099481,0.919048715272298,0.994771161099481,0.919048715272298,
0.994771161099481,0.919048715272298,0.994771161099481,0.919048715272298,
0.994771161099481,0.919048715272298,0.994771161099481,0.919048715272298,
0.994771161099481,0.919048715272298,0.994771161099481,0.919048715272298,
0.994771161099481,0.919048715272298,0.994771161099481,0.919048715272298,
0.994771161099481,0.919048715272298,0.994771161099481,0.919048715272298,
0.994771161099481,0.919048715272298,0.994771161099481,0.919048715272298,
0.994771161099481,0.919048715272298,0.994771161099481,0.919048715272298,
0.994771161099481,0.919048715272298,0.994771161099481,0.919048715272298,
0.994771161099481,0.919048715272298,0.994771161099481,0.919048715272298,
0.994771161099481,0.919048715272298,0.994771161099481,0.919048715272298,
0.994771161099481,0.919048715272298,0.994771161099481,0.919048715272298,
0.994771161099481,0.919048715272298,0.994771161099481,0.919048715272298,
0.994771161099481,0.919048715272298,0.994771161099481,0.919048715272298,
0.994771161099481,0.919048715272298,0.994771161099481,0.919048715272298,
0.994771161099481,0.919048715272298,0.994771161099481,0.919048715272298,
0.994771161099481,0.919048715272298,0.994771161099481,0.919048715272298,
0.994771161099481,0.919048715272298,0.994771161099481,0.919048715272298,
0.994771161099481,0.919048715272298,0.994771161099481,0.919048715272298,
0.994771161099481,0.919048715272298,0.994771161099481,0.919048715272298,
0.994771161099481,0.919048715272298,0.994771161099481,0.919048715272298,
0.994771161099481,0.919048715272298,0.994771161099481,0.919048715272298,
0.994771161099481,0.919048715272298,0.994771161099481,0.919048715272298,
0.994771161099481,0.919048715272298,0.994771161099481,0.919048715272298,
0.994771161099481,0.919048715272298,0.994771161099481,0.919048715272298,
0.994771161099481,0.919048715272298,0.994771161099481,0.919048715272298,
0.994771161099481,0.919048715272298,0.994771161099481,0.919048715272298,
0.994771161099481,0.919048715272298,0.994771161099481,0.919048715272298,
0.994771161099481,0.919048715272298,0.994771161099481,0.919048715272298,
0.994771161099481,0.919048715272298,0.994771161099481,0.919048715272298,
0.994771161099481,0.919048715272298,0.994771161099481,0.919048715272298,
0.994771161099481,0.919048715272298,0.994771161099481,0.919048715272298,
0.994771161099481,0.919048715272298,0.994771161099481,0.919048715272298,
0.994771161099481,0.919048715272298,0.994771161099481,0.919048715272298,
0.994771161099481,0.919048715272298,0.994771161099481,0.919048715272298,
0.994771161099481,0.919048715272298,0.994771161099481,0.919048715272298,
0.994771161099481,0.919048715272298,0.994771161099481,0.919048715272298,
0.994771161099481,0.919048715272298,0.994771161099481,0.919048715272298,
0.994771161099481,0.919048715272298,0.994771161099481,0.919048715272298,
0.994771161099481,0.919048715272298,0.994771161099481,0.919048715272298,
0.994771161099481,0.919048715272298,0.994771161099481,0.919048715272298,
0.994771161099481,0.919048715272298,0.994771161099481,0.919048715272298,
0.994771161099481,0.919048715272298,0.994771161099481,0.919048715272298,
0.994771161099481,0.919048715272298,0.994771161099481,0.919048715272298,
0.994771161099481,0.919048715272298,0.994771161099481,0.919048715272298,
0.994771161099481,0.919048715272298,0.994771161099481,0.919048715272298,
0.994771161099481,0.919048715272298,0.994771161099481,0.919048715272298,
0.994771161099481,0.919048715272298,0.994771161099481,0.919048715272298,
0.994771161099481,0.919048715272298,0.994771161099481,0.919048715272298,
0.994771161099481,0.919048715272298,0.994771161099481,0.919048715272298,
0.994771161099481,0.919048715272298,0.994771161099481,0.919048715272298,
0.994771161099481,0.919048715272298,0.994771161099481,0.919048715272298,
0.994771161099481,0.919048715272298,0.994771161099481,0.919048715272298,
0.994771161099481,0.919048715272298,0.994771161099481,0.919048715272298,
0.994771161099481,0.919048715272298,0.994771161099481,0.919048715272298,
0.994771161099481,0.919048715272298,0.994771161099481,0.919048715272298,
0.994771161099481,0.919048715272298,0.994771161099481,0.919048715272298,
0.994771161099481,0.919048715272298,0.994771161099481,0.919048715272298,
0.994771161099481,0.919048715272298,0.994771161099481,0.919048715272298,
0.994771161099481,0.919048715272298,0.994771161099481,0.919048715272298,
0.994771161099481,0.919048715272298,0.994771161099481,0.919048715272298,
0.994771161099481,0.919048715272298,0.994771161099481,0.919048715272298,
0.994771161099481,0.919048715272298,0.994771161099481,0.919048715272298,
0.994771161099481,0.919048715272298,0.994771161099481,0.919048715272298,
0.994771161099481,0.919048715272298,0.994771161099481,0.919048715272298,
0.994771161099481,0.919048715272298,0.994771161099481,0.919048715272298,
0.994771161099481,0.919048715272298,0.994771161099481,0.919048715272298,
0.994771161099481,0.919048715272298,0.994771161099481,0.919048715272298,
0.994771161099481,0.919048715272298,0.994771161099481,0.919048715272298,
0.994771161099481,0.919048715272298,0.994771161099481,0.919048715272298,
0.994771161099481,0.919048715272298,0.994771161099481,0.919048715272298,
0.994771161099481,0.919048715272298,0.994771161099481,0.919048715272298,
0.994771161099481,0.919048715272298,0.994771161099481,0.919048715272298,
0.994771161099481,0.919048715272298,0.994771161099481,0.919048715272298,
0.994771161099481,0.919048715272298,0.994771161099481,0.919048715272298,
0.994771161099481,0.919048715272298,0.994771161099481,0.919048715272298,
0.994771161099481,0.919048715272298,0.994771161099481,0.919048715272298,
0.994771161099481,0.919048715272298,0.994771161099481,0.919048715272298,
0.994771161099481,0.919048715272298,0.994771161099481,0.919048715272298,
0.994771161099481,0.919048715272298,0.994771161099481,0.919048715272298,
0.994771161099481,0.919048715272298,0.994771161099481,0.919048715272298,
0.994771161099481,0.919048715272298,0.994771161099481,0.919048715272298,
0.994771161099481,0.919048715272298,0.994771161099481,0.919048715272298,
0.994771161099481,0.919048715272298,0.994771161099481,0.919048715272298,
0.994771161099481,0.919048715272298,0.994771161099481,0.919048715272298,
0.994771161099481,0.919048715272298,0.994771161099481,0.919048715272298,
0.994771161099481,0.919048715272298,0.994771161099481,0.919048715272298,
0.994771161099481,0.919048715272298,0.994771161099481,0.919048715272298,
0.994771161099481,0.919048715272298,0.994771161099481,0.919048715272298,
0.994771161099481,0.919048715272298,0.994771161099481,0.919048715272298,
0.994771161099481,0.919048715272298,0.994771161099481,0.919048715272298,
0.994771161099481,0.919048715272298,0.994771161099481,0.919048715272298,
0.994771161099481,0.919048715272298,0.994771161099481,0.919048715272298,
0.994771161099481,0.919048715272298,0.994771161099481,0.919048715272298,
0.994771161099481,0.919048715272298,0.994771161099481,0.919048715272298,
0.994771161099481,0.919048715272298,0.994771161099481,0.919048715272298,
0.994771161099481,0.919048715272298,0.994771161099481,0.919048715272298,
0.994771161099481,0.919048715272298,0.994771161099481,0.919048715272298,
0.994771161099481,0.919048715272298,0.994771161099481,0.919048715272298,
0.994771161099481,0.919048715272298,0.994771161099481,0.919048715272298,
0.994771161099481,0.919048715272298,0.994771161099481,0.919048715272298,
0.994771161099481,0.919048715272298,0.994771161099481,0.919048715272298,
0.994771161099481,0.919048715272298,0.994771161099481,0.919048715272298,
0.994771161099481,0.919048715272298,0.994771161099481,0.919048715272298,
0.994771161099481,0.919048715272298,0.994771161099481,0.919048715272298,
0.994771161099481,0.919048715272298,0.994771161099481,0.919048715272298,
0.994771161099481,0.919048715272298,0.994771161099481,0.919048715272298,
0.994771161099481,0.919048715272298,0.994771161099481,0.919048715272298,
0.994771161099481,0.919048715272298,0.994771161099481,0.919048715272298,
0.994771161099481,0.919048715272298,0.994771161099481,0.919048715272298,
0.994771161099481,0.919048715272298,0.994771161099481,0.919048715272298,
0.994771161099481,0.919048715272298,0.994771161099481,0.919048715272298,
0.994771161099481,0.919048715272298,0.994771161099481,0.919048715272298,
0.994771161099481,0.919048715272298,0.994771161099481,0.919048715272298,
0.994771161099481,0.919048715272298,0.994771161099481,0.919048715272298,
0.994771161099481,0.919048715272298,0.994771161099481,0.919048715272298,
0.994771161099481,0.919048715272298,0.994771161099481,0.919048715272298,
0.994771161099481,0.919048715272298,0.994771161099481,0.919048715272298,
0.994771161099481,0.919048715272298,0.994771161099481,0.919048715272298,
0.994771161099481,0.919048715272298,0.994771161099481,0.919048715272298,
0.994771161099481,0.919048715272298,0.994771161099481,0.919048715272298,
0.994771161099481,0.919048715272298,0.994771161099481,0.919048715272298,
0.994771161099481,0.919048715272298,0.994771161099481,0.919048715272298,
0.994771161099481,0.919048715272298,0.994771161099481,0.919048715272298,
0.994771161099481,0.919048715272298,0.994771161099481,0.919048715272298,
0.994771161099481,0.919048715272298,0.994771161099481,0.919048715272298,
0.994771161099481,0.919048715272298,0.994771161099481,0.919048715272298,
0.994771161099481,0.919048715272298,0.994771161099481,0.919048715272298,
0.994771161099481,0.919048715272298,0.994771161099481,0.919048715272298,
0.994771161099481,0.919048715272298,0.994771161099481,0.919048715272298,
0.994771161099481,0.919048715272298,0.994771161099481,0.919048715272298,
0.994771161099481,0.919048715272298,0.994771161099481,0.919048715272298,
0.994771161099481,0.919048715272298,0.994771161099481,0.919048715272298,
0.994771161099481,0.919048715272298,0.994771161099481,0.919048715272298,
0.994771161099481,0.919048715272298,0.994771161099481,0.919048715272298,
0.994771161099481,0.919048715272298,0.994771161099481,0.919048715272298,
0.994771161099481,0.919048715272298,0.994771161099481,0.944435365484515,
0.961020079172012),(0.994771161099481,0.919048715272298,0.994771161099481,
0.919048715272298,0.994771161099481,0.919048715272298,0.994771161099481,
0.919048715272298,0.994771161099481,0.919048715272298,0.994771161099481,
0.919048715272298,0.994771161099481,0.919048715272298,0.994771161099481,
0.919048715272298,0.994771161099481,0.919048715272298,0.994771161099481,
0.919048715272298,0.994771161099481,0.919048715272298,0.994771161099481,
0.919048715272298,0.994771161099481,0.919048715272298,0.994771161099481,
0.919048715272298,0.994771161099481,0.919048715272298,0.994771161099481,
0.919048715272298,0.994771161099481,0.919048715272298,0.994771161099481,
0.919048715272298,0.994771161099481,0.919048715272298,0.994771161099481,
0.919048715272298,0.994771161099481,0.919048715272298,0.994771161099481,
0.919048715272298,0.994771161099481,0.919048715272298,0.994771161099481,
0.919048715272298,0.994771161099481,0.919048715272298,0.994771161099481,
0.919048715272298,0.994771161099481,0.919048715272298,0.994771161099481,
0.919048715272298,0.994771161099481,0.919048715272298,0.994771161099481,
0.919048715272298,0.994771161099481,0.919048715272298,0.994771161099481,
0.919048715272298,0.994771161099481,0.919048715272298,0.994771161099481,
0.919048715272298,0.994771161099481,0.919048715272298,0.994771161099481,
0.919048715272298,0.994771161099481,0.919048715272298,0.994771161099481,
0.919048715272298,0.994771161099481,0.919048715272298,0.994771161099481,
0.919048715272298,0.994771161099481,0.919048715272298,0.994771161099481,
0.919048715272298,0.994771161099481,0.919048715272298,0.994771161099481,
0.919048715272298,0.994771161099481,0.919048715272298,0.994771161099481,
0.919048715272298,0.994771161099481,0.919048715272298,0.994771161099481,
0.919048715272298,0.994771161099481,0.919048715272298,0.994771161099481,
0.919048715272298,0.994771161099481,0.919048715272298,0.994771161099481,
0.919048715272298,0.994771161099481,0.919048715272298,0.994771161099481,
0.919048715272298,0.994771161099481,0.919048715272298,0.994771161099481,
0.919048715272298,0.994771161099481,0.919048715272298,0.994771161099481,
0.919048715272298,0.994771161099481,0.919048715272298,0.994771161099481,
0.919048715272298,0.994771161099481,0.919048715272298,0.994771161099481,
0.919048715272298,0.994771161099481,0.919048715272298,0.994771161099481,
0.919048715272298,0.994771161099481,0.919048715272298,0.994771161099481,
0.919048715272298,0.994771161099481,0.919048715272298,0.994771161099481,
0.919048715272298,0.994771161099481,0.919048715272298,0.994771161099481,
0.919048715272298,0.994771161099481,0.919048715272298,0.994771161099481,
0.919048715272298,0.994771161099481,0.919048715272298,0.994771161099481,
0.919048715272298,0.994771161099481,0.919048715272298,0.994771161099481,
0.919048715272298,0.994771161099481,0.919048715272298,0.994771161099481,
0.919048715272298,0.994771161099481,0.919048715272298,0.994771161099481,
0.919048715272298,0.994771161099481,0.919048715272298,0.994771161099481,
0.919048715272298,0.994771161099481,0.919048715272298,0.994771161099481,
0.919048715272298,0.994771161099481,0.919048715272298,0.994771161099481,
0.919048715272298,0.994771161099481,0.919048715272298,0.994771161099481,
0.919048715272298,0.994771161099481,0.919048715272298,0.994771161099481,
0.919048715272298,0.994771161099481,0.919048715272298,0.994771161099481,
0.919048715272298,0.994771161099481,0.919048715272298,0.994771161099481,
0.919048715272298,0.994771161099481,0.919048715272298,0.994771161099481,
0.919048715272298,0.994771161099481,0.919048715272298,0.994771161099481,
0.919048715272298,0.994771161099481,0.919048715272298,0.994771161099481,
0.919048715272298,0.994771161099481,0.919048715272298,0.994771161099481,
0.919048715272298,0.994771161099481,0.919048715272298,0.994771161099481,
0.919048715272298,0.994771161099481,0.919048715272298,0.994771161099481,
0.919048715272298,0.994771161099481,0.919048715272298,0.994771161099481,
0.919048715272298,0.994771161099481,0.919048715272298,0.994771161099481,
0.919048715272298,0.994771161099481,0.919048715272298,0.994771161099481,
0.919048715272298,0.994771161099481,0.919048715272298,0.994771161099481,
0.919048715272298,0.994771161099481,0.919048715272298,0.994771161099481,
0.919048715272298,0.994771161099481,0.919048715272298,0.994771161099481,
0.919048715272298,0.994771161099481,0.919048715272298,0.994771161099481,
0.919048715272298,0.994771161099481,0.919048715272298,0.994771161099481,
0.919048715272298,0.994771161099481,0.919048715272298,0.994771161099481,
0.919048715272298,0.994771161099481,0.919048715272298,0.994771161099481,
0.919048715272298,0.994771161099481,0.919048715272298,0.994771161099481,
0.919048715272298,0.994771161099481,0.919048715272298,0.994771161099481,
0.919048715272298,0.994771161099481,0.919048715272298,0.994771161099481,
0.919048715272298,0.994771161099481,0.919048715272298,0.994771161099481,
0.919048715272298,0.994771161099481,0.919048715272298,0.994771161099481,
0.919048715272298,0.994771161099481,0.919048715272298,0.994771161099481,
0.919048715272298,0.994771161099481,0.919048715272298,0.994771161099481,
0.919048715272298,0.994771161099481,0.919048715272298,0.994771161099481,
0.919048715272298,0.994771161099481,0.919048715272298,0.994771161099481,
0.919048715272298,0.994771161099481,0.919048715272298,0.994771161099481,
0.919048715272298,0.994771161099481,0.919048715272298,0.994771161099481,
0.919048715272298,0.994771161099481,0.919048715272298,0.994771161099481,
0.919048715272298,0.994771161099481,0.919048715272298,0.994771161099481,
0.919048715272298,0.994771161099481,0.919048715272298,0.994771161099481,
0.919048715272298,0.994771161099481,0.919048715272298,0.994771161099481,
0.919048715272298,0.994771161099481,0.919048715272298,0.994771161099481,
0.919048715272298,0.994771161099481,0.919048715272298,0.994771161099481,
0.919048715272298,0.994771161099481,0.919048715272298,0.994771161099481,
0.919048715272298,0.994771161099481,0.919048715272298,0.994771161099481,
0.919048715272298,0.994771161099481,0.919048715272298,0.994771161099481,
0.919048715272298,0.994771161099481,0.919048715272298,0.994771161099481,
0.919048715272298,0.994771161099481,0.919048715272298,0.994771161099481,
0.919048715272298,0.994771161099481,0.919048715272298,0.994771161099481,
0.919048715272298,0.994771161099481,0.919048715272298,0.994771161099481,
0.919048715272298,0.994771161099481,0.919048715272298,0.994771161099481,
0.919048715272298,0.994771161099481,0.919048715272298,0.994771161099481,
0.919048715272298,0.994771161099481,0.919048715272298,0.994771161099481,
0.919048715272298,0.994771161099481,0.919048715272298,0.994771161099481,
0.919048715272298,0.994771161099481,0.919048715272298,0.994771161099481,
0.919048715272298,0.994771161099481,0.919048715272298,0.994771161099481,
0.919048715272298,0.994771161099481,0.919048715272298,0.994771161099481,
0.919048715272298,0.994771161099481,0.919048715272298,0.994771161099481,
0.919048715272298,0.994771161099481,0.919048715272298,0.994771161099481,
0.919048715272298,0.994771161099481,0.919048715272298,0.994771161099481,
0.919048715272298,0.994771161099481,0.919048715272298,0.994771161099481,
0.919048715272298,0.994771161099481,0.919048715272298,0.994771161099481,
0.919048715272298,0.994771161099481,0.919048715272298,0.994771161099481,
0.919048715272298,0.994771161099481,0.919048715272298,0.994771161099481,
0.919048715272298,0.994771161099481,0.919048715272298,0.994771161099481,
0.919048715272298,0.994771161099481,0.919048715272298,0.994771161099481,
0.919048715272298,0.994771161099481,0.919048715272298,0.994771161099481,
0.919048715272298,0.994771161099481,0.919048715272298,0.994771161099481,
0.919048715272298,0.994771161099481,0.919048715272298,0.994771161099481,
0.919048715272298,0.994771161099481,0.919048715272298,0.994771161099481,
0.919048715272298,0.994771161099481,0.919048715272298,0.994771161099481,
0.919048715272298,0.994771161099481,0.919048715272298,0.994771161099481,
0.919048715272298,0.994771161099481,0.919048715272298,0.994771161099481,
0.919048715272298,0.994771161099481,0.919048715272298,0.994771161099481,
0.919048715272298,0.994771161099481,0.919048715272298,0.994771161099481,
0.919048715272298,0.994771161099481,0.919048715272298,0.994771161099481,
0.919048715272298,0.994771161099481,0.919048715272298,0.994771161099481,
0.919048715272298,0.994771161099481,0.919048715272298,0.994771161099481,
0.919048715272298,0.994771161099481,0.919048715272298,0.994771161099481,
0.919048715272298,0.994771161099481,0.919048715272298,0.994771161099481,
0.919048715272298,0.994771161099481,0.919048715272298,0.994771161099481,
0.919048715272298,0.994771161099481,0.919048715272298,0.994771161099481,
0.919048715272298,0.994771161099481,0.919048715272298,0.994771161099481,
0.919048715272298,0.994771161099481,0.919048715272298,0.994771161099481,
0.919048715272298,0.994771161099481,0.919048715272298,0.994771161099481,
0.919048715272298,0.994771161099481,0.919048715272298,0.994771161099481,
0.919048715272298,0.994771161099481,0.919048715272298,0.994771161099481,
0.919048715272298,0.994771161099481,0.919048715272298,0.994771161099481,
0.919048715272298,0.994771161099481,0.919048715272298,0.994771161099481,
0.919048715272298,0.994771161099481,0.919048715272298,0.994771161099481,
0.919048715272298,0.994771161099481,0.919048715272298,0.994771161099481,
0.919048715272298,0.994771161099481,0.919048715272298,0.994771161099481,
0.919048715272298,0.994771161099481,0.919048715272298,0.994771161099481,
0.919048715272298,0.994771161099481,0.919048715272298,0.994771161099481,
0.919048715272298,0.994771161099481,0.919048715272298,0.994771161099481,
0.919048715272298,0.994771161099481,0.919048715272298,0.994771161099481,
0.919048715272298,0.994771161099481,0.919048715272298,0.994771161099481,
0.919048715272298,0.994771161099481,0.919048715272298,0.994771161099481,
0.919048715272298,0.994771161099481,0.919048715272298,0.994771161099481,
0.919048715272298,0.994771161099481,0.919048715272298,0.994771161099481,
0.919048715272298,0.994771161099481,0.919048715272298,0.994771161099481,
0.919048715272298,0.994771161099481,0.919048715272298,0.994771161099481,
0.919048715272298,0.994771161099481,0.919048715272298,0.994771161099481,
0.919048715272298,0.994771161099481,0.919048715272298,0.994771161099481,
0.919048715272298,0.994771161099481,0.919048715272298,0.994771161099481,
0.919048715272298,0.994771161099481,0.919048715272298,0.994771161099481,
0.919048715272298,0.994771161099481,0.919048715272298,0.994771161099481,
0.919048715272298,0.994771161099481,0.919048715272298,0.994771161099481,
0.919048715272298,0.994771161099481,0.919048715272298,0.994771161099481,
0.919048715272298,0.994771161099481,0.919048715272298,0.994771161099481,
0.919048715272298,0.994771161099481,0.919048715272298,0.994771161099481,
0.919048715272298,0.994771161099481,0.919048715272298,0.994771161099481,
0.919048715272298,0.994771161099481,0.919048715272298,0.994771161099481,
0.919048715272298,0.994771161099481,0.919048715272298,0.994771161099481,
0.919048715272298,0.994771161099481,0.919048715272298,0.994771161099481,
0.919048715272298,0.994771161099481,0.919048715272298,0.994771161099481,
0.919048715272298,0.994771161099481,0.919048715272298,0.994771161099481,
0.919048715272298,0.994771161099481,0.919048715272298,0.994771161099481,
0.919048715272298,0.994771161099481,0.919048715272298,0.994771161099481,
0.919048715272298,0.994771161099481,0.919048715272298,0.994771161099481,
0.919048715272298,0.994771161099481,0.919048715272298,0.994771161099481,
0.919048715272298,0.994771161099481,0.919048715272298,0.994771161099481,
0.919048715272298,0.994771161099481,0.919048715272298,0.994771161099481,
0.919048715272298,0.994771161099481,0.919048715272298,0.994771161099481,
0.919048715272298,0.994771161099481,0.919048715272298,0.994771161099481,
0.919048715272298,0.994771161099481,0.919048715272298,0.994771161099481,
0.919048715272298,0.994771161099481,0.919048715272298,0.994771161099481,
0.919048715272298,0.994771161099481,0.919048715272298,0.994771161099481,
0.919048715272298,0.994771161099481,0.919048715272298,0.994771161099481,
0.919048715272298,0.994771161099481,0.919048715272298,0.994771161099481,
0.919048715272298,0.994771161099481,0.919048715272298,0.994771161099481,
0.919048715272298,0.994771161099481,0.919048715272298,0.994771161099481,
0.919048715272298,0.994771161099481,0.919048715272298,0.994771161099481,
0.919048715272298,0.994771161099481,0.919048715272298,0.994771161099481,
0.919048715272298,0.994771161099481,0.919048715272298,0.994771161099481,
0.919048715272298,0.994771161099481,0.919048715272298,0.994771161099481,
0.919048715272298,0.994771161099481,0.944435365484515,0.961020079172012),
(1.,0.923879532511287,1.,0.923879532511287,1.,0.923879532511287,1.,0.923879532511287,
1.,0.923879532511287,1.,0.923879532511287,1.,0.923879532511287,1.,0.923879532511287,
1.,0.923879532511287,1.,0.923879532511287,1.,0.923879532511287,1.,0.923879532511287,
1.,0.923879532511287,1.,0.923879532511287,1.,0.923879532511287,1.,0.923879532511287,
1.,0.923879532511287,1.,0.923879532511287,1.,0.923879532511287,1.,0.923879532511287,
1.,0.923879532511287,1.,0.923879532511287,1.,0.923879532511287,1.,0.923879532511287,
1.,0.923879532511287,1.,0.923879532511287,1.,0.923879532511287,1.,0.923879532511287,
1.,0.923879532511287,1.,0.923879532511287,1.,0.923879532511287,1.,0.923879532511287,
1.,0.923879532511287,1.,0.923879532511287,1.,0.923879532511287,1.,0.923879532511287,
1.,0.923879532511287,1.,0.923879532511287,1.,0.923879532511287,1.,0.923879532511287,
1.,0.923879532511287,1.,0.923879532511287,1.,0.923879532511287,1.,0.923879532511287,
1.,0.923879532511287,1.,0.923879532511287,1.,0.923879532511287,1.,0.923879532511287,
1.,0.923879532511287,1.,0.923879532511287,1.,0.923879532511287,1.,0.923879532511287,
1.,0.923879532511287,1.,0.923879532511287,1.,0.923879532511287,1.,0.923879532511287,
1.,0.923879532511287,1.,0.923879532511287,1.,0.923879532511287,1.,0.923879532511287,
1.,0.923879532511287,1.,0.923879532511287,1.,0.923879532511287,1.,0.923879532511287,
1.,0.923879532511287,1.,0.923879532511287,1.,0.923879532511287,1.,0.923879532511287,
1.,0.923879532511287,1.,0.923879532511287,1.,0.923879532511287,1.,0.923879532511287,
1.,0.923879532511287,1.,0.923879532511287,1.,0.923879532511287,1.,0.923879532511287,
1.,0.923879532511287,1.,0.923879532511287,1.,0.923879532511287,1.,0.923879532511287,
1.,0.923879532511287,1.,0.923879532511287,1.,0.923879532511287,1.,0.923879532511287,
1.,0.923879532511287,1.,0.923879532511287,1.,0.923879532511287,1.,0.923879532511287,
1.,0.923879532511287,1.,0.923879532511287,1.,0.923879532511287,1.,0.923879532511287,
1.,0.923879532511287,1.,0.923879532511287,1.,0.923879532511287,1.,0.923879532511287,
1.,0.923879532511287,1.,0.923879532511287,1.,0.923879532511287,1.,0.923879532511287,
1.,0.923879532511287,1.,0.923879532511287,1.,0.923879532511287,1.,0.923879532511287,
1.,0.923879532511287,1.,0.923879532511287,1.,0.923879532511287,1.,0.923879532511287,
1.,0.923879532511287,1.,0.923879532511287,1.,0.923879532511287,1.,0.923879532511287,
1.,0.923879532511287,1.,0.923879532511287,1.,0.923879532511287,1.,0.923879532511287,
1.,0.923879532511287,1.,0.923879532511287,1.,0.923879532511287,1.,0.923879532511287,
1.,0.923879532511287,1.,0.923879532511287,1.,0.923879532511287,1.,0.923879532511287,
1.,0.923879532511287,1.,0.923879532511287,1.,0.923879532511287,1.,0.923879532511287,
1.,0.923879532511287,1.,0.923879532511287,1.,0.923879532511287,1.,0.923879532511287,
1.,0.923879532511287,1.,0.923879532511287,1.,0.923879532511287,1.,0.923879532511287,
1.,0.923879532511287,1.,0.923879532511287,1.,0.923879532511287,1.,0.923879532511287,
1.,0.923879532511287,1.,0.923879532511287,1.,0.923879532511287,1.,0.923879532511287,
1.,0.923879532511287,1.,0.923879532511287,1.,0.923879532511287,1.,0.923879532511287,
1.,0.923879532511287,1.,0.923879532511287,1.,0.923879532511287,1.,0.923879532511287,
1.,0.923879532511287,1.,0.923879532511287,1.,0.923879532511287,1.,0.923879532511287,
1.,0.923879532511287,1.,0.923879532511287,1.,0.923879532511287,1.,0.923879532511287,
1.,0.923879532511287,1.,0.923879532511287,1.,0.923879532511287,1.,0.923879532511287,
1.,0.923879532511287,1.,0.923879532511287,1.,0.923879532511287,1.,0.923879532511287,
1.,0.923879532511287,1.,0.923879532511287,1.,0.923879532511287,1.,0.923879532511287,
1.,0.923879532511287,1.,0.923879532511287,1.,0.923879532511287,1.,0.923879532511287,
1.,0.923879532511287,1.,0.923879532511287,1.,0.923879532511287,1.,0.923879532511287,
1.,0.923879532511287,1.,0.923879532511287,1.,0.923879532511287,1.,0.923879532511287,
1.,0.923879532511287,1.,0.923879532511287,1.,0.923879532511287,1.,0.923879532511287,
1.,0.923879532511287,1.,0.923879532511287,1.,0.923879532511287,1.,0.923879532511287,
1.,0.923879532511287,1.,0.923879532511287,1.,0.923879532511287,1.,0.923879532511287,
1.,0.923879532511287,1.,0.923879532511287,1.,0.923879532511287,1.,0.923879532511287,
1.,0.923879532511287,1.,0.923879532511287,1.,0.923879532511287,1.,0.923879532511287,
1.,0.923879532511287,1.,0.923879532511287,1.,0.923879532511287,1.,0.923879532511287,
1.,0.923879532511287,1.,0.923879532511287,1.,0.923879532511287,1.,0.923879532511287,
1.,0.923879532511287,1.,0.923879532511287,1.,0.923879532511287,1.,0.923879532511287,
1.,0.923879532511287,1.,0.923879532511287,1.,0.923879532511287,1.,0.923879532511287,
1.,0.923879532511287,1.,0.923879532511287,1.,0.923879532511287,1.,0.923879532511287,
1.,0.923879532511287,1.,0.923879532511287,1.,0.923879532511287,1.,0.923879532511287,
1.,0.923879532511287,1.,0.923879532511287,1.,0.923879532511287,1.,0.923879532511287,
1.,0.923879532511287,1.,0.923879532511287,1.,0.923879532511287,1.,0.923879532511287,
1.,0.923879532511287,1.,0.923879532511287,1.,0.923879532511287,1.,0.923879532511287,
1.,0.923879532511287,1.,0.923879532511287,1.,0.923879532511287,1.,0.923879532511287,
1.,0.923879532511287,1.,0.923879532511287,1.,0.923879532511287,1.,0.923879532511287,
1.,0.923879532511287,1.,0.923879532511287,1.,0.923879532511287,1.,0.923879532511287,
1.,0.923879532511287,1.,0.923879532511287,1.,0.923879532511287,1.,0.923879532511287,
1.,0.923879532511287,1.,0.923879532511287,1.,0.923879532511287,1.,0.923879532511287,
1.,0.923879532511287,1.,0.923879532511287,1.,0.923879532511287,1.,0.923879532511287,
1.,0.923879532511287,1.,0.923879532511287,1.,0.923879532511287,1.,0.923879532511287,
1.,0.923879532511287,1.,0.923879532511287,1.,0.923879532511287,1.,0.923879532511287,
1.,0.923879532511287,1.,0.923879532511287,1.,0.923879532511287,1.,0.923879532511287,
1.,0.923879532511287,1.,0.923879532511287,1.,0.923879532511287,1.,0.923879532511287,
1.,0.923879532511287,1.,0.923879532511287,1.,0.923879532511287,1.,0.923879532511287,
1.,0.923879532511287,1.,0.923879532511287,1.,0.923879532511287,1.,0.923879532511287,
1.,0.923879532511287,1.,0.923879532511287,1.,0.923879532511287,1.,0.923879532511287,
1.,0.923879532511287,1.,0.923879532511287,1.,0.923879532511287,1.,0.923879532511287,
1.,0.923879532511287,1.,0.923879532511287,1.,0.923879532511287,1.,0.923879532511287,
1.,0.923879532511287,1.,0.923879532511287,1.,0.923879532511287,1.,0.923879532511287,
1.,0.923879532511287,1.,0.923879532511287,1.,0.923879532511287,1.,0.923879532511287,
1.,0.923879532511287,1.,0.923879532511287,1.,0.923879532511287,1.,0.923879532511287,
1.,0.923879532511287,1.,0.923879532511287,1.,0.923879532511287,1.,0.923879532511287,
1.,0.923879532511287,1.,0.923879532511287,1.,0.923879532511287,1.,0.923879532511287,
1.,0.923879532511287,1.,0.923879532511287,1.,0.923879532511287,1.,0.923879532511287,
1.,0.923879532511287,1.,0.923879532511287,1.,0.923879532511287,1.,0.923879532511287,
1.,0.923879532511287,1.,0.923879532511287,1.,0.923879532511287,1.,0.923879532511287,
1.,0.923879532511287,1.,0.923879532511287,1.,0.923879532511287,1.,0.923879532511287,
1.,0.923879532511287,1.,0.923879532511287,1.,0.923879532511287,1.,0.923879532511287,
1.,0.923879532511287,1.,0.923879532511287,1.,0.923879532511287,1.,0.923879532511287,
1.,0.923879532511287,1.,0.923879532511287,1.,0.949399623166265,0.96607151147188)))
REPRESENTATION_ITEM('')
SURFACE()
);
#590=(
BOUNDED_SURFACE()
B_SPLINE_SURFACE(3,2,((#45068,#45069,#45070),(#45071,#45072,#45073),(#45074,
#45075,#45076),(#45077,#45078,#45079),(#45080,#45081,#45082),(#45083,#45084,
#45085),(#45086,#45087,#45088),(#45089,#45090,#45091)),.UNSPECIFIED.,.F.,
 .F.,.F.)
B_SPLINE_SURFACE_WITH_KNOTS((4,2,2,4),(3,3),(-0.000265671039808014,0.000664177599544138,
0.00132835519908425,0.00292238143798051),(-0.000697566251991853,1.),
 .UNSPECIFIED.)
GEOMETRIC_REPRESENTATION_ITEM()
RATIONAL_B_SPLINE_SURFACE(((1.00006735358899,0.951722442998278,1.),(1.00009085795633,
0.934875034398606,1.),(1.00011995255585,0.914020671505109,1.),(1.00017679132716,
0.873279902332299,1.),(1.000202236158,0.855041612592702,1.),(1.00029314270923,
0.789881815244371,1.),(1.00036608854593,0.737595859260726,1.),(1.00044993425484,
0.677497116903894,1.)))
REPRESENTATION_ITEM('')
SURFACE()
);
#591=(
BOUNDED_SURFACE()
B_SPLINE_SURFACE(3,2,((#45093,#45094,#45095),(#45096,#45097,#45098),(#45099,
#45100,#45101),(#45102,#45103,#45104)),.UNSPECIFIED.,.F.,.F.,.F.)
B_SPLINE_SURFACE_WITH_KNOTS((4,4),(3,3),(1.73472347597681E-18,0.00194751686681009),
(0.,1.),.UNSPECIFIED.)
GEOMETRIC_REPRESENTATION_ITEM()
RATIONAL_B_SPLINE_SURFACE(((1.,0.9363704575632,1.),(1.,0.937911573932337,
1.),(1.,0.939551224752395,1.),(1.,0.941276432107511,1.)))
REPRESENTATION_ITEM('')
SURFACE()
);
#592=(
BOUNDED_SURFACE()
B_SPLINE_SURFACE(3,2,((#45115,#45116,#45117),(#45118,#45119,#45120),(#45121,
#45122,#45123),(#45124,#45125,#45126),(#45127,#45128,#45129),(#45130,#45131,
#45132),(#45133,#45134,#45135),(#45136,#45137,#45138)),.UNSPECIFIED.,.F.,
 .F.,.F.)
B_SPLINE_SURFACE_WITH_KNOTS((4,2,2,4),(3,3),(-0.000264848297699882,0.00132424148849942,
0.00198636223274913,0.00291333127469873),(-0.000376747913465724,1.),
 .UNSPECIFIED.)
GEOMETRIC_REPRESENTATION_ITEM()
RATIONAL_B_SPLINE_SURFACE(((1.00024295987203,0.677556446441725,1.),(1.00019753111789,
0.73784709770907,1.),(1.00015862247899,0.789484595236775,1.),(1.00010910533939,
0.855201136507422,1.),(1.00009527454653,0.873556636784662,1.),(1.00006486797912,
0.91391063254542,1.),(1.00004913297578,0.934793300746539,1.),(1.0000362266027,
0.951921959744005,1.)))
REPRESENTATION_ITEM('')
SURFACE()
);
#593=(
BOUNDED_SURFACE()
B_SPLINE_SURFACE(3,2,((#45140,#45141,#45142),(#45143,#45144,#45145),(#45146,
#45147,#45148),(#45149,#45150,#45151)),.UNSPECIFIED.,.F.,.F.,.F.)
B_SPLINE_SURFACE_WITH_KNOTS((4,4),(3,3),(-3.46944695195361E-18,0.00194751686680595),
(0.,1.),.UNSPECIFIED.)
GEOMETRIC_REPRESENTATION_ITEM()
RATIONAL_B_SPLINE_SURFACE(((1.,0.936370457563209,1.),(1.,0.937911573932344,
1.),(1.,0.939551224752402,1.),(1.,0.941276432107508,1.)))
REPRESENTATION_ITEM('')
SURFACE()
);
#594=(
BOUNDED_SURFACE()
B_SPLINE_SURFACE(3,2,((#45152,#45153,#45154),(#45155,#45156,#45157),(#45158,
#45159,#45160),(#45161,#45162,#45163)),.UNSPECIFIED.,.F.,.F.,.F.)
B_SPLINE_SURFACE_WITH_KNOTS((4,4),(3,3),(-8.67361737988404E-19,0.00145502531726256),
(0.,1.),.UNSPECIFIED.)
GEOMETRIC_REPRESENTATION_ITEM()
RATIONAL_B_SPLINE_SURFACE(((1.,0.668532680377463,1.),(1.,0.667444009600454,
1.),(1.,0.666151431295988,1.),(1.,0.66453110293118,1.)))
REPRESENTATION_ITEM('')
SURFACE()
);
#595=(
BOUNDED_SURFACE()
B_SPLINE_SURFACE(3,2,((#45165,#45166,#45167),(#45168,#45169,#45170),(#45171,
#45172,#45173),(#45174,#45175,#45176),(#45177,#45178,#45179),(#45180,#45181,
#45182),(#45183,#45184,#45185),(#45186,#45187,#45188)),.UNSPECIFIED.,.F.,
 .F.,.F.)
B_SPLINE_SURFACE_WITH_KNOTS((4,2,2,4),(3,3),(-8.23993651088983E-18,0.000785858548320119,
0.00117878782248018,0.00157171709664025),(0.,1.),.UNSPECIFIED.)
GEOMETRIC_REPRESENTATION_ITEM()
RATIONAL_B_SPLINE_SURFACE(((1.,0.707106781186552,1.),(1.,0.700392709855563,
1.),(1.,0.693103478140052,1.),(1.,0.68292873029758,1.),(1.,0.679593975234355,
1.),(1.,0.673572573507934,1.),(1.,0.670859596930162,1.),(1.,0.668532680377463,
1.)))
REPRESENTATION_ITEM('')
SURFACE()
);
#596=(
BOUNDED_SURFACE()
B_SPLINE_SURFACE(3,2,((#45208,#45209,#45210),(#45211,#45212,#45213),(#45214,
#45215,#45216),(#45217,#45218,#45219),(#45220,#45221,#45222),(#45223,#45224,
#45225),(#45226,#45227,#45228),(#45229,#45230,#45231)),.UNSPECIFIED.,.F.,
 .F.,.F.)
B_SPLINE_SURFACE_WITH_KNOTS((4,2,2,4),(3,3),(-1.25767452008319E-17,0.000785889192074472,
0.00117883378811171,0.00157177838414896),(0.,1.),.UNSPECIFIED.)
GEOMETRIC_REPRESENTATION_ITEM()
RATIONAL_B_SPLINE_SURFACE(((1.,0.668532680377451,1.),(1.,0.673123216892149,
1.),(1.,0.679555858731309,1.),(1.,0.68973495589728,1.),(1.,0.693295125056467,
1.),(1.,0.700263684314459,1.),(1.,0.703699964289598,1.),(1.,0.707106781186548,
1.)))
REPRESENTATION_ITEM('')
SURFACE()
);
#597=(
BOUNDED_SURFACE()
B_SPLINE_SURFACE(3,2,((#45233,#45234,#45235),(#45236,#45237,#45238),(#45239,
#45240,#45241),(#45242,#45243,#45244)),.UNSPECIFIED.,.F.,.F.,.F.)
B_SPLINE_SURFACE_WITH_KNOTS((4,4),(3,3),(-8.67361737988404E-19,0.00145502531726205),
(0.,1.),.UNSPECIFIED.)
GEOMETRIC_REPRESENTATION_ITEM()
RATIONAL_B_SPLINE_SURFACE(((1.,0.668532680377451,1.),(1.,0.667444009600447,
1.),(1.,0.666151431295967,1.),(1.,0.664531102931197,1.)))
REPRESENTATION_ITEM('')
SURFACE()
);
#598=(
BOUNDED_SURFACE()
B_SPLINE_SURFACE(3,2,((#46726,#46727,#46728),(#46729,#46730,#46731),(#46732,
#46733,#46734),(#46735,#46736,#46737),(#46738,#46739,#46740),(#46741,#46742,
#46743),(#46744,#46745,#46746),(#46747,#46748,#46749),(#46750,#46751,#46752),
(#46753,#46754,#46755),(#46756,#46757,#46758),(#46759,#46760,#46761),(#46762,
#46763,#46764),(#46765,#46766,#46767),(#46768,#46769,#46770),(#46771,#46772,
#46773),(#46774,#46775,#46776),(#46777,#46778,#46779),(#46780,#46781,#46782),
(#46783,#46784,#46785),(#46786,#46787,#46788),(#46789,#46790,#46791),(#46792,
#46793,#46794),(#46795,#46796,#46797),(#46798,#46799,#46800),(#46801,#46802,
#46803),(#46804,#46805,#46806),(#46807,#46808,#46809),(#46810,#46811,#46812),
(#46813,#46814,#46815),(#46816,#46817,#46818),(#46819,#46820,#46821),(#46822,
#46823,#46824),(#46825,#46826,#46827)),.UNSPECIFIED.,.F.,.F.,.F.)
B_SPLINE_SURFACE_WITH_KNOTS((4,2,2,2,2,2,2,2,2,2,2,2,2,2,2,2,4),(3,3),(0.0462087893288186,
0.0464703270720222,0.0466010959436241,0.046666480379425,0.0467318648152259,
0.0472549403016333,0.048301091274448,0.0503933932200775,0.0545779971113364,
0.0629472048938543,0.07968562045889,0.0880548282414078,0.0964240360239257,
0.104793243806444,0.108977847697702,0.111070149643332,0.113162451588961),
(0.,1.),.UNSPECIFIED.)
GEOMETRIC_REPRESENTATION_ITEM()
RATIONAL_B_SPLINE_SURFACE(((1.,0.707106781186557,1.),(1.,0.707106781186557,
1.),(1.,0.707106781186551,1.),(1.,0.707106781186551,1.),(1.,0.707106781186557,
1.),(1.,0.707106781186557,1.),(1.,0.707106781186557,1.),(1.,0.707106781186557,
1.),(1.,0.707106781186557,1.),(1.,0.707106781186557,1.),(1.,0.707106781186557,
1.),(1.,0.707106781186557,1.),(1.,0.707106781186557,1.),(1.,0.707106781186557,
1.),(1.,0.707106781186562,1.),(1.,0.707106781186562,1.),(1.,0.707106781186557,
1.),(1.,0.707106781186557,1.),(1.,0.707106781186557,1.),(1.,0.707106781186557,
1.),(1.,0.707106781186557,1.),(1.,0.707106781186557,1.),(1.,0.707106781186538,
1.),(1.,0.707106781186538,1.),(1.,0.707106781186557,1.),(1.,0.707106781186557,
1.),(1.,0.707106781186557,1.),(1.,0.707106781186557,1.),(1.,0.707106781186556,
1.),(1.,0.707106781186556,1.),(1.,0.707106781186557,1.),(1.,0.707106781186557,
1.),(1.,0.707106781186548,1.),(1.,0.707106781186548,1.)))
REPRESENTATION_ITEM('')
SURFACE()
);
#599=(
BOUNDED_SURFACE()
B_SPLINE_SURFACE(3,2,((#46877,#46878,#46879),(#46880,#46881,#46882),(#46883,
#46884,#46885),(#46886,#46887,#46888),(#46889,#46890,#46891),(#46892,#46893,
#46894),(#46895,#46896,#46897),(#46898,#46899,#46900),(#46901,#46902,#46903),
(#46904,#46905,#46906),(#46907,#46908,#46909),(#46910,#46911,#46912),(#46913,
#46914,#46915),(#46916,#46917,#46918),(#46919,#46920,#46921),(#46922,#46923,
#46924),(#46925,#46926,#46927),(#46928,#46929,#46930),(#46931,#46932,#46933),
(#46934,#46935,#46936),(#46937,#46938,#46939),(#46940,#46941,#46942),(#46943,
#46944,#46945),(#46946,#46947,#46948),(#46949,#46950,#46951),(#46952,#46953,
#46954),(#46955,#46956,#46957),(#46958,#46959,#46960),(#46961,#46962,#46963),
(#46964,#46965,#46966),(#46967,#46968,#46969),(#46970,#46971,#46972),(#46973,
#46974,#46975),(#46976,#46977,#46978)),.UNSPECIFIED.,.F.,.F.,.F.)
B_SPLINE_SURFACE_WITH_KNOTS((4,2,2,2,2,2,2,2,2,2,2,2,2,2,2,2,4),(3,3),(0.0317072603307532,
0.0337720562518688,0.0358368521729843,0.0399664440152153,0.0482256276996774,
0.0564848113841394,0.0647439950686015,0.0812623624375256,0.0895215461219877,
0.0936511379642187,0.0957159338853342,0.096748331845892,0.0972645308261708,
0.0973290556987057,0.0973935805712406,0.0975226303163103,0.0977807298064497),
(0.,1.),.UNSPECIFIED.)
GEOMETRIC_REPRESENTATION_ITEM()
RATIONAL_B_SPLINE_SURFACE(((1.,0.707106781186557,1.),(1.,0.707106781186557,
1.),(1.,0.707106781186557,1.),(1.,0.707106781186557,1.),(1.,0.707106781186557,
1.),(1.,0.707106781186557,1.),(1.,0.707106781186556,1.),(1.,0.707106781186556,
1.),(1.,0.707106781186557,1.),(1.,0.707106781186557,1.),(1.,0.707106781186557,
1.),(1.,0.707106781186557,1.),(1.,0.707106781186557,1.),(1.,0.707106781186557,
1.),(1.,0.707106781186557,1.),(1.,0.707106781186557,1.),(1.,0.707106781186553,
1.),(1.,0.707106781186553,1.),(1.,0.707106781186557,1.),(1.,0.707106781186557,
1.),(1.,0.707106781186557,1.),(1.,0.707106781186557,1.),(1.,0.707106781186557,
1.),(1.,0.707106781186557,1.),(1.,0.707106781186557,1.),(1.,0.707106781186557,
1.),(1.,0.707106781186557,1.),(1.,0.707106781186557,1.),(1.,0.707106781186557,
1.),(1.,0.707106781186557,1.),(1.,0.707106781186557,1.),(1.,0.707106781186557,
1.),(1.,0.707106781186557,1.),(1.,0.707106781186557,1.)))
REPRESENTATION_ITEM('')
SURFACE()
);
#600=(
BOUNDED_SURFACE()
B_SPLINE_SURFACE(3,2,((#47073,#47074,#47075),(#47076,#47077,#47078),(#47079,
#47080,#47081),(#47082,#47083,#47084),(#47085,#47086,#47087),(#47088,#47089,
#47090),(#47091,#47092,#47093),(#47094,#47095,#47096),(#47097,#47098,#47099),
(#47100,#47101,#47102),(#47103,#47104,#47105),(#47106,#47107,#47108),(#47109,
#47110,#47111),(#47112,#47113,#47114),(#47115,#47116,#47117),(#47118,#47119,
#47120),(#47121,#47122,#47123),(#47124,#47125,#47126),(#47127,#47128,#47129),
(#47130,#47131,#47132),(#47133,#47134,#47135),(#47136,#47137,#47138)),
 .UNSPECIFIED.,.F.,.F.,.F.)
B_SPLINE_SURFACE_WITH_KNOTS((4,2,2,2,2,2,2,2,2,2,4),(3,3),(0.0497700329860562,
0.0499435417983895,0.0501170506107227,0.0504640682353892,0.0511581034847222,
0.0525461739833882,0.0553223149807202,0.0608745969753841,0.0719791609647121,
0.08308372495404,0.0941882889433679),(0.,1.),.UNSPECIFIED.)
GEOMETRIC_REPRESENTATION_ITEM()
RATIONAL_B_SPLINE_SURFACE(((1.,0.707106781186552,1.),(1.,0.707106781186552,
1.),(1.,0.707106781186548,1.),(1.,0.707106781186548,1.),(1.,0.707106781186548,
1.),(1.,0.707106781186548,1.),(1.,0.707106781186548,1.),(1.,0.707106781186548,
1.),(1.,0.707106781186548,1.),(1.,0.707106781186548,1.),(1.,0.707106781186552,
1.),(1.,0.707106781186552,1.),(1.,0.707106781186552,1.),(1.,0.707106781186552,
1.),(1.,0.707106781186543,1.),(1.,0.707106781186543,1.),(1.,0.707106781186548,
1.),(1.,0.707106781186548,1.),(1.,0.707106781186548,1.),(1.,0.707106781186548,
1.),(1.,0.707106781186548,1.),(1.,0.707106781186548,1.)))
REPRESENTATION_ITEM('')
SURFACE()
);
#601=(
BOUNDED_SURFACE()
B_SPLINE_SURFACE(3,2,((#47140,#47141,#47142),(#47143,#47144,#47145),(#47146,
#47147,#47148),(#47149,#47150,#47151),(#47152,#47153,#47154),(#47155,#47156,
#47157),(#47158,#47159,#47160),(#47161,#47162,#47163),(#47164,#47165,#47166),
(#47167,#47168,#47169),(#47170,#47171,#47172),(#47173,#47174,#47175),(#47176,
#47177,#47178),(#47179,#47180,#47181),(#47182,#47183,#47184),(#47185,#47186,
#47187),(#47188,#47189,#47190),(#47191,#47192,#47193),(#47194,#47195,#47196),
(#47197,#47198,#47199),(#47200,#47201,#47202),(#47203,#47204,#47205)),
 .UNSPECIFIED.,.F.,.F.,.F.)
B_SPLINE_SURFACE_WITH_KNOTS((4,2,2,2,2,2,2,2,2,2,4),(3,3),(0.00146045554386956,
0.00183455394335381,0.0020667680883163,0.00229898223327879,0.00241508930576004,
0.00253119637824129,0.00264730345072254,0.00276341052320378,0.00299562466816628,
0.00322783881312877,0.00360193721261649),(-0.000683445866355827,1.),
 .UNSPECIFIED.)
GEOMETRIC_REPRESENTATION_ITEM()
RATIONAL_B_SPLINE_SURFACE(((1.00042379451114,0.689957513824106,1.),(1.00040554234364,
0.703310559329287,1.),(1.00038207055231,0.720482212916271,1.),(1.00033118410993,
0.75771006437072,1.),(1.00030837452904,0.77439725351972,1.),(1.00025611113095,
0.812632467645312,1.),(1.00022596681978,0.834685648929338,1.),(1.0001846081175,
0.864943131131046,1.),(1.00017167736853,0.874403096882682,1.),(1.00015246067487,
0.88846177701933,1.),(1.00014653964815,0.892793522236095,1.),(1.00014594005926,
0.89323217357368,1.),(1.0001511099939,0.889449917438278,1.),(1.00016917206089,
0.876235946970749,1.),(1.00018188807499,0.866933078428389,1.),(1.0002231052286,
0.836779151366944,1.),(1.00025373494149,0.814370856578693,1.),(1.00030668059841,
0.775636510873654,1.),(1.00032978588761,0.758732985413562,1.),(1.00038153719649,
0.720872409012061,1.),(1.00040541002051,0.7034073651832,1.),(1.00042487779778,
0.689164995581676,1.)))
REPRESENTATION_ITEM('')
SURFACE()
);
#602=(
BOUNDED_SURFACE()
B_SPLINE_SURFACE(3,2,((#47207,#47208,#47209),(#47210,#47211,#47212),(#47213,
#47214,#47215),(#47216,#47217,#47218),(#47219,#47220,#47221),(#47222,#47223,
#47224),(#47225,#47226,#47227),(#47228,#47229,#47230),(#47231,#47232,#47233),
(#47234,#47235,#47236),(#47237,#47238,#47239),(#47240,#47241,#47242)),
 .UNSPECIFIED.,.F.,.F.,.F.)
B_SPLINE_SURFACE_WITH_KNOTS((4,2,2,2,2,4),(3,3),(0.0960380936069649,0.106151670712726,
0.111208459265607,0.113736853542047,0.115001050680268,0.116265247818488),
(0.,1.),.UNSPECIFIED.)
GEOMETRIC_REPRESENTATION_ITEM()
RATIONAL_B_SPLINE_SURFACE(((1.,0.707106781186548,1.),(1.,0.707106781186548,
1.),(1.,0.707106781186548,1.),(1.,0.707106781186548,1.),(1.,0.707106781186557,
1.),(1.,0.707106781186557,1.),(1.,0.707106781186549,1.),(1.,0.707106781186549,
1.),(1.,0.707106781186548,1.),(1.,0.707106781186548,1.),(1.,0.707106781186548,
1.),(1.,0.707106781186548,1.)))
REPRESENTATION_ITEM('')
SURFACE()
);
#603=(
BOUNDED_SURFACE()
B_SPLINE_SURFACE(3,2,((#47243,#47244,#47245),(#47246,#47247,#47248),(#47249,
#47250,#47251),(#47252,#47253,#47254),(#47255,#47256,#47257),(#47258,#47259,
#47260),(#47261,#47262,#47263),(#47264,#47265,#47266),(#47267,#47268,#47269),
(#47270,#47271,#47272),(#47273,#47274,#47275),(#47276,#47277,#47278),(#47279,
#47280,#47281),(#47282,#47283,#47284),(#47285,#47286,#47287),(#47288,#47289,
#47290),(#47291,#47292,#47293),(#47294,#47295,#47296),(#47297,#47298,#47299),
(#47300,#47301,#47302),(#47303,#47304,#47305),(#47306,#47307,#47308)),
 .UNSPECIFIED.,.F.,.F.,.F.)
B_SPLINE_SURFACE_WITH_KNOTS((4,2,2,2,2,2,2,2,2,2,4),(3,3),(0.057360394545972,
0.0683115303997951,0.0792626662536183,0.0902138021074414,0.095689370034353,
0.0984271539978088,0.0997960459795367,0.100480491970401,0.100822714965833,
0.100993826463549,0.101164937961265),(0.,1.),.UNSPECIFIED.)
GEOMETRIC_REPRESENTATION_ITEM()
RATIONAL_B_SPLINE_SURFACE(((1.,0.707106781186537,1.),(1.,0.707106781186537,
1.),(1.,0.707106781186548,1.),(1.,0.707106781186548,1.),(1.,0.707106781186552,
1.),(1.,0.707106781186552,1.),(1.,0.707106781186548,1.),(1.,0.707106781186548,
1.),(1.,0.707106781186548,1.),(1.,0.707106781186548,1.),(1.,0.707106781186549,
1.),(1.,0.707106781186549,1.),(1.,0.707106781186552,1.),(1.,0.707106781186552,
1.),(1.,0.707106781186548,1.),(1.,0.707106781186548,1.),(1.,0.707106781186552,
1.),(1.,0.707106781186552,1.),(1.,0.707106781186548,1.),(1.,0.707106781186548,
1.),(1.,0.707106781186549,1.),(1.,0.707106781186549,1.)))
REPRESENTATION_ITEM('')
SURFACE()
);
#604=(
BOUNDED_SURFACE()
B_SPLINE_SURFACE(3,2,((#47310,#47311,#47312),(#47313,#47314,#47315),(#47316,
#47317,#47318),(#47319,#47320,#47321),(#47322,#47323,#47324),(#47325,#47326,
#47327),(#47328,#47329,#47330),(#47331,#47332,#47333),(#47334,#47335,#47336),
(#47337,#47338,#47339),(#47340,#47341,#47342),(#47343,#47344,#47345),(#47346,
#47347,#47348),(#47349,#47350,#47351),(#47352,#47353,#47354),(#47355,#47356,
#47357),(#47358,#47359,#47360),(#47361,#47362,#47363),(#47364,#47365,#47366),
(#47367,#47368,#47369),(#47370,#47371,#47372),(#47373,#47374,#47375)),
 .UNSPECIFIED.,.F.,.F.,.F.)
B_SPLINE_SURFACE_WITH_KNOTS((4,2,2,2,2,2,2,2,2,2,4),(3,3),(0.00144383890556605,
0.00183455394336773,0.0020667680883287,0.00229898223328968,0.00241508930577017,
0.00253119637825066,0.00264730345073115,0.00276341052321164,0.00299562466817261,
0.00322783881313359,0.00361855385093527),(0.,1.00015850089284),
 .UNSPECIFIED.)
GEOMETRIC_REPRESENTATION_ITEM()
RATIONAL_B_SPLINE_SURFACE(((1.,0.688364167948368,1.00009878911524),(1.,
0.70195297713868,1.00009448143846),(1.,0.719609110627684,1.00008888441262),
(1.,0.757837166390466,1.00007676605068),(1.,0.774515601665459,1.00007147895692),
(1.,0.812730758117016,1.00005936468408),(1.,0.834772370599585,1.00005237745356),
(1.,0.865013980137201,1.00004279080934),(1.,0.874468983318253,1.00003979355645),
(1.,0.8885202884607,1.00003533926763),(1.,0.89284976130205,1.000033966817),
(1.,0.893288182527816,1.00003382783669),(1.,0.889507910512134,1.00003502618967),
(1.,0.876300871913868,1.00003921284449),(1.,0.867002883530373,1.00004216032341),
(1.,0.836864774809164,1.00005171415769),(1.,0.814468235110218,1.00005881390077),
(1.,0.775754208917403,1.0000710863162),(1.,0.758859550818501,1.00007644195299),
(1.,0.719981770628353,1.00008876627873),(1.,0.702023873648148,1.00009445896414),
(1.,0.687450036010001,1.0000990788967)))
REPRESENTATION_ITEM('')
SURFACE()
);
#605=(
BOUNDED_SURFACE()
B_SPLINE_SURFACE(3,2,((#47377,#47378,#47379),(#47380,#47381,#47382),(#47383,
#47384,#47385),(#47386,#47387,#47388),(#47389,#47390,#47391),(#47392,#47393,
#47394),(#47395,#47396,#47397),(#47398,#47399,#47400),(#47401,#47402,#47403),
(#47404,#47405,#47406),(#47407,#47408,#47409),(#47410,#47411,#47412)),
 .UNSPECIFIED.,.F.,.F.,.F.)
B_SPLINE_SURFACE_WITH_KNOTS((4,2,2,2,2,4),(3,3),(0.0355884658045091,0.0368351959435732,
0.0380819260826373,0.0405753863607654,0.0455623069170217,0.0555361480295343),
(0.,1.),.UNSPECIFIED.)
GEOMETRIC_REPRESENTATION_ITEM()
RATIONAL_B_SPLINE_SURFACE(((1.,0.707106781186548,1.),(1.,0.707106781186548,
1.),(1.,0.707106781186548,1.),(1.,0.707106781186548,1.),(1.,0.707106781186548,
1.),(1.,0.707106781186548,1.),(1.,0.707106781186567,1.),(1.,0.707106781186567,
1.),(1.,0.707106781186548,1.),(1.,0.707106781186548,1.),(1.,0.707106781186548,
1.),(1.,0.707106781186548,1.)))
REPRESENTATION_ITEM('')
SURFACE()
);
#606=TOROIDAL_SURFACE('',#9082,2.00000000000001,0.4);
#607=TOROIDAL_SURFACE('',#9088,2.,0.4);
#608=TOROIDAL_SURFACE('',#9093,1.79999999999999,0.4);
#609=TOROIDAL_SURFACE('',#9096,1.8,0.4);
#610=TOROIDAL_SURFACE('',#9128,39.,0.5);
#611=TOROIDAL_SURFACE('',#9132,39.,0.5);
#612=TOROIDAL_SURFACE('',#9136,6.15470053837925,0.5);
#613=TOROIDAL_SURFACE('',#9140,6.15470053837925,0.5);
#614=TOROIDAL_SURFACE('',#9282,11.1547005383793,0.5);
#615=TOROIDAL_SURFACE('',#9286,11.1547005383793,0.5);
#616=TOROIDAL_SURFACE('',#9298,15.5,0.5);
#617=TOROIDAL_SURFACE('',#9302,14.5,0.5);
#618=TOROIDAL_SURFACE('',#9305,15.5,0.5);
#619=TOROIDAL_SURFACE('',#9309,14.5,0.5);
#620=TOROIDAL_SURFACE('',#9319,14.5,0.5);
#621=TOROIDAL_SURFACE('',#9323,15.5,0.5);
#622=TOROIDAL_SURFACE('',#9333,12.2,0.5);
#623=TOROIDAL_SURFACE('',#9335,9.5,0.5);
#624=TOROIDAL_SURFACE('',#9337,4.5,0.5);
#625=TOROIDAL_SURFACE('',#9338,4.5,0.5);
#626=TOROIDAL_SURFACE('',#9340,9.5,0.5);
#627=TOROIDAL_SURFACE('',#9342,12.2,0.5);
#628=TOROIDAL_SURFACE('',#9404,6.,1.);
#629=TOROIDAL_SURFACE('',#9434,6.,1.);
#630=TOROIDAL_SURFACE('',#9516,5.9,0.5);
#631=TOROIDAL_SURFACE('',#9521,5.9,0.5);
#632=TOROIDAL_SURFACE('',#9535,14.989297312108,1.);
#633=TOROIDAL_SURFACE('',#9539,14.989297312108,1.);
#634=TOROIDAL_SURFACE('',#9626,6.44337567297407,1.);
#635=TOROIDAL_SURFACE('',#9628,106.443375672974,1.);
#636=TOROIDAL_SURFACE('',#9629,6.44337567297407,1.);
#637=TOROIDAL_SURFACE('',#9631,106.443375672974,1.);
#638=TOROIDAL_SURFACE('',#9660,15.5,0.5);
#639=TOROIDAL_SURFACE('',#9663,3.5,0.5);
#640=TOROIDAL_SURFACE('',#9666,35.5,0.5);
#641=TOROIDAL_SURFACE('',#9668,27.5,0.5);
#642=TOROIDAL_SURFACE('',#9671,15.5,0.5);
#643=TOROIDAL_SURFACE('',#9674,3.5,0.5);
#644=TOROIDAL_SURFACE('',#9677,35.5,0.5);
#645=TOROIDAL_SURFACE('',#9679,27.5,0.5);
#646=TOROIDAL_SURFACE('',#9684,100.5,0.5);
#647=TOROIDAL_SURFACE('',#9686,12.5,0.5);
#648=TOROIDAL_SURFACE('',#9688,6.5,0.5);
#649=TOROIDAL_SURFACE('',#9696,6.5,0.5);
#650=TOROIDAL_SURFACE('',#9698,12.5,0.5);
#651=TOROIDAL_SURFACE('',#9700,100.5,0.5);
#652=TOROIDAL_SURFACE('',#9704,76.5,1.5);
#653=TOROIDAL_SURFACE('',#9707,76.5,1.5);
#654=TOROIDAL_SURFACE('',#9710,219.,3.);
#655=TOROIDAL_SURFACE('',#9713,219.,3.);
#656=TOROIDAL_SURFACE('',#9788,103.,3.);
#657=TOROIDAL_SURFACE('',#9790,103.,3.);
#658=TOROIDAL_SURFACE('',#9797,4.43478616545488,1.5);
#659=TOROIDAL_SURFACE('',#9804,4.43478616545488,1.5);
#660=TOROIDAL_SURFACE('',#9872,2.25,0.25);
#661=TOROIDAL_SURFACE('',#9876,4.15,0.25);
#662=TOROIDAL_SURFACE('',#9881,2.25,0.25);
#663=TOROIDAL_SURFACE('',#9885,4.15,0.25);
#664=TOROIDAL_SURFACE('',#9890,2.25,0.25);
#665=TOROIDAL_SURFACE('',#9894,2.25,0.25);
#666=TOROIDAL_SURFACE('',#9928,4.15,0.25);
#667=TOROIDAL_SURFACE('',#9929,20.25,0.25);
#668=TOROIDAL_SURFACE('',#9932,9.75,0.25);
#669=TOROIDAL_SURFACE('',#9934,24.25,0.25);
#670=TOROIDAL_SURFACE('',#9936,9.75,0.25);
#671=TOROIDAL_SURFACE('',#9938,4.15,0.25);
#672=TOROIDAL_SURFACE('',#9940,24.25,0.25);
#673=TOROIDAL_SURFACE('',#9942,20.25,0.25);
#674=SHAPE_REPRESENTATION_RELATIONSHIP('SRR','None',#47761,#686);
#675=SHAPE_REPRESENTATION_RELATIONSHIP('SRR','None',#47762,#687);
#676=SHAPE_REPRESENTATION_RELATIONSHIP('SRR','None',#47763,#688);
#677=SHAPE_REPRESENTATION_RELATIONSHIP('SRR','None',#47764,#689);
#678=SHAPE_REPRESENTATION_RELATIONSHIP('SRR','None',#47765,#690);
#679=SHAPE_REPRESENTATION_RELATIONSHIP('SRR','None',#47766,#691);
#680=SHAPE_REPRESENTATION_RELATIONSHIP('SRR','None',#47767,#692);
#681=SHAPE_REPRESENTATION_RELATIONSHIP('SRR','None',#47768,#693);
#682=SHAPE_REPRESENTATION_RELATIONSHIP('SRR','None',#47769,#694);
#683=SHAPE_REPRESENTATION_RELATIONSHIP('SRR','None',#47770,#695);
#684=SHAPE_REPRESENTATION_RELATIONSHIP('SRR','None',#47771,#696);
#685=SHAPE_REPRESENTATION_RELATIONSHIP('SRR','None',#47772,#697);
#686=ADVANCED_BREP_SHAPE_REPRESENTATION('',(#710),#47705);
#687=ADVANCED_BREP_SHAPE_REPRESENTATION('',(#711),#47706);
#688=ADVANCED_BREP_SHAPE_REPRESENTATION('',(#712),#47707);
#689=ADVANCED_BREP_SHAPE_REPRESENTATION('',(#713),#47708);
#690=ADVANCED_BREP_SHAPE_REPRESENTATION('',(#714),#47709);
#691=ADVANCED_BREP_SHAPE_REPRESENTATION('',(#715),#47710);
#692=ADVANCED_BREP_SHAPE_REPRESENTATION('',(#716),#47711);
#693=ADVANCED_BREP_SHAPE_REPRESENTATION('',(#717),#47712);
#694=ADVANCED_BREP_SHAPE_REPRESENTATION('',(#718),#47713);
#695=ADVANCED_BREP_SHAPE_REPRESENTATION('',(#719),#47714);
#696=ADVANCED_BREP_SHAPE_REPRESENTATION('',(#720),#47715);
#697=ADVANCED_BREP_SHAPE_REPRESENTATION('',(#721),#47716);
#698=STYLED_ITEM('',(#47830),#710);
#699=STYLED_ITEM('',(#47830),#711);
#700=STYLED_ITEM('',(#47830),#712);
#701=STYLED_ITEM('',(#47830),#713);
#702=STYLED_ITEM('',(#47830),#714);
#703=STYLED_ITEM('',(#47830),#715);
#704=STYLED_ITEM('',(#47830),#716);
#705=STYLED_ITEM('',(#47830),#717);
#706=STYLED_ITEM('',(#47830),#718);
#707=STYLED_ITEM('',(#47830),#719);
#708=STYLED_ITEM('',(#47830),#720);
#709=STYLED_ITEM('',(#47830),#721);
#710=MANIFOLD_SOLID_BREP('Body1',#8925);
#711=MANIFOLD_SOLID_BREP('Body1',#8926);
#712=MANIFOLD_SOLID_BREP('Body1',#8927);
#713=MANIFOLD_SOLID_BREP('Body1',#8928);
#714=MANIFOLD_SOLID_BREP('Body1',#8929);
#715=MANIFOLD_SOLID_BREP('Body1',#8930);
#716=MANIFOLD_SOLID_BREP('Body1',#8931);
#717=MANIFOLD_SOLID_BREP('Body1',#8932);
#718=MANIFOLD_SOLID_BREP('Body1',#8933);
#719=MANIFOLD_SOLID_BREP('Body1',#8934);
#720=MANIFOLD_SOLID_BREP('Body1',#8935);
#721=MANIFOLD_SOLID_BREP('Body1',#8936);
#722=FACE_BOUND('',#2579,.T.);
#723=FACE_BOUND('',#2581,.T.);
#724=FACE_BOUND('',#2600,.T.);
#725=FACE_BOUND('',#2602,.T.);
#726=FACE_BOUND('',#2631,.T.);
#727=FACE_BOUND('',#2665,.T.);
#728=FACE_BOUND('',#2667,.T.);
#729=FACE_BOUND('',#2673,.T.);
#730=FACE_BOUND('',#2857,.T.);
#731=FACE_BOUND('',#2898,.T.);
#732=FACE_BOUND('',#2899,.T.);
#733=FACE_BOUND('',#2901,.T.);
#734=FACE_BOUND('',#2902,.T.);
#735=FACE_BOUND('',#2927,.T.);
#736=FACE_BOUND('',#2929,.T.);
#737=FACE_BOUND('',#2996,.T.);
#738=FACE_BOUND('',#2997,.T.);
#739=FACE_BOUND('',#2999,.T.);
#740=FACE_BOUND('',#3000,.T.);
#741=FACE_BOUND('',#3008,.T.);
#742=FACE_BOUND('',#3010,.T.);
#743=FACE_BOUND('',#3014,.T.);
#744=FACE_BOUND('',#3015,.T.);
#745=FACE_BOUND('',#3017,.T.);
#746=FACE_BOUND('',#3018,.T.);
#747=FACE_BOUND('',#3044,.T.);
#748=FACE_BOUND('',#3046,.T.);
#749=FACE_BOUND('',#3051,.T.);
#750=FACE_BOUND('',#3053,.T.);
#751=FACE_BOUND('',#3058,.T.);
#752=FACE_BOUND('',#3060,.T.);
#753=FACE_BOUND('',#3068,.T.);
#754=FACE_BOUND('',#3070,.T.);
#755=FACE_BOUND('',#3098,.T.);
#756=FACE_BOUND('',#3099,.T.);
#757=FACE_BOUND('',#3101,.T.);
#758=FACE_BOUND('',#3102,.T.);
#759=PLANE('',#9079);
#760=PLANE('',#9080);
#761=PLANE('',#9110);
#762=PLANE('',#9111);
#763=PLANE('',#9120);
#764=PLANE('',#9121);
#765=PLANE('',#9173);
#766=PLANE('',#9193);
#767=PLANE('',#9194);
#768=PLANE('',#9198);
#769=PLANE('',#9201);
#770=PLANE('',#9202);
#771=PLANE('',#9203);
#772=PLANE('',#9214);
#773=PLANE('',#9215);
#774=PLANE('',#9216);
#775=PLANE('',#9219);
#776=PLANE('',#9225);
#777=PLANE('',#9237);
#778=PLANE('',#9238);
#779=PLANE('',#9243);
#780=PLANE('',#9244);
#781=PLANE('',#9250);
#782=PLANE('',#9252);
#783=PLANE('',#9253);
#784=PLANE('',#9254);
#785=PLANE('',#9260);
#786=PLANE('',#9261);
#787=PLANE('',#9262);
#788=PLANE('',#9263);
#789=PLANE('',#9264);
#790=PLANE('',#9265);
#791=PLANE('',#9266);
#792=PLANE('',#9267);
#793=PLANE('',#9268);
#794=PLANE('',#9269);
#795=PLANE('',#9270);
#796=PLANE('',#9271);
#797=PLANE('',#9272);
#798=PLANE('',#9273);
#799=PLANE('',#9274);
#800=PLANE('',#9275);
#801=PLANE('',#9276);
#802=PLANE('',#9277);
#803=PLANE('',#9278);
#804=PLANE('',#9291);
#805=PLANE('',#9294);
#806=PLANE('',#9295);
#807=PLANE('',#9327);
#808=PLANE('',#9490);
#809=PLANE('',#9491);
#810=PLANE('',#9493);
#811=PLANE('',#9510);
#812=PLANE('',#9563);
#813=PLANE('',#9573);
#814=PLANE('',#9583);
#815=PLANE('',#9595);
#816=PLANE('',#9604);
#817=PLANE('',#9611);
#818=PLANE('',#9619);
#819=PLANE('',#9625);
#820=PLANE('',#9635);
#821=PLANE('',#9636);
#822=PLANE('',#9638);
#823=PLANE('',#9641);
#824=PLANE('',#9642);
#825=PLANE('',#9643);
#826=PLANE('',#9644);
#827=PLANE('',#9645);
#828=PLANE('',#9646);
#829=PLANE('',#9647);
#830=PLANE('',#9648);
#831=PLANE('',#9649);
#832=PLANE('',#9650);
#833=PLANE('',#9651);
#834=PLANE('',#9652);
#835=PLANE('',#9653);
#836=PLANE('',#9654);
#837=PLANE('',#9655);
#838=PLANE('',#9656);
#839=PLANE('',#9657);
#840=PLANE('',#9658);
#841=PLANE('',#9659);
#842=PLANE('',#9742);
#843=PLANE('',#9743);
#844=PLANE('',#9744);
#845=PLANE('',#9745);
#846=PLANE('',#9747);
#847=PLANE('',#9750);
#848=PLANE('',#9753);
#849=PLANE('',#9757);
#850=PLANE('',#9758);
#851=PLANE('',#9759);
#852=PLANE('',#9761);
#853=PLANE('',#9764);
#854=PLANE('',#9766);
#855=PLANE('',#9768);
#856=PLANE('',#9771);
#857=PLANE('',#9774);
#858=PLANE('',#9777);
#859=PLANE('',#9780);
#860=PLANE('',#9782);
#861=PLANE('',#9783);
#862=PLANE('',#9784);
#863=PLANE('',#9785);
#864=PLANE('',#9786);
#865=PLANE('',#9787);
#866=PLANE('',#9809);
#867=PLANE('',#9810);
#868=PLANE('',#9811);
#869=PLANE('',#9822);
#870=PLANE('',#9823);
#871=PLANE('',#9832);
#872=PLANE('',#9833);
#873=PLANE('',#9848);
#874=PLANE('',#9852);
#875=PLANE('',#9855);
#876=PLANE('',#9859);
#877=PLANE('',#9860);
#878=PLANE('',#9901);
#879=PLANE('',#9906);
#880=PLANE('',#9911);
#881=PLANE('',#9915);
#882=PLANE('',#9919);
#883=LINE('',#12224,#1370);
#884=LINE('',#12260,#1371);
#885=LINE('',#14184,#1372);
#886=LINE('',#15682,#1373);
#887=LINE('',#15695,#1374);
#888=LINE('',#15699,#1375);
#889=LINE('',#15703,#1376);
#890=LINE('',#15719,#1377);
#891=LINE('',#15862,#1378);
#892=LINE('',#15868,#1379);
#893=LINE('',#15883,#1380);
#894=LINE('',#15886,#1381);
#895=LINE('',#15892,#1382);
#896=LINE('',#15905,#1383);
#897=LINE('',#15922,#1384);
#898=LINE('',#15937,#1385);
#899=LINE('',#15941,#1386);
#900=LINE('',#16174,#1387);
#901=LINE('',#16178,#1388);
#902=LINE('',#16210,#1389);
#903=LINE('',#16245,#1390);
#904=LINE('',#16277,#1391);
#905=LINE('',#16312,#1392);
#906=LINE('',#16334,#1393);
#907=LINE('',#16349,#1394);
#908=LINE('',#16361,#1395);
#909=LINE('',#16376,#1396);
#910=LINE('',#16388,#1397);
#911=LINE('',#16403,#1398);
#912=LINE('',#16415,#1399);
#913=LINE('',#16430,#1400);
#914=LINE('',#16442,#1401);
#915=LINE('',#16457,#1402);
#916=LINE('',#16469,#1403);
#917=LINE('',#16484,#1404);
#918=LINE('',#16496,#1405);
#919=LINE('',#16511,#1406);
#920=LINE('',#16523,#1407);
#921=LINE('',#17082,#1408);
#922=LINE('',#17084,#1409);
#923=LINE('',#17102,#1410);
#924=LINE('',#17120,#1411);
#925=LINE('',#17138,#1412);
#926=LINE('',#17156,#1413);
#927=LINE('',#17174,#1414);
#928=LINE('',#17192,#1415);
#929=LINE('',#17208,#1416);
#930=LINE('',#17210,#1417);
#931=LINE('',#17214,#1418);
#932=LINE('',#17217,#1419);
#933=LINE('',#17288,#1420);
#934=LINE('',#17585,#1421);
#935=LINE('',#17630,#1422);
#936=LINE('',#17677,#1423);
#937=LINE('',#17724,#1424);
#938=LINE('',#17773,#1425);
#939=LINE('',#17824,#1426);
#940=LINE('',#18047,#1427);
#941=LINE('',#18336,#1428);
#942=LINE('',#18342,#1429);
#943=LINE('',#18377,#1430);
#944=LINE('',#18379,#1431);
#945=LINE('',#18381,#1432);
#946=LINE('',#18384,#1433);
#947=LINE('',#18423,#1434);
#948=LINE('',#18426,#1435);
#949=LINE('',#18428,#1436);
#950=LINE('',#18429,#1437);
#951=LINE('',#18433,#1438);
#952=LINE('',#18435,#1439);
#953=LINE('',#18437,#1440);
#954=LINE('',#18438,#1441);
#955=LINE('',#18461,#1442);
#956=LINE('',#18465,#1443);
#957=LINE('',#18469,#1444);
#958=LINE('',#18473,#1445);
#959=LINE('',#18477,#1446);
#960=LINE('',#18502,#1447);
#961=LINE('',#18507,#1448);
#962=LINE('',#18511,#1449);
#963=LINE('',#18549,#1450);
#964=LINE('',#18579,#1451);
#965=LINE('',#18580,#1452);
#966=LINE('',#18582,#1453);
#967=LINE('',#18583,#1454);
#968=LINE('',#18672,#1455);
#969=LINE('',#18676,#1456);
#970=LINE('',#18679,#1457);
#971=LINE('',#18682,#1458);
#972=LINE('',#18686,#1459);
#973=LINE('',#18690,#1460);
#974=LINE('',#19155,#1461);
#975=LINE('',#19161,#1462);
#976=LINE('',#19162,#1463);
#977=LINE('',#19269,#1464);
#978=LINE('',#19270,#1465);
#979=LINE('',#19339,#1466);
#980=LINE('',#19343,#1467);
#981=LINE('',#19447,#1468);
#982=LINE('',#19462,#1469);
#983=LINE('',#19463,#1470);
#984=LINE('',#19467,#1471);
#985=LINE('',#19468,#1472);
#986=LINE('',#19469,#1473);
#987=LINE('',#19529,#1474);
#988=LINE('',#19589,#1475);
#989=LINE('',#19606,#1476);
#990=LINE('',#19616,#1477);
#991=LINE('',#19618,#1478);
#992=LINE('',#19620,#1479);
#993=LINE('',#19622,#1480);
#994=LINE('',#19624,#1481);
#995=LINE('',#19626,#1482);
#996=LINE('',#19628,#1483);
#997=LINE('',#19630,#1484);
#998=LINE('',#19632,#1485);
#999=LINE('',#19634,#1486);
#1000=LINE('',#19636,#1487);
#1001=LINE('',#19638,#1488);
#1002=LINE('',#19640,#1489);
#1003=LINE('',#19642,#1490);
#1004=LINE('',#19644,#1491);
#1005=LINE('',#19646,#1492);
#1006=LINE('',#19648,#1493);
#1007=LINE('',#19650,#1494);
#1008=LINE('',#19651,#1495);
#1009=LINE('',#19654,#1496);
#1010=LINE('',#19655,#1497);
#1011=LINE('',#19659,#1498);
#1012=LINE('',#19660,#1499);
#1013=LINE('',#19661,#1500);
#1014=LINE('',#19678,#1501);
#1015=LINE('',#19680,#1502);
#1016=LINE('',#19682,#1503);
#1017=LINE('',#19684,#1504);
#1018=LINE('',#19686,#1505);
#1019=LINE('',#19688,#1506);
#1020=LINE('',#19690,#1507);
#1021=LINE('',#19692,#1508);
#1022=LINE('',#19694,#1509);
#1023=LINE('',#19696,#1510);
#1024=LINE('',#19698,#1511);
#1025=LINE('',#19700,#1512);
#1026=LINE('',#19702,#1513);
#1027=LINE('',#19704,#1514);
#1028=LINE('',#19706,#1515);
#1029=LINE('',#19708,#1516);
#1030=LINE('',#19710,#1517);
#1031=LINE('',#19712,#1518);
#1032=LINE('',#19713,#1519);
#1033=LINE('',#19749,#1520);
#1034=LINE('',#19751,#1521);
#1035=LINE('',#19753,#1522);
#1036=LINE('',#19755,#1523);
#1037=LINE('',#19757,#1524);
#1038=LINE('',#19759,#1525);
#1039=LINE('',#19761,#1526);
#1040=LINE('',#19763,#1527);
#1041=LINE('',#19765,#1528);
#1042=LINE('',#19767,#1529);
#1043=LINE('',#19769,#1530);
#1044=LINE('',#19771,#1531);
#1045=LINE('',#19773,#1532);
#1046=LINE('',#19775,#1533);
#1047=LINE('',#19777,#1534);
#1048=LINE('',#19779,#1535);
#1049=LINE('',#19781,#1536);
#1050=LINE('',#19783,#1537);
#1051=LINE('',#32346,#1538);
#1052=LINE('',#32362,#1539);
#1053=LINE('',#32436,#1540);
#1054=LINE('',#32512,#1541);
#1055=LINE('',#32588,#1542);
#1056=LINE('',#32664,#1543);
#1057=LINE('',#32740,#1544);
#1058=LINE('',#32816,#1545);
#1059=LINE('',#32892,#1546);
#1060=LINE('',#32968,#1547);
#1061=LINE('',#33044,#1548);
#1062=LINE('',#33120,#1549);
#1063=LINE('',#33196,#1550);
#1064=LINE('',#33272,#1551);
#1065=LINE('',#33348,#1552);
#1066=LINE('',#33424,#1553);
#1067=LINE('',#33500,#1554);
#1068=LINE('',#33576,#1555);
#1069=LINE('',#33652,#1556);
#1070=LINE('',#33728,#1557);
#1071=LINE('',#33804,#1558);
#1072=LINE('',#33880,#1559);
#1073=LINE('',#33956,#1560);
#1074=LINE('',#34032,#1561);
#1075=LINE('',#34108,#1562);
#1076=LINE('',#34184,#1563);
#1077=LINE('',#34260,#1564);
#1078=LINE('',#34336,#1565);
#1079=LINE('',#34412,#1566);
#1080=LINE('',#34488,#1567);
#1081=LINE('',#34564,#1568);
#1082=LINE('',#34640,#1569);
#1083=LINE('',#34716,#1570);
#1084=LINE('',#34792,#1571);
#1085=LINE('',#34868,#1572);
#1086=LINE('',#34944,#1573);
#1087=LINE('',#35020,#1574);
#1088=LINE('',#35096,#1575);
#1089=LINE('',#35172,#1576);
#1090=LINE('',#35248,#1577);
#1091=LINE('',#35324,#1578);
#1092=LINE('',#35399,#1579);
#1093=LINE('',#35438,#1580);
#1094=LINE('',#35472,#1581);
#1095=LINE('',#35509,#1582);
#1096=LINE('',#35543,#1583);
#1097=LINE('',#35580,#1584);
#1098=LINE('',#35614,#1585);
#1099=LINE('',#35651,#1586);
#1100=LINE('',#35685,#1587);
#1101=LINE('',#35722,#1588);
#1102=LINE('',#35756,#1589);
#1103=LINE('',#35793,#1590);
#1104=LINE('',#35827,#1591);
#1105=LINE('',#35864,#1592);
#1106=LINE('',#35898,#1593);
#1107=LINE('',#35935,#1594);
#1108=LINE('',#35969,#1595);
#1109=LINE('',#36006,#1596);
#1110=LINE('',#36040,#1597);
#1111=LINE('',#36077,#1598);
#1112=LINE('',#36111,#1599);
#1113=LINE('',#37277,#1600);
#1114=LINE('',#37287,#1601);
#1115=LINE('',#37289,#1602);
#1116=LINE('',#37290,#1603);
#1117=LINE('',#37292,#1604);
#1118=LINE('',#37293,#1605);
#1119=LINE('',#37295,#1606);
#1120=LINE('',#37296,#1607);
#1121=LINE('',#37298,#1608);
#1122=LINE('',#37299,#1609);
#1123=LINE('',#37301,#1610);
#1124=LINE('',#37302,#1611);
#1125=LINE('',#37304,#1612);
#1126=LINE('',#37305,#1613);
#1127=LINE('',#37307,#1614);
#1128=LINE('',#37308,#1615);
#1129=LINE('',#37310,#1616);
#1130=LINE('',#37311,#1617);
#1131=LINE('',#37313,#1618);
#1132=LINE('',#37314,#1619);
#1133=LINE('',#37316,#1620);
#1134=LINE('',#37317,#1621);
#1135=LINE('',#37319,#1622);
#1136=LINE('',#37320,#1623);
#1137=LINE('',#37322,#1624);
#1138=LINE('',#37323,#1625);
#1139=LINE('',#37325,#1626);
#1140=LINE('',#37326,#1627);
#1141=LINE('',#37328,#1628);
#1142=LINE('',#37329,#1629);
#1143=LINE('',#37369,#1630);
#1144=LINE('',#37370,#1631);
#1145=LINE('',#44352,#1632);
#1146=LINE('',#44377,#1633);
#1147=LINE('',#44383,#1634);
#1148=LINE('',#44389,#1635);
#1149=LINE('',#44463,#1636);
#1150=LINE('',#44466,#1637);
#1151=LINE('',#44468,#1638);
#1152=LINE('',#44469,#1639);
#1153=LINE('',#44475,#1640);
#1154=LINE('',#44478,#1641);
#1155=LINE('',#44529,#1642);
#1156=LINE('',#44574,#1643);
#1157=LINE('',#44580,#1644);
#1158=LINE('',#44583,#1645);
#1159=LINE('',#44587,#1646);
#1160=LINE('',#44591,#1647);
#1161=LINE('',#44606,#1648);
#1162=LINE('',#44622,#1649);
#1163=LINE('',#44632,#1650);
#1164=LINE('',#44634,#1651);
#1165=LINE('',#44636,#1652);
#1166=LINE('',#44638,#1653);
#1167=LINE('',#44640,#1654);
#1168=LINE('',#44641,#1655);
#1169=LINE('',#44646,#1656);
#1170=LINE('',#44650,#1657);
#1171=LINE('',#44654,#1658);
#1172=LINE('',#44659,#1659);
#1173=LINE('',#44663,#1660);
#1174=LINE('',#44670,#1661);
#1175=LINE('',#44672,#1662);
#1176=LINE('',#44673,#1663);
#1177=LINE('',#44720,#1664);
#1178=LINE('',#44791,#1665);
#1179=LINE('',#44793,#1666);
#1180=LINE('',#44795,#1667);
#1181=LINE('',#44797,#1668);
#1182=LINE('',#44799,#1669);
#1183=LINE('',#44801,#1670);
#1184=LINE('',#44803,#1671);
#1185=LINE('',#44805,#1672);
#1186=LINE('',#44807,#1673);
#1187=LINE('',#44809,#1674);
#1188=LINE('',#44811,#1675);
#1189=LINE('',#44813,#1676);
#1190=LINE('',#44815,#1677);
#1191=LINE('',#44817,#1678);
#1192=LINE('',#44818,#1679);
#1193=LINE('',#44820,#1680);
#1194=LINE('',#44821,#1681);
#1195=LINE('',#44823,#1682);
#1196=LINE('',#44824,#1683);
#1197=LINE('',#44827,#1684);
#1198=LINE('',#44829,#1685);
#1199=LINE('',#44854,#1686);
#1200=LINE('',#44863,#1687);
#1201=LINE('',#44872,#1688);
#1202=LINE('',#44890,#1689);
#1203=LINE('',#44891,#1690);
#1204=LINE('',#44893,#1691);
#1205=LINE('',#44894,#1692);
#1206=LINE('',#44896,#1693);
#1207=LINE('',#44898,#1694);
#1208=LINE('',#44900,#1695);
#1209=LINE('',#44902,#1696);
#1210=LINE('',#44904,#1697);
#1211=LINE('',#44906,#1698);
#1212=LINE('',#44908,#1699);
#1213=LINE('',#44910,#1700);
#1214=LINE('',#44912,#1701);
#1215=LINE('',#44914,#1702);
#1216=LINE('',#44916,#1703);
#1217=LINE('',#44918,#1704);
#1218=LINE('',#44920,#1705);
#1219=LINE('',#44921,#1706);
#1220=LINE('',#45010,#1707);
#1221=LINE('',#45012,#1708);
#1222=LINE('',#45013,#1709);
#1223=LINE('',#45016,#1710);
#1224=LINE('',#45021,#1711);
#1225=LINE('',#45023,#1712);
#1226=LINE('',#45026,#1713);
#1227=LINE('',#45027,#1714);
#1228=LINE('',#45030,#1715);
#1229=LINE('',#45032,#1716);
#1230=LINE('',#45033,#1717);
#1231=LINE('',#45035,#1718);
#1232=LINE('',#45036,#1719);
#1233=LINE('',#45038,#1720);
#1234=LINE('',#45039,#1721);
#1235=LINE('',#45041,#1722);
#1236=LINE('',#45042,#1723);
#1237=LINE('',#45044,#1724);
#1238=LINE('',#45045,#1725);
#1239=LINE('',#45053,#1726);
#1240=LINE('',#45056,#1727);
#1241=LINE('',#45427,#1728);
#1242=LINE('',#45430,#1729);
#1243=LINE('',#45435,#1730);
#1244=LINE('',#45441,#1731);
#1245=LINE('',#45447,#1732);
#1246=LINE('',#45451,#1733);
#1247=LINE('',#45454,#1734);
#1248=LINE('',#45459,#1735);
#1249=LINE('',#45465,#1736);
#1250=LINE('',#45471,#1737);
#1251=LINE('',#45477,#1738);
#1252=LINE('',#45478,#1739);
#1253=LINE('',#45480,#1740);
#1254=LINE('',#45481,#1741);
#1255=LINE('',#45484,#1742);
#1256=LINE('',#45485,#1743);
#1257=LINE('',#45488,#1744);
#1258=LINE('',#45489,#1745);
#1259=LINE('',#45492,#1746);
#1260=LINE('',#45494,#1747);
#1261=LINE('',#45495,#1748);
#1262=LINE('',#45499,#1749);
#1263=LINE('',#45501,#1750);
#1264=LINE('',#45503,#1751);
#1265=LINE('',#45505,#1752);
#1266=LINE('',#45506,#1753);
#1267=LINE('',#45511,#1754);
#1268=LINE('',#45513,#1755);
#1269=LINE('',#45515,#1756);
#1270=LINE('',#45517,#1757);
#1271=LINE('',#45519,#1758);
#1272=LINE('',#45522,#1759);
#1273=LINE('',#45526,#1760);
#1274=LINE('',#45530,#1761);
#1275=LINE('',#45532,#1762);
#1276=LINE('',#45534,#1763);
#1277=LINE('',#45536,#1764);
#1278=LINE('',#45537,#1765);
#1279=LINE('',#45541,#1766);
#1280=LINE('',#45543,#1767);
#1281=LINE('',#45545,#1768);
#1282=LINE('',#45546,#1769);
#1283=LINE('',#45551,#1770);
#1284=LINE('',#45554,#1771);
#1285=LINE('',#45555,#1772);
#1286=LINE('',#45559,#1773);
#1287=LINE('',#45560,#1774);
#1288=LINE('',#45561,#1775);
#1289=LINE('',#45565,#1776);
#1290=LINE('',#45567,#1777);
#1291=LINE('',#45569,#1778);
#1292=LINE('',#45572,#1779);
#1293=LINE('',#45573,#1780);
#1294=LINE('',#45577,#1781);
#1295=LINE('',#45583,#1782);
#1296=LINE('',#45585,#1783);
#1297=LINE('',#45588,#1784);
#1298=LINE('',#45593,#1785);
#1299=LINE('',#45594,#1786);
#1300=LINE('',#45601,#1787);
#1301=LINE('',#45603,#1788);
#1302=LINE('',#45605,#1789);
#1303=LINE('',#45611,#1790);
#1304=LINE('',#45615,#1791);
#1305=LINE('',#45616,#1792);
#1306=LINE('',#45620,#1793);
#1307=LINE('',#45622,#1794);
#1308=LINE('',#45625,#1795);
#1309=LINE('',#45628,#1796);
#1310=LINE('',#45630,#1797);
#1311=LINE('',#45632,#1798);
#1312=LINE('',#45634,#1799);
#1313=LINE('',#45635,#1800);
#1314=LINE('',#45636,#1801);
#1315=LINE('',#45638,#1802);
#1316=LINE('',#45641,#1803);
#1317=LINE('',#45644,#1804);
#1318=LINE('',#45645,#1805);
#1319=LINE('',#45646,#1806);
#1320=LINE('',#45649,#1807);
#1321=LINE('',#45650,#1808);
#1322=LINE('',#45653,#1809);
#1323=LINE('',#45852,#1810);
#1324=LINE('',#45870,#1811);
#1325=LINE('',#45874,#1812);
#1326=LINE('',#45891,#1813);
#1327=LINE('',#45894,#1814);
#1328=LINE('',#45895,#1815);
#1329=LINE('',#45913,#1816);
#1330=LINE('',#45925,#1817);
#1331=LINE('',#45937,#1818);
#1332=LINE('',#45948,#1819);
#1333=LINE('',#45950,#1820);
#1334=LINE('',#45952,#1821);
#1335=LINE('',#46016,#1822);
#1336=LINE('',#46087,#1823);
#1337=LINE('',#46095,#1824);
#1338=LINE('',#46097,#1825);
#1339=LINE('',#46099,#1826);
#1340=LINE('',#46100,#1827);
#1341=LINE('',#46129,#1828);
#1342=LINE('',#46137,#1829);
#1343=LINE('',#46157,#1830);
#1344=LINE('',#46251,#1831);
#1345=LINE('',#46398,#1832);
#1346=LINE('',#46413,#1833);
#1347=LINE('',#46649,#1834);
#1348=LINE('',#47457,#1835);
#1349=LINE('',#47459,#1836);
#1350=LINE('',#47461,#1837);
#1351=LINE('',#47462,#1838);
#1352=LINE('',#47469,#1839);
#1353=LINE('',#47473,#1840);
#1354=LINE('',#47476,#1841);
#1355=LINE('',#47481,#1842);
#1356=LINE('',#47487,#1843);
#1357=LINE('',#47490,#1844);
#1358=LINE('',#47494,#1845);
#1359=LINE('',#47495,#1846);
#1360=LINE('',#47496,#1847);
#1361=LINE('',#47500,#1848);
#1362=LINE('',#47506,#1849);
#1363=LINE('',#47507,#1850);
#1364=LINE('',#47508,#1851);
#1365=LINE('',#47512,#1852);
#1366=LINE('',#47518,#1853);
#1367=LINE('',#47519,#1854);
#1368=LINE('',#47520,#1855);
#1369=LINE('',#47524,#1856);
#1370=VECTOR('',#9968,2.);
#1371=VECTOR('',#10017,0.400000000000003);
#1372=VECTOR('',#10032,0.400000000000011);
#1373=VECTOR('',#10053,2.);
#1374=VECTOR('',#10070,1000.);
#1375=VECTOR('',#10073,1000.);
#1376=VECTOR('',#10076,1000.);
#1377=VECTOR('',#10079,1000.);
#1378=VECTOR('',#10124,2.);
#1379=VECTOR('',#10131,2.);
#1380=VECTOR('',#10138,1000.);
#1381=VECTOR('',#10141,1000.);
#1382=VECTOR('',#10146,1000.);
#1383=VECTOR('',#10149,1000.);
#1384=VECTOR('',#10152,1000.);
#1385=VECTOR('',#10153,1000.);
#1386=VECTOR('',#10156,1000.);
#1387=VECTOR('',#10157,1000.);
#1388=VECTOR('',#10160,1000.);
#1389=VECTOR('',#10161,1000.);
#1390=VECTOR('',#10164,1000.);
#1391=VECTOR('',#10165,1000.);
#1392=VECTOR('',#10168,1000.);
#1393=VECTOR('',#10171,1000.);
#1394=VECTOR('',#10174,1000.);
#1395=VECTOR('',#10175,10.);
#1396=VECTOR('',#10178,1000.);
#1397=VECTOR('',#10179,10.);
#1398=VECTOR('',#10182,1000.);
#1399=VECTOR('',#10183,10.);
#1400=VECTOR('',#10186,1000.);
#1401=VECTOR('',#10187,10.);
#1402=VECTOR('',#10190,1000.);
#1403=VECTOR('',#10191,10.);
#1404=VECTOR('',#10194,1000.);
#1405=VECTOR('',#10195,10.);
#1406=VECTOR('',#10198,1000.);
#1407=VECTOR('',#10199,10.);
#1408=VECTOR('',#10204,1000.);
#1409=VECTOR('',#10205,1000.);
#1410=VECTOR('',#10208,1000.);
#1411=VECTOR('',#10211,1000.);
#1412=VECTOR('',#10214,1000.);
#1413=VECTOR('',#10217,1000.);
#1414=VECTOR('',#10220,1000.);
#1415=VECTOR('',#10223,1000.);
#1416=VECTOR('',#10224,1000.);
#1417=VECTOR('',#10225,1000.);
#1418=VECTOR('',#10228,1000.);
#1419=VECTOR('',#10231,1000.);
#1420=VECTOR('',#10232,1000.);
#1421=VECTOR('',#10237,10.);
#1422=VECTOR('',#10238,10.);
#1423=VECTOR('',#10239,10.);
#1424=VECTOR('',#10240,10.);
#1425=VECTOR('',#10241,10.);
#1426=VECTOR('',#10242,10.);
#1427=VECTOR('',#10261,1000.);
#1428=VECTOR('',#10264,1000.);
#1429=VECTOR('',#10271,1000.);
#1430=VECTOR('',#10274,1000.);
#1431=VECTOR('',#10277,1000.);
#1432=VECTOR('',#10278,1000.);
#1433=VECTOR('',#10281,1000.);
#1434=VECTOR('',#10282,1000.);
#1435=VECTOR('',#10285,1000.);
#1436=VECTOR('',#10286,1000.);
#1437=VECTOR('',#10287,1000.);
#1438=VECTOR('',#10290,1000.);
#1439=VECTOR('',#10291,1000.);
#1440=VECTOR('',#10292,1000.);
#1441=VECTOR('',#10293,1000.);
#1442=VECTOR('',#10296,1000.);
#1443=VECTOR('',#10299,1000.);
#1444=VECTOR('',#10302,1000.);
#1445=VECTOR('',#10305,1000.);
#1446=VECTOR('',#10308,1000.);
#1447=VECTOR('',#10313,1000.);
#1448=VECTOR('',#10318,1000.);
#1449=VECTOR('',#10321,1000.);
#1450=VECTOR('',#10324,1000.);
#1451=VECTOR('',#10327,1000.);
#1452=VECTOR('',#10328,1000.);
#1453=VECTOR('',#10331,1000.);
#1454=VECTOR('',#10332,1000.);
#1455=VECTOR('',#10335,1000.);
#1456=VECTOR('',#10338,1000.);
#1457=VECTOR('',#10341,1000.);
#1458=VECTOR('',#10344,1000.);
#1459=VECTOR('',#10347,1000.);
#1460=VECTOR('',#10350,1000.);
#1461=VECTOR('',#10357,10.);
#1462=VECTOR('',#10366,1000.);
#1463=VECTOR('',#10367,1000.);
#1464=VECTOR('',#10382,1000.);
#1465=VECTOR('',#10383,1000.);
#1466=VECTOR('',#10396,1000.);
#1467=VECTOR('',#10399,1000.);
#1468=VECTOR('',#10402,1000.);
#1469=VECTOR('',#10403,1000.);
#1470=VECTOR('',#10404,1000.);
#1471=VECTOR('',#10407,1000.);
#1472=VECTOR('',#10408,1000.);
#1473=VECTOR('',#10409,1000.);
#1474=VECTOR('',#10416,1000.);
#1475=VECTOR('',#10421,1000.);
#1476=VECTOR('',#10424,1000.);
#1477=VECTOR('',#10427,1000.);
#1478=VECTOR('',#10428,1000.);
#1479=VECTOR('',#10429,1000.);
#1480=VECTOR('',#10430,1000.);
#1481=VECTOR('',#10431,1000.);
#1482=VECTOR('',#10432,1000.);
#1483=VECTOR('',#10433,1000.);
#1484=VECTOR('',#10434,1000.);
#1485=VECTOR('',#10435,1000.);
#1486=VECTOR('',#10436,1000.);
#1487=VECTOR('',#10437,1000.);
#1488=VECTOR('',#10438,1000.);
#1489=VECTOR('',#10439,1000.);
#1490=VECTOR('',#10440,1000.);
#1491=VECTOR('',#10441,1000.);
#1492=VECTOR('',#10442,1000.);
#1493=VECTOR('',#10443,1000.);
#1494=VECTOR('',#10444,1000.);
#1495=VECTOR('',#10445,1000.);
#1496=VECTOR('',#10448,1000.);
#1497=VECTOR('',#10449,1000.);
#1498=VECTOR('',#10452,1000.);
#1499=VECTOR('',#10453,1000.);
#1500=VECTOR('',#10454,1000.);
#1501=VECTOR('',#10457,1000.);
#1502=VECTOR('',#10458,1000.);
#1503=VECTOR('',#10459,1000.);
#1504=VECTOR('',#10460,1000.);
#1505=VECTOR('',#10461,1000.);
#1506=VECTOR('',#10462,1000.);
#1507=VECTOR('',#10463,1000.);
#1508=VECTOR('',#10464,1000.);
#1509=VECTOR('',#10465,1000.);
#1510=VECTOR('',#10466,1000.);
#1511=VECTOR('',#10467,1000.);
#1512=VECTOR('',#10468,1000.);
#1513=VECTOR('',#10469,1000.);
#1514=VECTOR('',#10470,1000.);
#1515=VECTOR('',#10471,1000.);
#1516=VECTOR('',#10472,1000.);
#1517=VECTOR('',#10473,1000.);
#1518=VECTOR('',#10474,1000.);
#1519=VECTOR('',#10475,1000.);
#1520=VECTOR('',#10488,1000.);
#1521=VECTOR('',#10491,1000.);
#1522=VECTOR('',#10494,1000.);
#1523=VECTOR('',#10497,1000.);
#1524=VECTOR('',#10500,1000.);
#1525=VECTOR('',#10503,1000.);
#1526=VECTOR('',#10506,1000.);
#1527=VECTOR('',#10509,1000.);
#1528=VECTOR('',#10512,1000.);
#1529=VECTOR('',#10515,1000.);
#1530=VECTOR('',#10518,1000.);
#1531=VECTOR('',#10521,1000.);
#1532=VECTOR('',#10524,1000.);
#1533=VECTOR('',#10527,1000.);
#1534=VECTOR('',#10530,1000.);
#1535=VECTOR('',#10533,1000.);
#1536=VECTOR('',#10536,1000.);
#1537=VECTOR('',#10539,1000.);
#1538=VECTOR('',#10678,2.99999999999999);
#1539=VECTOR('',#10683,2.99999999999999);
#1540=VECTOR('',#10688,2.99999999999999);
#1541=VECTOR('',#10691,2.99999999999999);
#1542=VECTOR('',#10694,2.99999999999999);
#1543=VECTOR('',#10697,2.99999999999999);
#1544=VECTOR('',#10700,2.99999999999999);
#1545=VECTOR('',#10703,2.99999999999999);
#1546=VECTOR('',#10706,2.99999999999999);
#1547=VECTOR('',#10709,2.99999999999999);
#1548=VECTOR('',#10712,2.99999999999999);
#1549=VECTOR('',#10715,2.99999999999999);
#1550=VECTOR('',#10718,2.99999999999999);
#1551=VECTOR('',#10721,2.99999999999999);
#1552=VECTOR('',#10724,2.99999999999999);
#1553=VECTOR('',#10727,2.99999999999999);
#1554=VECTOR('',#10730,2.99999999999999);
#1555=VECTOR('',#10733,2.99999999999999);
#1556=VECTOR('',#10736,2.99999999999999);
#1557=VECTOR('',#10739,2.99999999999999);
#1558=VECTOR('',#10742,2.99999999999999);
#1559=VECTOR('',#10745,2.99999999999999);
#1560=VECTOR('',#10748,2.99999999999999);
#1561=VECTOR('',#10751,2.99999999999999);
#1562=VECTOR('',#10754,2.99999999999999);
#1563=VECTOR('',#10757,2.99999999999999);
#1564=VECTOR('',#10760,2.99999999999999);
#1565=VECTOR('',#10763,2.99999999999999);
#1566=VECTOR('',#10766,2.99999999999999);
#1567=VECTOR('',#10769,2.99999999999999);
#1568=VECTOR('',#10772,2.99999999999999);
#1569=VECTOR('',#10775,2.99999999999999);
#1570=VECTOR('',#10778,2.99999999999999);
#1571=VECTOR('',#10781,2.99999999999999);
#1572=VECTOR('',#10784,2.99999999999999);
#1573=VECTOR('',#10787,2.99999999999999);
#1574=VECTOR('',#10790,2.99999999999999);
#1575=VECTOR('',#10793,2.99999999999999);
#1576=VECTOR('',#10796,2.99999999999999);
#1577=VECTOR('',#10799,2.99999999999999);
#1578=VECTOR('',#10802,2.99999999999999);
#1579=VECTOR('',#10809,2.99999999999999);
#1580=VECTOR('',#10816,1000.);
#1581=VECTOR('',#10817,1000.);
#1582=VECTOR('',#10820,1000.);
#1583=VECTOR('',#10821,1000.);
#1584=VECTOR('',#10824,1000.);
#1585=VECTOR('',#10825,1000.);
#1586=VECTOR('',#10828,1000.);
#1587=VECTOR('',#10829,1000.);
#1588=VECTOR('',#10832,1000.);
#1589=VECTOR('',#10833,1000.);
#1590=VECTOR('',#10836,1000.);
#1591=VECTOR('',#10837,1000.);
#1592=VECTOR('',#10840,1000.);
#1593=VECTOR('',#10841,1000.);
#1594=VECTOR('',#10844,1000.);
#1595=VECTOR('',#10845,1000.);
#1596=VECTOR('',#10848,1000.);
#1597=VECTOR('',#10849,1000.);
#1598=VECTOR('',#10852,1000.);
#1599=VECTOR('',#10853,1000.);
#1600=VECTOR('',#10980,1000.);
#1601=VECTOR('',#10999,1000.);
#1602=VECTOR('',#11002,1000.);
#1603=VECTOR('',#11003,1000.);
#1604=VECTOR('',#11006,1000.);
#1605=VECTOR('',#11007,1000.);
#1606=VECTOR('',#11010,1000.);
#1607=VECTOR('',#11011,1000.);
#1608=VECTOR('',#11014,1000.);
#1609=VECTOR('',#11015,1000.);
#1610=VECTOR('',#11018,1000.);
#1611=VECTOR('',#11019,1000.);
#1612=VECTOR('',#11022,1000.);
#1613=VECTOR('',#11023,1000.);
#1614=VECTOR('',#11026,1000.);
#1615=VECTOR('',#11027,1000.);
#1616=VECTOR('',#11030,1000.);
#1617=VECTOR('',#11031,1000.);
#1618=VECTOR('',#11034,1000.);
#1619=VECTOR('',#11035,1000.);
#1620=VECTOR('',#11038,1000.);
#1621=VECTOR('',#11039,1000.);
#1622=VECTOR('',#11042,1000.);
#1623=VECTOR('',#11043,1000.);
#1624=VECTOR('',#11046,1000.);
#1625=VECTOR('',#11047,1000.);
#1626=VECTOR('',#11050,1000.);
#1627=VECTOR('',#11051,1000.);
#1628=VECTOR('',#11054,1000.);
#1629=VECTOR('',#11055,1000.);
#1630=VECTOR('',#11062,1000.);
#1631=VECTOR('',#11063,1000.);
#1632=VECTOR('',#11106,2.);
#1633=VECTOR('',#11135,1.5);
#1634=VECTOR('',#11142,2.00000000000001);
#1635=VECTOR('',#11149,2.);
#1636=VECTOR('',#11172,1000.);
#1637=VECTOR('',#11175,1000.);
#1638=VECTOR('',#11178,1000.);
#1639=VECTOR('',#11179,1000.);
#1640=VECTOR('',#11184,1000.);
#1641=VECTOR('',#11187,1000.);
#1642=VECTOR('',#11196,1000.);
#1643=VECTOR('',#11203,1000.);
#1644=VECTOR('',#11208,1000.);
#1645=VECTOR('',#11211,1000.);
#1646=VECTOR('',#11214,1000.);
#1647=VECTOR('',#11217,1000.);
#1648=VECTOR('',#11234,1000.);
#1649=VECTOR('',#11251,1000.);
#1650=VECTOR('',#11264,1000.);
#1651=VECTOR('',#11265,1000.);
#1652=VECTOR('',#11266,1000.);
#1653=VECTOR('',#11267,1000.);
#1654=VECTOR('',#11268,1000.);
#1655=VECTOR('',#11269,1000.);
#1656=VECTOR('',#11274,1000.);
#1657=VECTOR('',#11277,1000.);
#1658=VECTOR('',#11280,1000.);
#1659=VECTOR('',#11285,1000.);
#1660=VECTOR('',#11288,1000.);
#1661=VECTOR('',#11299,1000.);
#1662=VECTOR('',#11300,1000.);
#1663=VECTOR('',#11301,1000.);
#1664=VECTOR('',#11308,1000.);
#1665=VECTOR('',#11327,1000.);
#1666=VECTOR('',#11328,1000.);
#1667=VECTOR('',#11329,1000.);
#1668=VECTOR('',#11330,1000.);
#1669=VECTOR('',#11331,1000.);
#1670=VECTOR('',#11332,1000.);
#1671=VECTOR('',#11333,1000.);
#1672=VECTOR('',#11334,1000.);
#1673=VECTOR('',#11335,1000.);
#1674=VECTOR('',#11336,1000.);
#1675=VECTOR('',#11337,1000.);
#1676=VECTOR('',#11338,1000.);
#1677=VECTOR('',#11339,1000.);
#1678=VECTOR('',#11340,1000.);
#1679=VECTOR('',#11341,1000.);
#1680=VECTOR('',#11342,1000.);
#1681=VECTOR('',#11343,1000.);
#1682=VECTOR('',#11344,1000.);
#1683=VECTOR('',#11345,1000.);
#1684=VECTOR('',#11348,1000.);
#1685=VECTOR('',#11351,1000.);
#1686=VECTOR('',#11370,1000.);
#1687=VECTOR('',#11373,1000.);
#1688=VECTOR('',#11378,1000.);
#1689=VECTOR('',#11387,1000.);
#1690=VECTOR('',#11388,1000.);
#1691=VECTOR('',#11389,1000.);
#1692=VECTOR('',#11390,1000.);
#1693=VECTOR('',#11391,1000.);
#1694=VECTOR('',#11392,1000.);
#1695=VECTOR('',#11393,1000.);
#1696=VECTOR('',#11394,1000.);
#1697=VECTOR('',#11395,1000.);
#1698=VECTOR('',#11396,1000.);
#1699=VECTOR('',#11397,1000.);
#1700=VECTOR('',#11398,1000.);
#1701=VECTOR('',#11399,1000.);
#1702=VECTOR('',#11400,1000.);
#1703=VECTOR('',#11401,1000.);
#1704=VECTOR('',#11402,1000.);
#1705=VECTOR('',#11403,1000.);
#1706=VECTOR('',#11404,1000.);
#1707=VECTOR('',#11425,1000.);
#1708=VECTOR('',#11426,1000.);
#1709=VECTOR('',#11427,1000.);
#1710=VECTOR('',#11430,1000.);
#1711=VECTOR('',#11437,1000.);
#1712=VECTOR('',#11440,1000.);
#1713=VECTOR('',#11445,1000.);
#1714=VECTOR('',#11446,1000.);
#1715=VECTOR('',#11451,1000.);
#1716=VECTOR('',#11454,1000.);
#1717=VECTOR('',#11455,1000.);
#1718=VECTOR('',#11458,1000.);
#1719=VECTOR('',#11459,1000.);
#1720=VECTOR('',#11462,1000.);
#1721=VECTOR('',#11463,1000.);
#1722=VECTOR('',#11466,1000.);
#1723=VECTOR('',#11467,1000.);
#1724=VECTOR('',#11470,1000.);
#1725=VECTOR('',#11471,1000.);
#1726=VECTOR('',#11486,1000.);
#1727=VECTOR('',#11491,1000.);
#1728=VECTOR('',#11610,1000.);
#1729=VECTOR('',#11613,1000.);
#1730=VECTOR('',#11618,2.);
#1731=VECTOR('',#11625,2.);
#1732=VECTOR('',#11632,1.00000000000001);
#1733=VECTOR('',#11637,1000.);
#1734=VECTOR('',#11640,1000.);
#1735=VECTOR('',#11645,2.);
#1736=VECTOR('',#11652,2.);
#1737=VECTOR('',#11659,1.00000000000001);
#1738=VECTOR('',#11666,1000.);
#1739=VECTOR('',#11667,1000.);
#1740=VECTOR('',#11670,1000.);
#1741=VECTOR('',#11671,1000.);
#1742=VECTOR('',#11674,1000.);
#1743=VECTOR('',#11675,1000.);
#1744=VECTOR('',#11678,1000.);
#1745=VECTOR('',#11679,1000.);
#1746=VECTOR('',#11682,1000.);
#1747=VECTOR('',#11683,1000.);
#1748=VECTOR('',#11684,1000.);
#1749=VECTOR('',#11687,1000.);
#1750=VECTOR('',#11688,1000.);
#1751=VECTOR('',#11689,1000.);
#1752=VECTOR('',#11690,1000.);
#1753=VECTOR('',#11691,1000.);
#1754=VECTOR('',#11698,1000.);
#1755=VECTOR('',#11699,1000.);
#1756=VECTOR('',#11700,1000.);
#1757=VECTOR('',#11701,1000.);
#1758=VECTOR('',#11702,1000.);
#1759=VECTOR('',#11705,1000.);
#1760=VECTOR('',#11710,1000.);
#1761=VECTOR('',#11713,1000.);
#1762=VECTOR('',#11714,1000.);
#1763=VECTOR('',#11715,1000.);
#1764=VECTOR('',#11716,1000.);
#1765=VECTOR('',#11717,1000.);
#1766=VECTOR('',#11720,1000.);
#1767=VECTOR('',#11721,1000.);
#1768=VECTOR('',#11722,1000.);
#1769=VECTOR('',#11723,1000.);
#1770=VECTOR('',#11728,1000.);
#1771=VECTOR('',#11733,1000.);
#1772=VECTOR('',#11734,1000.);
#1773=VECTOR('',#11737,1000.);
#1774=VECTOR('',#11738,1000.);
#1775=VECTOR('',#11739,1000.);
#1776=VECTOR('',#11742,1000.);
#1777=VECTOR('',#11743,1000.);
#1778=VECTOR('',#11744,1000.);
#1779=VECTOR('',#11747,1000.);
#1780=VECTOR('',#11748,1000.);
#1781=VECTOR('',#11751,1000.);
#1782=VECTOR('',#11758,1000.);
#1783=VECTOR('',#11759,1000.);
#1784=VECTOR('',#11762,1000.);
#1785=VECTOR('',#11767,1000.);
#1786=VECTOR('',#11768,1000.);
#1787=VECTOR('',#11777,1000.);
#1788=VECTOR('',#11778,1000.);
#1789=VECTOR('',#11779,1000.);
#1790=VECTOR('',#11788,1000.);
#1791=VECTOR('',#11791,1000.);
#1792=VECTOR('',#11792,1000.);
#1793=VECTOR('',#11797,1000.);
#1794=VECTOR('',#11798,1000.);
#1795=VECTOR('',#11801,1000.);
#1796=VECTOR('',#11804,1000.);
#1797=VECTOR('',#11805,1000.);
#1798=VECTOR('',#11806,1000.);
#1799=VECTOR('',#11807,1000.);
#1800=VECTOR('',#11808,1000.);
#1801=VECTOR('',#11809,1000.);
#1802=VECTOR('',#11812,1000.);
#1803=VECTOR('',#11817,1000.);
#1804=VECTOR('',#11820,1000.);
#1805=VECTOR('',#11821,1000.);
#1806=VECTOR('',#11822,1000.);
#1807=VECTOR('',#11825,1000.);
#1808=VECTOR('',#11826,1000.);
#1809=VECTOR('',#11831,1000.);
#1810=VECTOR('',#11846,1000.);
#1811=VECTOR('',#11859,1000.);
#1812=VECTOR('',#11864,1000.);
#1813=VECTOR('',#11875,1000.);
#1814=VECTOR('',#11880,1000.);
#1815=VECTOR('',#11881,1000.);
#1816=VECTOR('',#11904,1.);
#1817=VECTOR('',#11921,2.);
#1818=VECTOR('',#11938,0.999999999999998);
#1819=VECTOR('',#11949,1000.);
#1820=VECTOR('',#11950,10.);
#1821=VECTOR('',#11951,1000.);
#1822=VECTOR('',#11954,1000.);
#1823=VECTOR('',#11959,0.999999999999998);
#1824=VECTOR('',#11968,1000.);
#1825=VECTOR('',#11969,1000.);
#1826=VECTOR('',#11970,1000.);
#1827=VECTOR('',#11971,1000.);
#1828=VECTOR('',#11972,1000.);
#1829=VECTOR('',#11973,1000.);
#1830=VECTOR('',#11982,1000.);
#1831=VECTOR('',#11991,1000.);
#1832=VECTOR('',#11992,1000.);
#1833=VECTOR('',#11993,1000.);
#1834=VECTOR('',#12002,1000.);
#1835=VECTOR('',#12079,1.99999999999999);
#1836=VECTOR('',#12082,2.);
#1837=VECTOR('',#12085,1000.);
#1838=VECTOR('',#12086,1000.);
#1839=VECTOR('',#12093,1000.);
#1840=VECTOR('',#12096,1000.);
#1841=VECTOR('',#12099,1000.);
#1842=VECTOR('',#12104,1000.);
#1843=VECTOR('',#12109,1000.);
#1844=VECTOR('',#12112,1000.);
#1845=VECTOR('',#12115,1000.);
#1846=VECTOR('',#12116,1000.);
#1847=VECTOR('',#12117,1000.);
#1848=VECTOR('',#12120,1000.);
#1849=VECTOR('',#12127,1000.);
#1850=VECTOR('',#12128,1000.);
#1851=VECTOR('',#12129,1000.);
#1852=VECTOR('',#12132,1000.);
#1853=VECTOR('',#12139,1000.);
#1854=VECTOR('',#12140,1000.);
#1855=VECTOR('',#12141,1000.);
#1856=VECTOR('',#12144,1000.);
#1857=CYLINDRICAL_SURFACE('',#9074,2.);
#1858=CYLINDRICAL_SURFACE('',#9099,0.400000000000003);
#1859=CYLINDRICAL_SURFACE('',#9106,0.400000000000011);
#1860=CYLINDRICAL_SURFACE('',#9115,2.);
#1861=CYLINDRICAL_SURFACE('',#9123,5.);
#1862=CYLINDRICAL_SURFACE('',#9148,2.);
#1863=CYLINDRICAL_SURFACE('',#9151,2.);
#1864=CYLINDRICAL_SURFACE('',#9154,15.);
#1865=CYLINDRICAL_SURFACE('',#9157,15.);
#1866=CYLINDRICAL_SURFACE('',#9160,4.);
#1867=CYLINDRICAL_SURFACE('',#9163,4.);
#1868=CYLINDRICAL_SURFACE('',#9164,4.);
#1869=CYLINDRICAL_SURFACE('',#9166,3.);
#1870=CYLINDRICAL_SURFACE('',#9167,3.);
#1871=CYLINDRICAL_SURFACE('',#9168,3.);
#1872=CYLINDRICAL_SURFACE('',#9169,3.);
#1873=CYLINDRICAL_SURFACE('',#9170,3.);
#1874=CYLINDRICAL_SURFACE('',#9171,3.);
#1875=CYLINDRICAL_SURFACE('',#9172,3.);
#1876=CYLINDRICAL_SURFACE('',#9185,3.);
#1877=CYLINDRICAL_SURFACE('',#9186,3.);
#1878=CYLINDRICAL_SURFACE('',#9187,3.);
#1879=CYLINDRICAL_SURFACE('',#9188,3.);
#1880=CYLINDRICAL_SURFACE('',#9189,3.);
#1881=CYLINDRICAL_SURFACE('',#9190,3.);
#1882=CYLINDRICAL_SURFACE('',#9191,3.);
#1883=CYLINDRICAL_SURFACE('',#9211,15.);
#1884=CYLINDRICAL_SURFACE('',#9222,15.);
#1885=CYLINDRICAL_SURFACE('',#9236,1.49999773384112);
#1886=CYLINDRICAL_SURFACE('',#9242,39.5);
#1887=CYLINDRICAL_SURFACE('',#9245,11.7);
#1888=CYLINDRICAL_SURFACE('',#9279,0.5);
#1889=CYLINDRICAL_SURFACE('',#9283,0.5);
#1890=CYLINDRICAL_SURFACE('',#9292,4.);
#1891=CYLINDRICAL_SURFACE('',#9296,0.5);
#1892=CYLINDRICAL_SURFACE('',#9300,0.500000000000003);
#1893=CYLINDRICAL_SURFACE('',#9303,0.5);
#1894=CYLINDRICAL_SURFACE('',#9307,0.500000000000003);
#1895=CYLINDRICAL_SURFACE('',#9311,0.5);
#1896=CYLINDRICAL_SURFACE('',#9314,0.500000000000001);
#1897=CYLINDRICAL_SURFACE('',#9317,0.5);
#1898=CYLINDRICAL_SURFACE('',#9321,0.500000000000003);
#1899=CYLINDRICAL_SURFACE('',#9325,0.5);
#1900=CYLINDRICAL_SURFACE('',#9328,10.);
#1901=CYLINDRICAL_SURFACE('',#9346,2.99999999999999);
#1902=CYLINDRICAL_SURFACE('',#9348,2.99999999999999);
#1903=CYLINDRICAL_SURFACE('',#9350,2.99999999999999);
#1904=CYLINDRICAL_SURFACE('',#9351,2.99999999999999);
#1905=CYLINDRICAL_SURFACE('',#9352,2.99999999999999);
#1906=CYLINDRICAL_SURFACE('',#9353,2.99999999999999);
#1907=CYLINDRICAL_SURFACE('',#9354,2.99999999999999);
#1908=CYLINDRICAL_SURFACE('',#9355,2.99999999999999);
#1909=CYLINDRICAL_SURFACE('',#9356,2.99999999999999);
#1910=CYLINDRICAL_SURFACE('',#9357,2.99999999999999);
#1911=CYLINDRICAL_SURFACE('',#9358,2.99999999999999);
#1912=CYLINDRICAL_SURFACE('',#9359,2.99999999999999);
#1913=CYLINDRICAL_SURFACE('',#9360,2.99999999999999);
#1914=CYLINDRICAL_SURFACE('',#9361,2.99999999999999);
#1915=CYLINDRICAL_SURFACE('',#9362,2.99999999999999);
#1916=CYLINDRICAL_SURFACE('',#9363,2.99999999999999);
#1917=CYLINDRICAL_SURFACE('',#9364,2.99999999999999);
#1918=CYLINDRICAL_SURFACE('',#9365,2.99999999999999);
#1919=CYLINDRICAL_SURFACE('',#9366,2.99999999999999);
#1920=CYLINDRICAL_SURFACE('',#9367,2.99999999999999);
#1921=CYLINDRICAL_SURFACE('',#9368,2.99999999999999);
#1922=CYLINDRICAL_SURFACE('',#9369,2.99999999999999);
#1923=CYLINDRICAL_SURFACE('',#9370,2.99999999999999);
#1924=CYLINDRICAL_SURFACE('',#9371,2.99999999999999);
#1925=CYLINDRICAL_SURFACE('',#9372,2.99999999999999);
#1926=CYLINDRICAL_SURFACE('',#9373,2.99999999999999);
#1927=CYLINDRICAL_SURFACE('',#9374,2.99999999999999);
#1928=CYLINDRICAL_SURFACE('',#9375,2.99999999999999);
#1929=CYLINDRICAL_SURFACE('',#9376,2.99999999999999);
#1930=CYLINDRICAL_SURFACE('',#9377,2.99999999999999);
#1931=CYLINDRICAL_SURFACE('',#9378,2.99999999999999);
#1932=CYLINDRICAL_SURFACE('',#9379,2.99999999999999);
#1933=CYLINDRICAL_SURFACE('',#9380,2.99999999999999);
#1934=CYLINDRICAL_SURFACE('',#9381,2.99999999999999);
#1935=CYLINDRICAL_SURFACE('',#9382,2.99999999999999);
#1936=CYLINDRICAL_SURFACE('',#9383,2.99999999999999);
#1937=CYLINDRICAL_SURFACE('',#9384,2.99999999999999);
#1938=CYLINDRICAL_SURFACE('',#9385,2.99999999999999);
#1939=CYLINDRICAL_SURFACE('',#9386,2.99999999999999);
#1940=CYLINDRICAL_SURFACE('',#9387,2.99999999999999);
#1941=CYLINDRICAL_SURFACE('',#9388,2.99999999999999);
#1942=CYLINDRICAL_SURFACE('',#9394,0.500000000000008);
#1943=CYLINDRICAL_SURFACE('',#9395,0.500000000000008);
#1944=CYLINDRICAL_SURFACE('',#9396,0.500000000000008);
#1945=CYLINDRICAL_SURFACE('',#9397,0.500000000000008);
#1946=CYLINDRICAL_SURFACE('',#9398,0.500000000000008);
#1947=CYLINDRICAL_SURFACE('',#9399,0.500000000000008);
#1948=CYLINDRICAL_SURFACE('',#9400,0.500000000000008);
#1949=CYLINDRICAL_SURFACE('',#9401,0.500000000000008);
#1950=CYLINDRICAL_SURFACE('',#9402,0.500000000000008);
#1951=CYLINDRICAL_SURFACE('',#9403,0.500000000000008);
#1952=CYLINDRICAL_SURFACE('',#9464,2.99999999999999);
#1953=CYLINDRICAL_SURFACE('',#9465,6.99999999999999);
#1954=CYLINDRICAL_SURFACE('',#9466,6.99999999999999);
#1955=CYLINDRICAL_SURFACE('',#9467,6.99999999999999);
#1956=CYLINDRICAL_SURFACE('',#9468,6.99999999999999);
#1957=CYLINDRICAL_SURFACE('',#9469,6.99999999999999);
#1958=CYLINDRICAL_SURFACE('',#9470,6.99999999999999);
#1959=CYLINDRICAL_SURFACE('',#9471,6.99999999999999);
#1960=CYLINDRICAL_SURFACE('',#9472,6.99999999999999);
#1961=CYLINDRICAL_SURFACE('',#9473,6.99999999999999);
#1962=CYLINDRICAL_SURFACE('',#9474,6.99999999999999);
#1963=CYLINDRICAL_SURFACE('',#9475,6.99999999999999);
#1964=CYLINDRICAL_SURFACE('',#9476,6.99999999999999);
#1965=CYLINDRICAL_SURFACE('',#9477,6.99999999999999);
#1966=CYLINDRICAL_SURFACE('',#9478,6.99999999999999);
#1967=CYLINDRICAL_SURFACE('',#9479,6.99999999999999);
#1968=CYLINDRICAL_SURFACE('',#9480,6.99999999999999);
#1969=CYLINDRICAL_SURFACE('',#9481,6.99999999999999);
#1970=CYLINDRICAL_SURFACE('',#9482,6.99999999999999);
#1971=CYLINDRICAL_SURFACE('',#9483,6.99999999999999);
#1972=CYLINDRICAL_SURFACE('',#9484,6.99999999999999);
#1973=CYLINDRICAL_SURFACE('',#9485,6.99999999999999);
#1974=CYLINDRICAL_SURFACE('',#9486,6.99999999999999);
#1975=CYLINDRICAL_SURFACE('',#9487,6.99999999999999);
#1976=CYLINDRICAL_SURFACE('',#9488,6.99999999999999);
#1977=CYLINDRICAL_SURFACE('',#9489,6.99999999999999);
#1978=CYLINDRICAL_SURFACE('',#9492,6.99999999999999);
#1979=CYLINDRICAL_SURFACE('',#9494,0.500000000000008);
#1980=CYLINDRICAL_SURFACE('',#9495,0.500000000000008);
#1981=CYLINDRICAL_SURFACE('',#9496,0.500000000000008);
#1982=CYLINDRICAL_SURFACE('',#9497,0.500000000000008);
#1983=CYLINDRICAL_SURFACE('',#9498,0.500000000000008);
#1984=CYLINDRICAL_SURFACE('',#9499,0.500000000000009);
#1985=CYLINDRICAL_SURFACE('',#9500,0.500000000000008);
#1986=CYLINDRICAL_SURFACE('',#9501,0.500000000000008);
#1987=CYLINDRICAL_SURFACE('',#9502,0.500000000000008);
#1988=CYLINDRICAL_SURFACE('',#9503,0.500000000000009);
#1989=CYLINDRICAL_SURFACE('',#9504,0.500000000000007);
#1990=CYLINDRICAL_SURFACE('',#9505,0.500000000000007);
#1991=CYLINDRICAL_SURFACE('',#9506,0.500000000000008);
#1992=CYLINDRICAL_SURFACE('',#9507,0.500000000000008);
#1993=CYLINDRICAL_SURFACE('',#9508,0.500000000000008);
#1994=CYLINDRICAL_SURFACE('',#9509,0.500000000000008);
#1995=CYLINDRICAL_SURFACE('',#9512,4.);
#1996=CYLINDRICAL_SURFACE('',#9513,2.);
#1997=CYLINDRICAL_SURFACE('',#9514,4.);
#1998=CYLINDRICAL_SURFACE('',#9526,1.5);
#1999=CYLINDRICAL_SURFACE('',#9529,2.00000000000001);
#2000=CYLINDRICAL_SURFACE('',#9532,2.);
#2001=CYLINDRICAL_SURFACE('',#9543,100.);
#2002=CYLINDRICAL_SURFACE('',#9546,6.4);
#2003=CYLINDRICAL_SURFACE('',#9547,100.);
#2004=CYLINDRICAL_SURFACE('',#9550,100.);
#2005=CYLINDRICAL_SURFACE('',#9557,100.);
#2006=CYLINDRICAL_SURFACE('',#9560,3.);
#2007=CYLINDRICAL_SURFACE('',#9584,16.);
#2008=CYLINDRICAL_SURFACE('',#9589,7.);
#2009=CYLINDRICAL_SURFACE('',#9592,12.);
#2010=CYLINDRICAL_SURFACE('',#9596,28.);
#2011=CYLINDRICAL_SURFACE('',#9601,35.);
#2012=CYLINDRICAL_SURFACE('',#9632,3.);
#2013=CYLINDRICAL_SURFACE('',#9640,3.7);
#2014=CYLINDRICAL_SURFACE('',#9665,0.500000000000001);
#2015=CYLINDRICAL_SURFACE('',#9676,0.500000000000001);
#2016=CYLINDRICAL_SURFACE('',#9692,0.499999999999999);
#2017=CYLINDRICAL_SURFACE('',#9716,220.3);
#2018=CYLINDRICAL_SURFACE('',#9719,2.);
#2019=CYLINDRICAL_SURFACE('',#9722,2.);
#2020=CYLINDRICAL_SURFACE('',#9725,1.00000000000001);
#2021=CYLINDRICAL_SURFACE('',#9728,75.);
#2022=CYLINDRICAL_SURFACE('',#9730,2.);
#2023=CYLINDRICAL_SURFACE('',#9733,2.);
#2024=CYLINDRICAL_SURFACE('',#9736,1.00000000000001);
#2025=CYLINDRICAL_SURFACE('',#9739,75.);
#2026=CYLINDRICAL_SURFACE('',#9741,222.);
#2027=CYLINDRICAL_SURFACE('',#9754,100.);
#2028=CYLINDRICAL_SURFACE('',#9781,101.7);
#2029=CYLINDRICAL_SURFACE('',#9789,3.);
#2030=CYLINDRICAL_SURFACE('',#9791,3.00000000000001);
#2031=CYLINDRICAL_SURFACE('',#9792,3.00000000000001);
#2032=CYLINDRICAL_SURFACE('',#9793,3.00000000000001);
#2033=CYLINDRICAL_SURFACE('',#9794,1.5);
#2034=CYLINDRICAL_SURFACE('',#9796,1.5);
#2035=CYLINDRICAL_SURFACE('',#9800,1.5);
#2036=CYLINDRICAL_SURFACE('',#9801,1.5);
#2037=CYLINDRICAL_SURFACE('',#9803,1.5);
#2038=CYLINDRICAL_SURFACE('',#9807,1.5);
#2039=CYLINDRICAL_SURFACE('',#9808,2.06253449527014);
#2040=CYLINDRICAL_SURFACE('',#9819,1.);
#2041=CYLINDRICAL_SURFACE('',#9827,2.);
#2042=CYLINDRICAL_SURFACE('',#9835,0.999999999999998);
#2043=CYLINDRICAL_SURFACE('',#9840,0.6);
#2044=CYLINDRICAL_SURFACE('',#9843,0.999999999999998);
#2045=CYLINDRICAL_SURFACE('',#9849,33.6360679582853);
#2046=CYLINDRICAL_SURFACE('',#9857,33.6360679582853);
#2047=CYLINDRICAL_SURFACE('',#9862,1.);
#2048=CYLINDRICAL_SURFACE('',#9864,1.);
#2049=CYLINDRICAL_SURFACE('',#9866,0.999999999999998);
#2050=CYLINDRICAL_SURFACE('',#9898,1.99999999999999);
#2051=CYLINDRICAL_SURFACE('',#9899,2.);
#2052=CYLINDRICAL_SURFACE('',#9900,4.4);
#2053=CYLINDRICAL_SURFACE('',#9912,20.);
#2054=CYLINDRICAL_SURFACE('',#9916,4.4);
#2055=CYLINDRICAL_SURFACE('',#9920,9.99999999999999);
#2056=CYLINDRICAL_SURFACE('',#9923,24.);
#2057=CYLINDRICAL_SURFACE('',#9926,0.25);
#2058=CYLINDRICAL_SURFACE('',#9930,0.250000000000004);
#2059=CYLINDRICAL_SURFACE('',#9931,0.25);
#2060=CYLINDRICAL_SURFACE('',#9935,0.250000000000004);
#2061=CYLINDRICAL_SURFACE('',#9941,0.25);
#2062=CYLINDRICAL_SURFACE('',#9943,0.25);
#2063=FACE_OUTER_BOUND('',#2575,.T.);
#2064=FACE_OUTER_BOUND('',#2576,.T.);
#2065=FACE_OUTER_BOUND('',#2577,.T.);
#2066=FACE_OUTER_BOUND('',#2578,.T.);
#2067=FACE_OUTER_BOUND('',#2580,.T.);
#2068=FACE_OUTER_BOUND('',#2582,.T.);
#2069=FACE_OUTER_BOUND('',#2583,.T.);
#2070=FACE_OUTER_BOUND('',#2584,.T.);
#2071=FACE_OUTER_BOUND('',#2585,.T.);
#2072=FACE_OUTER_BOUND('',#2586,.T.);
#2073=FACE_OUTER_BOUND('',#2587,.T.);
#2074=FACE_OUTER_BOUND('',#2588,.T.);
#2075=FACE_OUTER_BOUND('',#2589,.T.);
#2076=FACE_OUTER_BOUND('',#2590,.T.);
#2077=FACE_OUTER_BOUND('',#2591,.T.);
#2078=FACE_OUTER_BOUND('',#2592,.T.);
#2079=FACE_OUTER_BOUND('',#2593,.T.);
#2080=FACE_OUTER_BOUND('',#2594,.T.);
#2081=FACE_OUTER_BOUND('',#2595,.T.);
#2082=FACE_OUTER_BOUND('',#2596,.T.);
#2083=FACE_OUTER_BOUND('',#2597,.T.);
#2084=FACE_OUTER_BOUND('',#2598,.T.);
#2085=FACE_OUTER_BOUND('',#2599,.T.);
#2086=FACE_OUTER_BOUND('',#2601,.T.);
#2087=FACE_OUTER_BOUND('',#2603,.T.);
#2088=FACE_OUTER_BOUND('',#2604,.T.);
#2089=FACE_OUTER_BOUND('',#2605,.T.);
#2090=FACE_OUTER_BOUND('',#2606,.T.);
#2091=FACE_OUTER_BOUND('',#2607,.T.);
#2092=FACE_OUTER_BOUND('',#2608,.T.);
#2093=FACE_OUTER_BOUND('',#2609,.T.);
#2094=FACE_OUTER_BOUND('',#2610,.T.);
#2095=FACE_OUTER_BOUND('',#2611,.T.);
#2096=FACE_OUTER_BOUND('',#2612,.T.);
#2097=FACE_OUTER_BOUND('',#2613,.T.);
#2098=FACE_OUTER_BOUND('',#2614,.T.);
#2099=FACE_OUTER_BOUND('',#2615,.T.);
#2100=FACE_OUTER_BOUND('',#2616,.T.);
#2101=FACE_OUTER_BOUND('',#2617,.T.);
#2102=FACE_OUTER_BOUND('',#2618,.T.);
#2103=FACE_OUTER_BOUND('',#2619,.T.);
#2104=FACE_OUTER_BOUND('',#2620,.T.);
#2105=FACE_OUTER_BOUND('',#2621,.T.);
#2106=FACE_OUTER_BOUND('',#2622,.T.);
#2107=FACE_OUTER_BOUND('',#2623,.T.);
#2108=FACE_OUTER_BOUND('',#2624,.T.);
#2109=FACE_OUTER_BOUND('',#2625,.T.);
#2110=FACE_OUTER_BOUND('',#2626,.T.);
#2111=FACE_OUTER_BOUND('',#2627,.T.);
#2112=FACE_OUTER_BOUND('',#2628,.T.);
#2113=FACE_OUTER_BOUND('',#2629,.T.);
#2114=FACE_OUTER_BOUND('',#2630,.T.);
#2115=FACE_OUTER_BOUND('',#2632,.T.);
#2116=FACE_OUTER_BOUND('',#2633,.T.);
#2117=FACE_OUTER_BOUND('',#2634,.T.);
#2118=FACE_OUTER_BOUND('',#2635,.T.);
#2119=FACE_OUTER_BOUND('',#2636,.T.);
#2120=FACE_OUTER_BOUND('',#2637,.T.);
#2121=FACE_OUTER_BOUND('',#2638,.T.);
#2122=FACE_OUTER_BOUND('',#2639,.T.);
#2123=FACE_OUTER_BOUND('',#2640,.T.);
#2124=FACE_OUTER_BOUND('',#2641,.T.);
#2125=FACE_OUTER_BOUND('',#2642,.T.);
#2126=FACE_OUTER_BOUND('',#2643,.T.);
#2127=FACE_OUTER_BOUND('',#2644,.T.);
#2128=FACE_OUTER_BOUND('',#2645,.T.);
#2129=FACE_OUTER_BOUND('',#2646,.T.);
#2130=FACE_OUTER_BOUND('',#2647,.T.);
#2131=FACE_OUTER_BOUND('',#2648,.T.);
#2132=FACE_OUTER_BOUND('',#2649,.T.);
#2133=FACE_OUTER_BOUND('',#2650,.T.);
#2134=FACE_OUTER_BOUND('',#2651,.T.);
#2135=FACE_OUTER_BOUND('',#2652,.T.);
#2136=FACE_OUTER_BOUND('',#2653,.T.);
#2137=FACE_OUTER_BOUND('',#2654,.T.);
#2138=FACE_OUTER_BOUND('',#2655,.T.);
#2139=FACE_OUTER_BOUND('',#2656,.T.);
#2140=FACE_OUTER_BOUND('',#2657,.T.);
#2141=FACE_OUTER_BOUND('',#2658,.T.);
#2142=FACE_OUTER_BOUND('',#2659,.T.);
#2143=FACE_OUTER_BOUND('',#2660,.T.);
#2144=FACE_OUTER_BOUND('',#2661,.T.);
#2145=FACE_OUTER_BOUND('',#2662,.T.);
#2146=FACE_OUTER_BOUND('',#2663,.T.);
#2147=FACE_OUTER_BOUND('',#2664,.T.);
#2148=FACE_OUTER_BOUND('',#2666,.T.);
#2149=FACE_OUTER_BOUND('',#2668,.T.);
#2150=FACE_OUTER_BOUND('',#2669,.T.);
#2151=FACE_OUTER_BOUND('',#2670,.T.);
#2152=FACE_OUTER_BOUND('',#2671,.T.);
#2153=FACE_OUTER_BOUND('',#2672,.T.);
#2154=FACE_OUTER_BOUND('',#2674,.T.);
#2155=FACE_OUTER_BOUND('',#2675,.T.);
#2156=FACE_OUTER_BOUND('',#2676,.T.);
#2157=FACE_OUTER_BOUND('',#2677,.T.);
#2158=FACE_OUTER_BOUND('',#2678,.T.);
#2159=FACE_OUTER_BOUND('',#2679,.T.);
#2160=FACE_OUTER_BOUND('',#2680,.T.);
#2161=FACE_OUTER_BOUND('',#2681,.T.);
#2162=FACE_OUTER_BOUND('',#2682,.T.);
#2163=FACE_OUTER_BOUND('',#2683,.T.);
#2164=FACE_OUTER_BOUND('',#2684,.T.);
#2165=FACE_OUTER_BOUND('',#2685,.T.);
#2166=FACE_OUTER_BOUND('',#2686,.T.);
#2167=FACE_OUTER_BOUND('',#2687,.T.);
#2168=FACE_OUTER_BOUND('',#2688,.T.);
#2169=FACE_OUTER_BOUND('',#2689,.T.);
#2170=FACE_OUTER_BOUND('',#2690,.T.);
#2171=FACE_OUTER_BOUND('',#2691,.T.);
#2172=FACE_OUTER_BOUND('',#2692,.T.);
#2173=FACE_OUTER_BOUND('',#2693,.T.);
#2174=FACE_OUTER_BOUND('',#2694,.T.);
#2175=FACE_OUTER_BOUND('',#2695,.T.);
#2176=FACE_OUTER_BOUND('',#2696,.T.);
#2177=FACE_OUTER_BOUND('',#2697,.T.);
#2178=FACE_OUTER_BOUND('',#2698,.T.);
#2179=FACE_OUTER_BOUND('',#2699,.T.);
#2180=FACE_OUTER_BOUND('',#2700,.T.);
#2181=FACE_OUTER_BOUND('',#2701,.T.);
#2182=FACE_OUTER_BOUND('',#2702,.T.);
#2183=FACE_OUTER_BOUND('',#2703,.T.);
#2184=FACE_OUTER_BOUND('',#2704,.T.);
#2185=FACE_OUTER_BOUND('',#2705,.T.);
#2186=FACE_OUTER_BOUND('',#2706,.T.);
#2187=FACE_OUTER_BOUND('',#2707,.T.);
#2188=FACE_OUTER_BOUND('',#2708,.T.);
#2189=FACE_OUTER_BOUND('',#2709,.T.);
#2190=FACE_OUTER_BOUND('',#2710,.T.);
#2191=FACE_OUTER_BOUND('',#2711,.T.);
#2192=FACE_OUTER_BOUND('',#2712,.T.);
#2193=FACE_OUTER_BOUND('',#2713,.T.);
#2194=FACE_OUTER_BOUND('',#2714,.T.);
#2195=FACE_OUTER_BOUND('',#2715,.T.);
#2196=FACE_OUTER_BOUND('',#2716,.T.);
#2197=FACE_OUTER_BOUND('',#2717,.T.);
#2198=FACE_OUTER_BOUND('',#2718,.T.);
#2199=FACE_OUTER_BOUND('',#2719,.T.);
#2200=FACE_OUTER_BOUND('',#2720,.T.);
#2201=FACE_OUTER_BOUND('',#2721,.T.);
#2202=FACE_OUTER_BOUND('',#2722,.T.);
#2203=FACE_OUTER_BOUND('',#2723,.T.);
#2204=FACE_OUTER_BOUND('',#2724,.T.);
#2205=FACE_OUTER_BOUND('',#2725,.T.);
#2206=FACE_OUTER_BOUND('',#2726,.T.);
#2207=FACE_OUTER_BOUND('',#2727,.T.);
#2208=FACE_OUTER_BOUND('',#2728,.T.);
#2209=FACE_OUTER_BOUND('',#2729,.T.);
#2210=FACE_OUTER_BOUND('',#2730,.T.);
#2211=FACE_OUTER_BOUND('',#2731,.T.);
#2212=FACE_OUTER_BOUND('',#2732,.T.);
#2213=FACE_OUTER_BOUND('',#2733,.T.);
#2214=FACE_OUTER_BOUND('',#2734,.T.);
#2215=FACE_OUTER_BOUND('',#2735,.T.);
#2216=FACE_OUTER_BOUND('',#2736,.T.);
#2217=FACE_OUTER_BOUND('',#2737,.T.);
#2218=FACE_OUTER_BOUND('',#2738,.T.);
#2219=FACE_OUTER_BOUND('',#2739,.T.);
#2220=FACE_OUTER_BOUND('',#2740,.T.);
#2221=FACE_OUTER_BOUND('',#2741,.T.);
#2222=FACE_OUTER_BOUND('',#2742,.T.);
#2223=FACE_OUTER_BOUND('',#2743,.T.);
#2224=FACE_OUTER_BOUND('',#2744,.T.);
#2225=FACE_OUTER_BOUND('',#2745,.T.);
#2226=FACE_OUTER_BOUND('',#2746,.T.);
#2227=FACE_OUTER_BOUND('',#2747,.T.);
#2228=FACE_OUTER_BOUND('',#2748,.T.);
#2229=FACE_OUTER_BOUND('',#2749,.T.);
#2230=FACE_OUTER_BOUND('',#2750,.T.);
#2231=FACE_OUTER_BOUND('',#2751,.T.);
#2232=FACE_OUTER_BOUND('',#2752,.T.);
#2233=FACE_OUTER_BOUND('',#2753,.T.);
#2234=FACE_OUTER_BOUND('',#2754,.T.);
#2235=FACE_OUTER_BOUND('',#2755,.T.);
#2236=FACE_OUTER_BOUND('',#2756,.T.);
#2237=FACE_OUTER_BOUND('',#2757,.T.);
#2238=FACE_OUTER_BOUND('',#2758,.T.);
#2239=FACE_OUTER_BOUND('',#2759,.T.);
#2240=FACE_OUTER_BOUND('',#2760,.T.);
#2241=FACE_OUTER_BOUND('',#2761,.T.);
#2242=FACE_OUTER_BOUND('',#2762,.T.);
#2243=FACE_OUTER_BOUND('',#2763,.T.);
#2244=FACE_OUTER_BOUND('',#2764,.T.);
#2245=FACE_OUTER_BOUND('',#2765,.T.);
#2246=FACE_OUTER_BOUND('',#2766,.T.);
#2247=FACE_OUTER_BOUND('',#2767,.T.);
#2248=FACE_OUTER_BOUND('',#2768,.T.);
#2249=FACE_OUTER_BOUND('',#2769,.T.);
#2250=FACE_OUTER_BOUND('',#2770,.T.);
#2251=FACE_OUTER_BOUND('',#2771,.T.);
#2252=FACE_OUTER_BOUND('',#2772,.T.);
#2253=FACE_OUTER_BOUND('',#2773,.T.);
#2254=FACE_OUTER_BOUND('',#2774,.T.);
#2255=FACE_OUTER_BOUND('',#2775,.T.);
#2256=FACE_OUTER_BOUND('',#2776,.T.);
#2257=FACE_OUTER_BOUND('',#2777,.T.);
#2258=FACE_OUTER_BOUND('',#2778,.T.);
#2259=FACE_OUTER_BOUND('',#2779,.T.);
#2260=FACE_OUTER_BOUND('',#2780,.T.);
#2261=FACE_OUTER_BOUND('',#2781,.T.);
#2262=FACE_OUTER_BOUND('',#2782,.T.);
#2263=FACE_OUTER_BOUND('',#2783,.T.);
#2264=FACE_OUTER_BOUND('',#2784,.T.);
#2265=FACE_OUTER_BOUND('',#2785,.T.);
#2266=FACE_OUTER_BOUND('',#2786,.T.);
#2267=FACE_OUTER_BOUND('',#2787,.T.);
#2268=FACE_OUTER_BOUND('',#2788,.T.);
#2269=FACE_OUTER_BOUND('',#2789,.T.);
#2270=FACE_OUTER_BOUND('',#2790,.T.);
#2271=FACE_OUTER_BOUND('',#2791,.T.);
#2272=FACE_OUTER_BOUND('',#2792,.T.);
#2273=FACE_OUTER_BOUND('',#2793,.T.);
#2274=FACE_OUTER_BOUND('',#2794,.T.);
#2275=FACE_OUTER_BOUND('',#2795,.T.);
#2276=FACE_OUTER_BOUND('',#2796,.T.);
#2277=FACE_OUTER_BOUND('',#2797,.T.);
#2278=FACE_OUTER_BOUND('',#2798,.T.);
#2279=FACE_OUTER_BOUND('',#2799,.T.);
#2280=FACE_OUTER_BOUND('',#2800,.T.);
#2281=FACE_OUTER_BOUND('',#2801,.T.);
#2282=FACE_OUTER_BOUND('',#2802,.T.);
#2283=FACE_OUTER_BOUND('',#2803,.T.);
#2284=FACE_OUTER_BOUND('',#2804,.T.);
#2285=FACE_OUTER_BOUND('',#2805,.T.);
#2286=FACE_OUTER_BOUND('',#2806,.T.);
#2287=FACE_OUTER_BOUND('',#2807,.T.);
#2288=FACE_OUTER_BOUND('',#2808,.T.);
#2289=FACE_OUTER_BOUND('',#2809,.T.);
#2290=FACE_OUTER_BOUND('',#2810,.T.);
#2291=FACE_OUTER_BOUND('',#2811,.T.);
#2292=FACE_OUTER_BOUND('',#2812,.T.);
#2293=FACE_OUTER_BOUND('',#2813,.T.);
#2294=FACE_OUTER_BOUND('',#2814,.T.);
#2295=FACE_OUTER_BOUND('',#2815,.T.);
#2296=FACE_OUTER_BOUND('',#2816,.T.);
#2297=FACE_OUTER_BOUND('',#2817,.T.);
#2298=FACE_OUTER_BOUND('',#2818,.T.);
#2299=FACE_OUTER_BOUND('',#2819,.T.);
#2300=FACE_OUTER_BOUND('',#2820,.T.);
#2301=FACE_OUTER_BOUND('',#2821,.T.);
#2302=FACE_OUTER_BOUND('',#2822,.T.);
#2303=FACE_OUTER_BOUND('',#2823,.T.);
#2304=FACE_OUTER_BOUND('',#2824,.T.);
#2305=FACE_OUTER_BOUND('',#2825,.T.);
#2306=FACE_OUTER_BOUND('',#2826,.T.);
#2307=FACE_OUTER_BOUND('',#2827,.T.);
#2308=FACE_OUTER_BOUND('',#2828,.T.);
#2309=FACE_OUTER_BOUND('',#2829,.T.);
#2310=FACE_OUTER_BOUND('',#2830,.T.);
#2311=FACE_OUTER_BOUND('',#2831,.T.);
#2312=FACE_OUTER_BOUND('',#2832,.T.);
#2313=FACE_OUTER_BOUND('',#2833,.T.);
#2314=FACE_OUTER_BOUND('',#2834,.T.);
#2315=FACE_OUTER_BOUND('',#2835,.T.);
#2316=FACE_OUTER_BOUND('',#2836,.T.);
#2317=FACE_OUTER_BOUND('',#2837,.T.);
#2318=FACE_OUTER_BOUND('',#2838,.T.);
#2319=FACE_OUTER_BOUND('',#2839,.T.);
#2320=FACE_OUTER_BOUND('',#2840,.T.);
#2321=FACE_OUTER_BOUND('',#2841,.T.);
#2322=FACE_OUTER_BOUND('',#2842,.T.);
#2323=FACE_OUTER_BOUND('',#2843,.T.);
#2324=FACE_OUTER_BOUND('',#2844,.T.);
#2325=FACE_OUTER_BOUND('',#2845,.T.);
#2326=FACE_OUTER_BOUND('',#2846,.T.);
#2327=FACE_OUTER_BOUND('',#2847,.T.);
#2328=FACE_OUTER_BOUND('',#2848,.T.);
#2329=FACE_OUTER_BOUND('',#2849,.T.);
#2330=FACE_OUTER_BOUND('',#2850,.T.);
#2331=FACE_OUTER_BOUND('',#2851,.T.);
#2332=FACE_OUTER_BOUND('',#2852,.T.);
#2333=FACE_OUTER_BOUND('',#2853,.T.);
#2334=FACE_OUTER_BOUND('',#2854,.T.);
#2335=FACE_OUTER_BOUND('',#2855,.T.);
#2336=FACE_OUTER_BOUND('',#2856,.T.);
#2337=FACE_OUTER_BOUND('',#2858,.T.);
#2338=FACE_OUTER_BOUND('',#2859,.T.);
#2339=FACE_OUTER_BOUND('',#2860,.T.);
#2340=FACE_OUTER_BOUND('',#2861,.T.);
#2341=FACE_OUTER_BOUND('',#2862,.T.);
#2342=FACE_OUTER_BOUND('',#2863,.T.);
#2343=FACE_OUTER_BOUND('',#2864,.T.);
#2344=FACE_OUTER_BOUND('',#2865,.T.);
#2345=FACE_OUTER_BOUND('',#2866,.T.);
#2346=FACE_OUTER_BOUND('',#2867,.T.);
#2347=FACE_OUTER_BOUND('',#2868,.T.);
#2348=FACE_OUTER_BOUND('',#2869,.T.);
#2349=FACE_OUTER_BOUND('',#2870,.T.);
#2350=FACE_OUTER_BOUND('',#2871,.T.);
#2351=FACE_OUTER_BOUND('',#2872,.T.);
#2352=FACE_OUTER_BOUND('',#2873,.T.);
#2353=FACE_OUTER_BOUND('',#2874,.T.);
#2354=FACE_OUTER_BOUND('',#2875,.T.);
#2355=FACE_OUTER_BOUND('',#2876,.T.);
#2356=FACE_OUTER_BOUND('',#2877,.T.);
#2357=FACE_OUTER_BOUND('',#2878,.T.);
#2358=FACE_OUTER_BOUND('',#2879,.T.);
#2359=FACE_OUTER_BOUND('',#2880,.T.);
#2360=FACE_OUTER_BOUND('',#2881,.T.);
#2361=FACE_OUTER_BOUND('',#2882,.T.);
#2362=FACE_OUTER_BOUND('',#2883,.T.);
#2363=FACE_OUTER_BOUND('',#2884,.T.);
#2364=FACE_OUTER_BOUND('',#2885,.T.);
#2365=FACE_OUTER_BOUND('',#2886,.T.);
#2366=FACE_OUTER_BOUND('',#2887,.T.);
#2367=FACE_OUTER_BOUND('',#2888,.T.);
#2368=FACE_OUTER_BOUND('',#2889,.T.);
#2369=FACE_OUTER_BOUND('',#2890,.T.);
#2370=FACE_OUTER_BOUND('',#2891,.T.);
#2371=FACE_OUTER_BOUND('',#2892,.T.);
#2372=FACE_OUTER_BOUND('',#2893,.T.);
#2373=FACE_OUTER_BOUND('',#2894,.T.);
#2374=FACE_OUTER_BOUND('',#2895,.T.);
#2375=FACE_OUTER_BOUND('',#2896,.T.);
#2376=FACE_OUTER_BOUND('',#2897,.T.);
#2377=FACE_OUTER_BOUND('',#2900,.T.);
#2378=FACE_OUTER_BOUND('',#2903,.T.);
#2379=FACE_OUTER_BOUND('',#2904,.T.);
#2380=FACE_OUTER_BOUND('',#2905,.T.);
#2381=FACE_OUTER_BOUND('',#2906,.T.);
#2382=FACE_OUTER_BOUND('',#2907,.T.);
#2383=FACE_OUTER_BOUND('',#2908,.T.);
#2384=FACE_OUTER_BOUND('',#2909,.T.);
#2385=FACE_OUTER_BOUND('',#2910,.T.);
#2386=FACE_OUTER_BOUND('',#2911,.T.);
#2387=FACE_OUTER_BOUND('',#2912,.T.);
#2388=FACE_OUTER_BOUND('',#2913,.T.);
#2389=FACE_OUTER_BOUND('',#2914,.T.);
#2390=FACE_OUTER_BOUND('',#2915,.T.);
#2391=FACE_OUTER_BOUND('',#2916,.T.);
#2392=FACE_OUTER_BOUND('',#2917,.T.);
#2393=FACE_OUTER_BOUND('',#2918,.T.);
#2394=FACE_OUTER_BOUND('',#2919,.T.);
#2395=FACE_OUTER_BOUND('',#2920,.T.);
#2396=FACE_OUTER_BOUND('',#2921,.T.);
#2397=FACE_OUTER_BOUND('',#2922,.T.);
#2398=FACE_OUTER_BOUND('',#2923,.T.);
#2399=FACE_OUTER_BOUND('',#2924,.T.);
#2400=FACE_OUTER_BOUND('',#2925,.T.);
#2401=FACE_OUTER_BOUND('',#2926,.T.);
#2402=FACE_OUTER_BOUND('',#2928,.T.);
#2403=FACE_OUTER_BOUND('',#2930,.T.);
#2404=FACE_OUTER_BOUND('',#2931,.T.);
#2405=FACE_OUTER_BOUND('',#2932,.T.);
#2406=FACE_OUTER_BOUND('',#2933,.T.);
#2407=FACE_OUTER_BOUND('',#2934,.T.);
#2408=FACE_OUTER_BOUND('',#2935,.T.);
#2409=FACE_OUTER_BOUND('',#2936,.T.);
#2410=FACE_OUTER_BOUND('',#2937,.T.);
#2411=FACE_OUTER_BOUND('',#2938,.T.);
#2412=FACE_OUTER_BOUND('',#2939,.T.);
#2413=FACE_OUTER_BOUND('',#2940,.T.);
#2414=FACE_OUTER_BOUND('',#2941,.T.);
#2415=FACE_OUTER_BOUND('',#2942,.T.);
#2416=FACE_OUTER_BOUND('',#2943,.T.);
#2417=FACE_OUTER_BOUND('',#2944,.T.);
#2418=FACE_OUTER_BOUND('',#2945,.T.);
#2419=FACE_OUTER_BOUND('',#2946,.T.);
#2420=FACE_OUTER_BOUND('',#2947,.T.);
#2421=FACE_OUTER_BOUND('',#2948,.T.);
#2422=FACE_OUTER_BOUND('',#2949,.T.);
#2423=FACE_OUTER_BOUND('',#2950,.T.);
#2424=FACE_OUTER_BOUND('',#2951,.T.);
#2425=FACE_OUTER_BOUND('',#2952,.T.);
#2426=FACE_OUTER_BOUND('',#2953,.T.);
#2427=FACE_OUTER_BOUND('',#2954,.T.);
#2428=FACE_OUTER_BOUND('',#2955,.T.);
#2429=FACE_OUTER_BOUND('',#2956,.T.);
#2430=FACE_OUTER_BOUND('',#2957,.T.);
#2431=FACE_OUTER_BOUND('',#2958,.T.);
#2432=FACE_OUTER_BOUND('',#2959,.T.);
#2433=FACE_OUTER_BOUND('',#2960,.T.);
#2434=FACE_OUTER_BOUND('',#2961,.T.);
#2435=FACE_OUTER_BOUND('',#2962,.T.);
#2436=FACE_OUTER_BOUND('',#2963,.T.);
#2437=FACE_OUTER_BOUND('',#2964,.T.);
#2438=FACE_OUTER_BOUND('',#2965,.T.);
#2439=FACE_OUTER_BOUND('',#2966,.T.);
#2440=FACE_OUTER_BOUND('',#2967,.T.);
#2441=FACE_OUTER_BOUND('',#2968,.T.);
#2442=FACE_OUTER_BOUND('',#2969,.T.);
#2443=FACE_OUTER_BOUND('',#2970,.T.);
#2444=FACE_OUTER_BOUND('',#2971,.T.);
#2445=FACE_OUTER_BOUND('',#2972,.T.);
#2446=FACE_OUTER_BOUND('',#2973,.T.);
#2447=FACE_OUTER_BOUND('',#2974,.T.);
#2448=FACE_OUTER_BOUND('',#2975,.T.);
#2449=FACE_OUTER_BOUND('',#2976,.T.);
#2450=FACE_OUTER_BOUND('',#2977,.T.);
#2451=FACE_OUTER_BOUND('',#2978,.T.);
#2452=FACE_OUTER_BOUND('',#2979,.T.);
#2453=FACE_OUTER_BOUND('',#2980,.T.);
#2454=FACE_OUTER_BOUND('',#2981,.T.);
#2455=FACE_OUTER_BOUND('',#2982,.T.);
#2456=FACE_OUTER_BOUND('',#2983,.T.);
#2457=FACE_OUTER_BOUND('',#2984,.T.);
#2458=FACE_OUTER_BOUND('',#2985,.T.);
#2459=FACE_OUTER_BOUND('',#2986,.T.);
#2460=FACE_OUTER_BOUND('',#2987,.T.);
#2461=FACE_OUTER_BOUND('',#2988,.T.);
#2462=FACE_OUTER_BOUND('',#2989,.T.);
#2463=FACE_OUTER_BOUND('',#2990,.T.);
#2464=FACE_OUTER_BOUND('',#2991,.T.);
#2465=FACE_OUTER_BOUND('',#2992,.T.);
#2466=FACE_OUTER_BOUND('',#2993,.T.);
#2467=FACE_OUTER_BOUND('',#2994,.T.);
#2468=FACE_OUTER_BOUND('',#2995,.T.);
#2469=FACE_OUTER_BOUND('',#2998,.T.);
#2470=FACE_OUTER_BOUND('',#3001,.T.);
#2471=FACE_OUTER_BOUND('',#3002,.T.);
#2472=FACE_OUTER_BOUND('',#3003,.T.);
#2473=FACE_OUTER_BOUND('',#3004,.T.);
#2474=FACE_OUTER_BOUND('',#3005,.T.);
#2475=FACE_OUTER_BOUND('',#3006,.T.);
#2476=FACE_OUTER_BOUND('',#3007,.T.);
#2477=FACE_OUTER_BOUND('',#3009,.T.);
#2478=FACE_OUTER_BOUND('',#3011,.T.);
#2479=FACE_OUTER_BOUND('',#3012,.T.);
#2480=FACE_OUTER_BOUND('',#3013,.T.);
#2481=FACE_OUTER_BOUND('',#3016,.T.);
#2482=FACE_OUTER_BOUND('',#3019,.T.);
#2483=FACE_OUTER_BOUND('',#3020,.T.);
#2484=FACE_OUTER_BOUND('',#3021,.T.);
#2485=FACE_OUTER_BOUND('',#3022,.T.);
#2486=FACE_OUTER_BOUND('',#3023,.T.);
#2487=FACE_OUTER_BOUND('',#3024,.T.);
#2488=FACE_OUTER_BOUND('',#3025,.T.);
#2489=FACE_OUTER_BOUND('',#3026,.T.);
#2490=FACE_OUTER_BOUND('',#3027,.T.);
#2491=FACE_OUTER_BOUND('',#3028,.T.);
#2492=FACE_OUTER_BOUND('',#3029,.T.);
#2493=FACE_OUTER_BOUND('',#3030,.T.);
#2494=FACE_OUTER_BOUND('',#3031,.T.);
#2495=FACE_OUTER_BOUND('',#3032,.T.);
#2496=FACE_OUTER_BOUND('',#3033,.T.);
#2497=FACE_OUTER_BOUND('',#3034,.T.);
#2498=FACE_OUTER_BOUND('',#3035,.T.);
#2499=FACE_OUTER_BOUND('',#3036,.T.);
#2500=FACE_OUTER_BOUND('',#3037,.T.);
#2501=FACE_OUTER_BOUND('',#3038,.T.);
#2502=FACE_OUTER_BOUND('',#3039,.T.);
#2503=FACE_OUTER_BOUND('',#3040,.T.);
#2504=FACE_OUTER_BOUND('',#3041,.T.);
#2505=FACE_OUTER_BOUND('',#3042,.T.);
#2506=FACE_OUTER_BOUND('',#3043,.T.);
#2507=FACE_OUTER_BOUND('',#3045,.T.);
#2508=FACE_OUTER_BOUND('',#3047,.T.);
#2509=FACE_OUTER_BOUND('',#3048,.T.);
#2510=FACE_OUTER_BOUND('',#3049,.T.);
#2511=FACE_OUTER_BOUND('',#3050,.T.);
#2512=FACE_OUTER_BOUND('',#3052,.T.);
#2513=FACE_OUTER_BOUND('',#3054,.T.);
#2514=FACE_OUTER_BOUND('',#3055,.T.);
#2515=FACE_OUTER_BOUND('',#3056,.T.);
#2516=FACE_OUTER_BOUND('',#3057,.T.);
#2517=FACE_OUTER_BOUND('',#3059,.T.);
#2518=FACE_OUTER_BOUND('',#3061,.T.);
#2519=FACE_OUTER_BOUND('',#3062,.T.);
#2520=FACE_OUTER_BOUND('',#3063,.T.);
#2521=FACE_OUTER_BOUND('',#3064,.T.);
#2522=FACE_OUTER_BOUND('',#3065,.T.);
#2523=FACE_OUTER_BOUND('',#3066,.T.);
#2524=FACE_OUTER_BOUND('',#3067,.T.);
#2525=FACE_OUTER_BOUND('',#3069,.T.);
#2526=FACE_OUTER_BOUND('',#3071,.T.);
#2527=FACE_OUTER_BOUND('',#3072,.T.);
#2528=FACE_OUTER_BOUND('',#3073,.T.);
#2529=FACE_OUTER_BOUND('',#3074,.T.);
#2530=FACE_OUTER_BOUND('',#3075,.T.);
#2531=FACE_OUTER_BOUND('',#3076,.T.);
#2532=FACE_OUTER_BOUND('',#3077,.T.);
#2533=FACE_OUTER_BOUND('',#3078,.T.);
#2534=FACE_OUTER_BOUND('',#3079,.T.);
#2535=FACE_OUTER_BOUND('',#3080,.T.);
#2536=FACE_OUTER_BOUND('',#3081,.T.);
#2537=FACE_OUTER_BOUND('',#3082,.T.);
#2538=FACE_OUTER_BOUND('',#3083,.T.);
#2539=FACE_OUTER_BOUND('',#3084,.T.);
#2540=FACE_OUTER_BOUND('',#3085,.T.);
#2541=FACE_OUTER_BOUND('',#3086,.T.);
#2542=FACE_OUTER_BOUND('',#3087,.T.);
#2543=FACE_OUTER_BOUND('',#3088,.T.);
#2544=FACE_OUTER_BOUND('',#3089,.T.);
#2545=FACE_OUTER_BOUND('',#3090,.T.);
#2546=FACE_OUTER_BOUND('',#3091,.T.);
#2547=FACE_OUTER_BOUND('',#3092,.T.);
#2548=FACE_OUTER_BOUND('',#3093,.T.);
#2549=FACE_OUTER_BOUND('',#3094,.T.);
#2550=FACE_OUTER_BOUND('',#3095,.T.);
#2551=FACE_OUTER_BOUND('',#3096,.T.);
#2552=FACE_OUTER_BOUND('',#3097,.T.);
#2553=FACE_OUTER_BOUND('',#3100,.T.);
#2554=FACE_OUTER_BOUND('',#3103,.T.);
#2555=FACE_OUTER_BOUND('',#3104,.T.);
#2556=FACE_OUTER_BOUND('',#3105,.T.);
#2557=FACE_OUTER_BOUND('',#3106,.T.);
#2558=FACE_OUTER_BOUND('',#3107,.T.);
#2559=FACE_OUTER_BOUND('',#3108,.T.);
#2560=FACE_OUTER_BOUND('',#3109,.T.);
#2561=FACE_OUTER_BOUND('',#3110,.T.);
#2562=FACE_OUTER_BOUND('',#3111,.T.);
#2563=FACE_OUTER_BOUND('',#3112,.T.);
#2564=FACE_OUTER_BOUND('',#3113,.T.);
#2565=FACE_OUTER_BOUND('',#3114,.T.);
#2566=FACE_OUTER_BOUND('',#3115,.T.);
#2567=FACE_OUTER_BOUND('',#3116,.T.);
#2568=FACE_OUTER_BOUND('',#3117,.T.);
#2569=FACE_OUTER_BOUND('',#3118,.T.);
#2570=FACE_OUTER_BOUND('',#3119,.T.);
#2571=FACE_OUTER_BOUND('',#3120,.T.);
#2572=FACE_OUTER_BOUND('',#3121,.T.);
#2573=FACE_OUTER_BOUND('',#3122,.T.);
#2574=FACE_OUTER_BOUND('',#3123,.T.);
#2575=EDGE_LOOP('',(#5727));
#2576=EDGE_LOOP('',(#5728,#5729,#5730,#5731));
#2577=EDGE_LOOP('',(#5732));
#2578=EDGE_LOOP('',(#5733));
#2579=EDGE_LOOP('',(#5734));
#2580=EDGE_LOOP('',(#5735));
#2581=EDGE_LOOP('',(#5736));
#2582=EDGE_LOOP('',(#5737,#5738,#5739,#5740,#5741,#5742));
#2583=EDGE_LOOP('',(#5743,#5744,#5745,#5746,#5747));
#2584=EDGE_LOOP('',(#5748,#5749,#5750,#5751,#5752));
#2585=EDGE_LOOP('',(#5753,#5754,#5755,#5756,#5757));
#2586=EDGE_LOOP('',(#5758,#5759,#5760,#5761,#5762,#5763,#5764));
#2587=EDGE_LOOP('',(#5765,#5766,#5767,#5768));
#2588=EDGE_LOOP('',(#5769,#5770,#5771,#5772));
#2589=EDGE_LOOP('',(#5773,#5774,#5775,#5776));
#2590=EDGE_LOOP('',(#5777,#5778,#5779,#5780,#5781));
#2591=EDGE_LOOP('',(#5782,#5783,#5784,#5785,#5786));
#2592=EDGE_LOOP('',(#5787,#5788,#5789,#5790));
#2593=EDGE_LOOP('',(#5791,#5792,#5793,#5794));
#2594=EDGE_LOOP('',(#5795));
#2595=EDGE_LOOP('',(#5796));
#2596=EDGE_LOOP('',(#5797));
#2597=EDGE_LOOP('',(#5798,#5799,#5800,#5801));
#2598=EDGE_LOOP('',(#5802));
#2599=EDGE_LOOP('',(#5803));
#2600=EDGE_LOOP('',(#5804));
#2601=EDGE_LOOP('',(#5805));
#2602=EDGE_LOOP('',(#5806));
#2603=EDGE_LOOP('',(#5807,#5808,#5809,#5810,#5811,#5812,#5813,#5814,#5815));
#2604=EDGE_LOOP('',(#5816,#5817,#5818,#5819));
#2605=EDGE_LOOP('',(#5820,#5821,#5822,#5823));
#2606=EDGE_LOOP('',(#5824,#5825,#5826,#5827));
#2607=EDGE_LOOP('',(#5828,#5829,#5830,#5831));
#2608=EDGE_LOOP('',(#5832,#5833,#5834,#5835));
#2609=EDGE_LOOP('',(#5836,#5837,#5838,#5839));
#2610=EDGE_LOOP('',(#5840,#5841,#5842,#5843));
#2611=EDGE_LOOP('',(#5844,#5845,#5846,#5847));
#2612=EDGE_LOOP('',(#5848,#5849,#5850,#5851,#5852,#5853));
#2613=EDGE_LOOP('',(#5854,#5855,#5856,#5857,#5858,#5859));
#2614=EDGE_LOOP('',(#5860,#5861,#5862,#5863,#5864,#5865,#5866,#5867,#5868,
#5869,#5870,#5871,#5872,#5873));
#2615=EDGE_LOOP('',(#5874,#5875,#5876,#5877));
#2616=EDGE_LOOP('',(#5878,#5879,#5880,#5881,#5882));
#2617=EDGE_LOOP('',(#5883,#5884,#5885,#5886));
#2618=EDGE_LOOP('',(#5887,#5888,#5889,#5890));
#2619=EDGE_LOOP('',(#5891,#5892,#5893,#5894));
#2620=EDGE_LOOP('',(#5895,#5896,#5897,#5898));
#2621=EDGE_LOOP('',(#5899,#5900,#5901,#5902));
#2622=EDGE_LOOP('',(#5903,#5904,#5905,#5906));
#2623=EDGE_LOOP('',(#5907,#5908,#5909,#5910));
#2624=EDGE_LOOP('',(#5911,#5912,#5913,#5914));
#2625=EDGE_LOOP('',(#5915,#5916,#5917,#5918));
#2626=EDGE_LOOP('',(#5919,#5920,#5921,#5922));
#2627=EDGE_LOOP('',(#5923,#5924,#5925,#5926));
#2628=EDGE_LOOP('',(#5927,#5928,#5929,#5930));
#2629=EDGE_LOOP('',(#5931,#5932,#5933,#5934));
#2630=EDGE_LOOP('',(#5935,#5936,#5937,#5938,#5939,#5940,#5941,#5942,#5943,
#5944,#5945,#5946,#5947,#5948,#5949,#5950,#5951,#5952,#5953,#5954,#5955,
#5956,#5957,#5958,#5959,#5960,#5961,#5962,#5963,#5964,#5965,#5966,#5967,
#5968,#5969,#5970,#5971,#5972,#5973,#5974,#5975,#5976,#5977,#5978,#5979));
#2631=EDGE_LOOP('',(#5980));
#2632=EDGE_LOOP('',(#5981,#5982,#5983,#5984));
#2633=EDGE_LOOP('',(#5985,#5986,#5987,#5988));
#2634=EDGE_LOOP('',(#5989,#5990,#5991,#5992));
#2635=EDGE_LOOP('',(#5993,#5994,#5995,#5996));
#2636=EDGE_LOOP('',(#5997,#5998,#5999,#6000));
#2637=EDGE_LOOP('',(#6001,#6002,#6003,#6004));
#2638=EDGE_LOOP('',(#6005,#6006,#6007,#6008));
#2639=EDGE_LOOP('',(#6009,#6010,#6011,#6012));
#2640=EDGE_LOOP('',(#6013,#6014,#6015,#6016));
#2641=EDGE_LOOP('',(#6017,#6018,#6019,#6020));
#2642=EDGE_LOOP('',(#6021,#6022,#6023,#6024));
#2643=EDGE_LOOP('',(#6025,#6026,#6027,#6028));
#2644=EDGE_LOOP('',(#6029,#6030,#6031,#6032));
#2645=EDGE_LOOP('',(#6033,#6034,#6035,#6036));
#2646=EDGE_LOOP('',(#6037,#6038,#6039,#6040));
#2647=EDGE_LOOP('',(#6041,#6042,#6043,#6044));
#2648=EDGE_LOOP('',(#6045,#6046,#6047,#6048));
#2649=EDGE_LOOP('',(#6049,#6050,#6051,#6052));
#2650=EDGE_LOOP('',(#6053,#6054,#6055));
#2651=EDGE_LOOP('',(#6056,#6057,#6058,#6059));
#2652=EDGE_LOOP('',(#6060,#6061,#6062,#6063));
#2653=EDGE_LOOP('',(#6064,#6065,#6066,#6067));
#2654=EDGE_LOOP('',(#6068,#6069,#6070,#6071));
#2655=EDGE_LOOP('',(#6072,#6073,#6074,#6075,#6076,#6077,#6078));
#2656=EDGE_LOOP('',(#6079,#6080,#6081,#6082,#6083,#6084,#6085,#6086,#6087,
#6088,#6089,#6090,#6091,#6092));
#2657=EDGE_LOOP('',(#6093,#6094,#6095,#6096));
#2658=EDGE_LOOP('',(#6097,#6098,#6099,#6100));
#2659=EDGE_LOOP('',(#6101,#6102,#6103,#6104,#6105,#6106,#6107,#6108,#6109,
#6110,#6111,#6112,#6113,#6114,#6115,#6116,#6117,#6118,#6119));
#2660=EDGE_LOOP('',(#6120,#6121,#6122,#6123));
#2661=EDGE_LOOP('',(#6124,#6125,#6126,#6127));
#2662=EDGE_LOOP('',(#6128,#6129,#6130,#6131));
#2663=EDGE_LOOP('',(#6132,#6133,#6134,#6135));
#2664=EDGE_LOOP('',(#6136,#6137,#6138,#6139,#6140,#6141,#6142));
#2665=EDGE_LOOP('',(#6143));
#2666=EDGE_LOOP('',(#6144,#6145,#6146,#6147,#6148,#6149,#6150));
#2667=EDGE_LOOP('',(#6151));
#2668=EDGE_LOOP('',(#6152,#6153,#6154,#6155));
#2669=EDGE_LOOP('',(#6156,#6157,#6158,#6159));
#2670=EDGE_LOOP('',(#6160,#6161,#6162,#6163));
#2671=EDGE_LOOP('',(#6164,#6165,#6166,#6167));
#2672=EDGE_LOOP('',(#6168,#6169,#6170,#6171,#6172,#6173,#6174,#6175,#6176,
#6177,#6178,#6179,#6180,#6181,#6182,#6183,#6184,#6185,#6186,#6187,#6188,
#6189,#6190,#6191,#6192,#6193,#6194,#6195,#6196,#6197,#6198,#6199,#6200,
#6201,#6202,#6203,#6204,#6205,#6206,#6207,#6208,#6209,#6210,#6211,#6212,
#6213));
#2673=EDGE_LOOP('',(#6214));
#2674=EDGE_LOOP('',(#6215,#6216,#6217,#6218,#6219));
#2675=EDGE_LOOP('',(#6220,#6221,#6222));
#2676=EDGE_LOOP('',(#6223,#6224,#6225,#6226,#6227,#6228));
#2677=EDGE_LOOP('',(#6229,#6230,#6231,#6232,#6233,#6234,#6235));
#2678=EDGE_LOOP('',(#6236,#6237,#6238,#6239,#6240,#6241,#6242,#6243,#6244,
#6245));
#2679=EDGE_LOOP('',(#6246,#6247,#6248,#6249,#6250,#6251));
#2680=EDGE_LOOP('',(#6252,#6253,#6254,#6255));
#2681=EDGE_LOOP('',(#6256,#6257,#6258,#6259,#6260,#6261,#6262,#6263,#6264,
#6265));
#2682=EDGE_LOOP('',(#6266,#6267,#6268,#6269,#6270,#6271,#6272,#6273,#6274,
#6275,#6276,#6277,#6278,#6279,#6280,#6281,#6282,#6283,#6284,#6285,#6286,
#6287,#6288,#6289,#6290,#6291,#6292));
#2683=EDGE_LOOP('',(#6293,#6294,#6295,#6296));
#2684=EDGE_LOOP('',(#6297,#6298,#6299,#6300));
#2685=EDGE_LOOP('',(#6301,#6302,#6303,#6304,#6305,#6306,#6307,#6308,#6309,
#6310,#6311,#6312,#6313,#6314,#6315,#6316,#6317,#6318,#6319,#6320,#6321,
#6322,#6323,#6324,#6325,#6326,#6327));
#2686=EDGE_LOOP('',(#6328,#6329,#6330,#6331));
#2687=EDGE_LOOP('',(#6332,#6333,#6334,#6335));
#2688=EDGE_LOOP('',(#6336,#6337,#6338,#6339));
#2689=EDGE_LOOP('',(#6340,#6341,#6342,#6343));
#2690=EDGE_LOOP('',(#6344,#6345,#6346,#6347));
#2691=EDGE_LOOP('',(#6348,#6349,#6350,#6351));
#2692=EDGE_LOOP('',(#6352,#6353,#6354,#6355));
#2693=EDGE_LOOP('',(#6356,#6357,#6358,#6359));
#2694=EDGE_LOOP('',(#6360,#6361,#6362,#6363));
#2695=EDGE_LOOP('',(#6364,#6365,#6366,#6367));
#2696=EDGE_LOOP('',(#6368,#6369,#6370,#6371));
#2697=EDGE_LOOP('',(#6372,#6373,#6374,#6375));
#2698=EDGE_LOOP('',(#6376,#6377,#6378,#6379));
#2699=EDGE_LOOP('',(#6380,#6381,#6382,#6383));
#2700=EDGE_LOOP('',(#6384,#6385,#6386,#6387));
#2701=EDGE_LOOP('',(#6388,#6389,#6390,#6391));
#2702=EDGE_LOOP('',(#6392,#6393,#6394,#6395));
#2703=EDGE_LOOP('',(#6396,#6397,#6398,#6399));
#2704=EDGE_LOOP('',(#6400,#6401,#6402,#6403));
#2705=EDGE_LOOP('',(#6404,#6405,#6406,#6407));
#2706=EDGE_LOOP('',(#6408,#6409,#6410,#6411));
#2707=EDGE_LOOP('',(#6412,#6413,#6414,#6415,#6416));
#2708=EDGE_LOOP('',(#6417,#6418,#6419));
#2709=EDGE_LOOP('',(#6420,#6421,#6422,#6423,#6424));
#2710=EDGE_LOOP('',(#6425,#6426,#6427));
#2711=EDGE_LOOP('',(#6428,#6429,#6430,#6431));
#2712=EDGE_LOOP('',(#6432,#6433,#6434,#6435));
#2713=EDGE_LOOP('',(#6436,#6437,#6438,#6439,#6440));
#2714=EDGE_LOOP('',(#6441,#6442,#6443,#6444));
#2715=EDGE_LOOP('',(#6445,#6446,#6447,#6448));
#2716=EDGE_LOOP('',(#6449,#6450,#6451,#6452,#6453));
#2717=EDGE_LOOP('',(#6454,#6455));
#2718=EDGE_LOOP('',(#6456,#6457,#6458));
#2719=EDGE_LOOP('',(#6459,#6460,#6461));
#2720=EDGE_LOOP('',(#6462,#6463));
#2721=EDGE_LOOP('',(#6464,#6465,#6466,#6467));
#2722=EDGE_LOOP('',(#6468,#6469,#6470,#6471));
#2723=EDGE_LOOP('',(#6472,#6473,#6474,#6475));
#2724=EDGE_LOOP('',(#6476,#6477,#6478,#6479));
#2725=EDGE_LOOP('',(#6480,#6481,#6482,#6483));
#2726=EDGE_LOOP('',(#6484,#6485,#6486,#6487));
#2727=EDGE_LOOP('',(#6488,#6489,#6490,#6491));
#2728=EDGE_LOOP('',(#6492,#6493,#6494,#6495));
#2729=EDGE_LOOP('',(#6496,#6497,#6498,#6499));
#2730=EDGE_LOOP('',(#6500,#6501,#6502,#6503));
#2731=EDGE_LOOP('',(#6504,#6505,#6506,#6507));
#2732=EDGE_LOOP('',(#6508,#6509,#6510,#6511));
#2733=EDGE_LOOP('',(#6512,#6513,#6514,#6515));
#2734=EDGE_LOOP('',(#6516,#6517,#6518,#6519));
#2735=EDGE_LOOP('',(#6520,#6521,#6522,#6523));
#2736=EDGE_LOOP('',(#6524,#6525,#6526,#6527));
#2737=EDGE_LOOP('',(#6528,#6529,#6530,#6531));
#2738=EDGE_LOOP('',(#6532,#6533,#6534,#6535,#6536,#6537,#6538,#6539,#6540));
#2739=EDGE_LOOP('',(#6541,#6542,#6543,#6544));
#2740=EDGE_LOOP('',(#6545,#6546,#6547,#6548,#6549,#6550));
#2741=EDGE_LOOP('',(#6551,#6552,#6553,#6554));
#2742=EDGE_LOOP('',(#6555,#6556));
#2743=EDGE_LOOP('',(#6557,#6558,#6559,#6560));
#2744=EDGE_LOOP('',(#6561,#6562,#6563,#6564));
#2745=EDGE_LOOP('',(#6565,#6566,#6567,#6568,#6569,#6570,#6571,#6572));
#2746=EDGE_LOOP('',(#6573,#6574,#6575,#6576,#6577,#6578,#6579));
#2747=EDGE_LOOP('',(#6580,#6581,#6582,#6583,#6584));
#2748=EDGE_LOOP('',(#6585,#6586,#6587,#6588,#6589,#6590,#6591,#6592));
#2749=EDGE_LOOP('',(#6593,#6594,#6595,#6596,#6597,#6598,#6599,#6600));
#2750=EDGE_LOOP('',(#6601,#6602,#6603,#6604));
#2751=EDGE_LOOP('',(#6605,#6606,#6607,#6608,#6609,#6610,#6611,#6612));
#2752=EDGE_LOOP('',(#6613,#6614,#6615,#6616,#6617,#6618,#6619,#6620));
#2753=EDGE_LOOP('',(#6621,#6622,#6623,#6624));
#2754=EDGE_LOOP('',(#6625,#6626,#6627,#6628,#6629,#6630,#6631,#6632));
#2755=EDGE_LOOP('',(#6633,#6634,#6635,#6636,#6637,#6638,#6639,#6640));
#2756=EDGE_LOOP('',(#6641,#6642,#6643,#6644));
#2757=EDGE_LOOP('',(#6645,#6646,#6647,#6648,#6649,#6650,#6651,#6652));
#2758=EDGE_LOOP('',(#6653,#6654,#6655,#6656,#6657,#6658,#6659,#6660));
#2759=EDGE_LOOP('',(#6661,#6662,#6663,#6664));
#2760=EDGE_LOOP('',(#6665,#6666,#6667,#6668,#6669,#6670,#6671,#6672));
#2761=EDGE_LOOP('',(#6673,#6674,#6675,#6676,#6677,#6678,#6679,#6680));
#2762=EDGE_LOOP('',(#6681,#6682,#6683,#6684));
#2763=EDGE_LOOP('',(#6685,#6686,#6687,#6688,#6689));
#2764=EDGE_LOOP('',(#6690,#6691,#6692));
#2765=EDGE_LOOP('',(#6693,#6694,#6695,#6696));
#2766=EDGE_LOOP('',(#6697,#6698,#6699,#6700));
#2767=EDGE_LOOP('',(#6701,#6702,#6703,#6704));
#2768=EDGE_LOOP('',(#6705,#6706,#6707,#6708));
#2769=EDGE_LOOP('',(#6709,#6710,#6711,#6712));
#2770=EDGE_LOOP('',(#6713,#6714,#6715,#6716,#6717));
#2771=EDGE_LOOP('',(#6718,#6719,#6720,#6721,#6722));
#2772=EDGE_LOOP('',(#6723,#6724,#6725,#6726));
#2773=EDGE_LOOP('',(#6727,#6728,#6729,#6730));
#2774=EDGE_LOOP('',(#6731,#6732,#6733,#6734));
#2775=EDGE_LOOP('',(#6735,#6736,#6737,#6738));
#2776=EDGE_LOOP('',(#6739,#6740,#6741));
#2777=EDGE_LOOP('',(#6742,#6743,#6744,#6745,#6746));
#2778=EDGE_LOOP('',(#6747,#6748,#6749,#6750));
#2779=EDGE_LOOP('',(#6751,#6752,#6753,#6754));
#2780=EDGE_LOOP('',(#6755,#6756,#6757,#6758));
#2781=EDGE_LOOP('',(#6759,#6760,#6761,#6762));
#2782=EDGE_LOOP('',(#6763,#6764,#6765,#6766));
#2783=EDGE_LOOP('',(#6767,#6768,#6769,#6770));
#2784=EDGE_LOOP('',(#6771,#6772,#6773,#6774));
#2785=EDGE_LOOP('',(#6775,#6776,#6777,#6778));
#2786=EDGE_LOOP('',(#6779,#6780,#6781,#6782));
#2787=EDGE_LOOP('',(#6783,#6784,#6785,#6786));
#2788=EDGE_LOOP('',(#6787,#6788,#6789,#6790));
#2789=EDGE_LOOP('',(#6791,#6792,#6793,#6794));
#2790=EDGE_LOOP('',(#6795,#6796,#6797,#6798));
#2791=EDGE_LOOP('',(#6799,#6800,#6801,#6802));
#2792=EDGE_LOOP('',(#6803,#6804,#6805,#6806));
#2793=EDGE_LOOP('',(#6807,#6808,#6809,#6810));
#2794=EDGE_LOOP('',(#6811,#6812,#6813,#6814));
#2795=EDGE_LOOP('',(#6815,#6816,#6817,#6818));
#2796=EDGE_LOOP('',(#6819,#6820,#6821,#6822));
#2797=EDGE_LOOP('',(#6823,#6824,#6825,#6826));
#2798=EDGE_LOOP('',(#6827,#6828,#6829,#6830));
#2799=EDGE_LOOP('',(#6831,#6832,#6833,#6834));
#2800=EDGE_LOOP('',(#6835,#6836,#6837,#6838));
#2801=EDGE_LOOP('',(#6839,#6840,#6841,#6842));
#2802=EDGE_LOOP('',(#6843,#6844,#6845,#6846));
#2803=EDGE_LOOP('',(#6847,#6848,#6849,#6850));
#2804=EDGE_LOOP('',(#6851,#6852,#6853,#6854));
#2805=EDGE_LOOP('',(#6855,#6856,#6857,#6858));
#2806=EDGE_LOOP('',(#6859,#6860,#6861,#6862));
#2807=EDGE_LOOP('',(#6863,#6864,#6865,#6866));
#2808=EDGE_LOOP('',(#6867,#6868,#6869,#6870));
#2809=EDGE_LOOP('',(#6871,#6872,#6873,#6874));
#2810=EDGE_LOOP('',(#6875,#6876,#6877,#6878));
#2811=EDGE_LOOP('',(#6879,#6880,#6881,#6882));
#2812=EDGE_LOOP('',(#6883,#6884,#6885,#6886));
#2813=EDGE_LOOP('',(#6887,#6888,#6889,#6890));
#2814=EDGE_LOOP('',(#6891,#6892,#6893,#6894));
#2815=EDGE_LOOP('',(#6895,#6896,#6897,#6898));
#2816=EDGE_LOOP('',(#6899,#6900,#6901,#6902,#6903));
#2817=EDGE_LOOP('',(#6904,#6905,#6906,#6907,#6908,#6909));
#2818=EDGE_LOOP('',(#6910,#6911,#6912,#6913));
#2819=EDGE_LOOP('',(#6914,#6915,#6916,#6917));
#2820=EDGE_LOOP('',(#6918,#6919,#6920,#6921));
#2821=EDGE_LOOP('',(#6922,#6923,#6924,#6925));
#2822=EDGE_LOOP('',(#6926,#6927,#6928,#6929));
#2823=EDGE_LOOP('',(#6930,#6931,#6932,#6933));
#2824=EDGE_LOOP('',(#6934,#6935,#6936,#6937));
#2825=EDGE_LOOP('',(#6938,#6939,#6940,#6941));
#2826=EDGE_LOOP('',(#6942,#6943,#6944,#6945));
#2827=EDGE_LOOP('',(#6946,#6947,#6948,#6949));
#2828=EDGE_LOOP('',(#6950,#6951,#6952,#6953,#6954,#6955,#6956,#6957,#6958,
#6959,#6960,#6961,#6962,#6963,#6964,#6965,#6966,#6967,#6968,#6969,#6970,
#6971,#6972,#6973,#6974,#6975,#6976,#6977,#6978,#6979,#6980,#6981,#6982,
#6983,#6984,#6985,#6986,#6987,#6988,#6989,#6990,#6991,#6992,#6993,#6994,
#6995,#6996,#6997,#6998,#6999,#7000,#7001,#7002,#7003,#7004,#7005));
#2829=EDGE_LOOP('',(#7006,#7007,#7008,#7009,#7010,#7011,#7012,#7013,#7014,
#7015,#7016,#7017,#7018,#7019,#7020,#7021,#7022,#7023,#7024,#7025,#7026,
#7027,#7028,#7029,#7030,#7031,#7032,#7033,#7034,#7035,#7036,#7037,#7038,
#7039,#7040,#7041,#7042,#7043,#7044,#7045,#7046,#7047,#7048,#7049,#7050,
#7051,#7052,#7053,#7054,#7055,#7056,#7057,#7058,#7059,#7060,#7061));
#2830=EDGE_LOOP('',(#7062,#7063,#7064));
#2831=EDGE_LOOP('',(#7065,#7066,#7067,#7068,#7069));
#2832=EDGE_LOOP('',(#7070,#7071,#7072,#7073));
#2833=EDGE_LOOP('',(#7074,#7075,#7076,#7077));
#2834=EDGE_LOOP('',(#7078,#7079,#7080,#7081));
#2835=EDGE_LOOP('',(#7082,#7083,#7084,#7085));
#2836=EDGE_LOOP('',(#7086,#7087,#7088,#7089));
#2837=EDGE_LOOP('',(#7090,#7091,#7092,#7093));
#2838=EDGE_LOOP('',(#7094,#7095,#7096,#7097));
#2839=EDGE_LOOP('',(#7098,#7099,#7100,#7101));
#2840=EDGE_LOOP('',(#7102,#7103,#7104,#7105));
#2841=EDGE_LOOP('',(#7106,#7107,#7108,#7109));
#2842=EDGE_LOOP('',(#7110,#7111,#7112,#7113));
#2843=EDGE_LOOP('',(#7114,#7115,#7116,#7117));
#2844=EDGE_LOOP('',(#7118,#7119,#7120,#7121));
#2845=EDGE_LOOP('',(#7122,#7123,#7124,#7125));
#2846=EDGE_LOOP('',(#7126,#7127,#7128,#7129));
#2847=EDGE_LOOP('',(#7130,#7131,#7132,#7133));
#2848=EDGE_LOOP('',(#7134,#7135,#7136,#7137));
#2849=EDGE_LOOP('',(#7138,#7139,#7140,#7141,#7142));
#2850=EDGE_LOOP('',(#7143,#7144,#7145,#7146));
#2851=EDGE_LOOP('',(#7147,#7148,#7149,#7150));
#2852=EDGE_LOOP('',(#7151,#7152,#7153,#7154));
#2853=EDGE_LOOP('',(#7155,#7156,#7157,#7158));
#2854=EDGE_LOOP('',(#7159,#7160,#7161,#7162));
#2855=EDGE_LOOP('',(#7163,#7164,#7165,#7166));
#2856=EDGE_LOOP('',(#7167));
#2857=EDGE_LOOP('',(#7168,#7169,#7170,#7171,#7172));
#2858=EDGE_LOOP('',(#7173));
#2859=EDGE_LOOP('',(#7174,#7175,#7176,#7177));
#2860=EDGE_LOOP('',(#7178,#7179,#7180,#7181));
#2861=EDGE_LOOP('',(#7182,#7183,#7184,#7185,#7186,#7187,#7188,#7189,#7190,
#7191,#7192,#7193,#7194,#7195,#7196,#7197,#7198,#7199,#7200,#7201,#7202,
#7203,#7204,#7205,#7206,#7207,#7208,#7209,#7210,#7211,#7212,#7213,#7214,
#7215,#7216,#7217,#7218,#7219,#7220,#7221,#7222,#7223,#7224,#7225));
#2862=EDGE_LOOP('',(#7226,#7227,#7228,#7229,#7230,#7231,#7232,#7233,#7234,
#7235,#7236,#7237,#7238,#7239,#7240,#7241,#7242,#7243,#7244,#7245,#7246,
#7247,#7248,#7249,#7250,#7251,#7252,#7253,#7254,#7255,#7256,#7257,#7258,
#7259,#7260,#7261,#7262,#7263,#7264,#7265,#7266,#7267,#7268,#7269));
#2863=EDGE_LOOP('',(#7270,#7271,#7272,#7273));
#2864=EDGE_LOOP('',(#7274,#7275,#7276,#7277));
#2865=EDGE_LOOP('',(#7278,#7279,#7280,#7281));
#2866=EDGE_LOOP('',(#7282,#7283,#7284,#7285));
#2867=EDGE_LOOP('',(#7286,#7287,#7288,#7289));
#2868=EDGE_LOOP('',(#7290,#7291,#7292,#7293));
#2869=EDGE_LOOP('',(#7294,#7295,#7296,#7297));
#2870=EDGE_LOOP('',(#7298,#7299,#7300,#7301));
#2871=EDGE_LOOP('',(#7302,#7303,#7304,#7305));
#2872=EDGE_LOOP('',(#7306,#7307,#7308,#7309));
#2873=EDGE_LOOP('',(#7310,#7311,#7312,#7313));
#2874=EDGE_LOOP('',(#7314,#7315,#7316,#7317));
#2875=EDGE_LOOP('',(#7318,#7319,#7320,#7321));
#2876=EDGE_LOOP('',(#7322,#7323,#7324,#7325));
#2877=EDGE_LOOP('',(#7326,#7327,#7328,#7329));
#2878=EDGE_LOOP('',(#7330,#7331,#7332,#7333));
#2879=EDGE_LOOP('',(#7334,#7335,#7336,#7337));
#2880=EDGE_LOOP('',(#7338));
#2881=EDGE_LOOP('',(#7339,#7340));
#2882=EDGE_LOOP('',(#7341,#7342,#7343,#7344,#7345));
#2883=EDGE_LOOP('',(#7346));
#2884=EDGE_LOOP('',(#7347,#7348,#7349,#7350));
#2885=EDGE_LOOP('',(#7351,#7352,#7353,#7354));
#2886=EDGE_LOOP('',(#7355,#7356,#7357,#7358));
#2887=EDGE_LOOP('',(#7359,#7360,#7361,#7362));
#2888=EDGE_LOOP('',(#7363,#7364,#7365,#7366));
#2889=EDGE_LOOP('',(#7367,#7368,#7369,#7370));
#2890=EDGE_LOOP('',(#7371,#7372,#7373,#7374));
#2891=EDGE_LOOP('',(#7375,#7376,#7377,#7378));
#2892=EDGE_LOOP('',(#7379,#7380,#7381,#7382));
#2893=EDGE_LOOP('',(#7383,#7384,#7385,#7386));
#2894=EDGE_LOOP('',(#7387,#7388,#7389,#7390,#7391,#7392,#7393,#7394,#7395,
#7396));
#2895=EDGE_LOOP('',(#7397,#7398,#7399,#7400));
#2896=EDGE_LOOP('',(#7401,#7402,#7403,#7404));
#2897=EDGE_LOOP('',(#7405,#7406,#7407,#7408,#7409,#7410,#7411,#7412,#7413,
#7414,#7415,#7416));
#2898=EDGE_LOOP('',(#7417));
#2899=EDGE_LOOP('',(#7418));
#2900=EDGE_LOOP('',(#7419,#7420,#7421,#7422,#7423,#7424,#7425,#7426,#7427,
#7428,#7429,#7430));
#2901=EDGE_LOOP('',(#7431));
#2902=EDGE_LOOP('',(#7432));
#2903=EDGE_LOOP('',(#7433,#7434,#7435,#7436,#7437,#7438,#7439,#7440));
#2904=EDGE_LOOP('',(#7441,#7442,#7443,#7444,#7445,#7446,#7447,#7448));
#2905=EDGE_LOOP('',(#7449,#7450,#7451,#7452));
#2906=EDGE_LOOP('',(#7453,#7454,#7455,#7456));
#2907=EDGE_LOOP('',(#7457,#7458,#7459,#7460));
#2908=EDGE_LOOP('',(#7461,#7462,#7463,#7464,#7465,#7466,#7467,#7468,#7469,
#7470));
#2909=EDGE_LOOP('',(#7471,#7472,#7473,#7474));
#2910=EDGE_LOOP('',(#7475,#7476,#7477,#7478,#7479,#7480,#7481,#7482,#7483,
#7484,#7485,#7486,#7487,#7488,#7489,#7490,#7491,#7492,#7493,#7494,#7495,
#7496,#7497,#7498,#7499,#7500,#7501,#7502,#7503));
#2911=EDGE_LOOP('',(#7504,#7505,#7506,#7507));
#2912=EDGE_LOOP('',(#7508,#7509,#7510,#7511));
#2913=EDGE_LOOP('',(#7512,#7513,#7514));
#2914=EDGE_LOOP('',(#7515,#7516,#7517,#7518));
#2915=EDGE_LOOP('',(#7519,#7520,#7521,#7522));
#2916=EDGE_LOOP('',(#7523,#7524,#7525));
#2917=EDGE_LOOP('',(#7526,#7527,#7528,#7529));
#2918=EDGE_LOOP('',(#7530,#7531,#7532,#7533));
#2919=EDGE_LOOP('',(#7534,#7535,#7536,#7537,#7538,#7539,#7540,#7541,#7542,
#7543,#7544,#7545,#7546,#7547,#7548,#7549,#7550,#7551,#7552,#7553,#7554,
#7555,#7556,#7557,#7558,#7559,#7560,#7561,#7562));
#2920=EDGE_LOOP('',(#7563,#7564,#7565,#7566));
#2921=EDGE_LOOP('',(#7567,#7568,#7569,#7570));
#2922=EDGE_LOOP('',(#7571,#7572,#7573,#7574));
#2923=EDGE_LOOP('',(#7575,#7576,#7577,#7578));
#2924=EDGE_LOOP('',(#7579,#7580,#7581,#7582));
#2925=EDGE_LOOP('',(#7583,#7584,#7585,#7586));
#2926=EDGE_LOOP('',(#7587,#7588,#7589,#7590,#7591,#7592));
#2927=EDGE_LOOP('',(#7593));
#2928=EDGE_LOOP('',(#7594,#7595,#7596,#7597,#7598,#7599));
#2929=EDGE_LOOP('',(#7600));
#2930=EDGE_LOOP('',(#7601,#7602,#7603,#7604));
#2931=EDGE_LOOP('',(#7605,#7606,#7607,#7608));
#2932=EDGE_LOOP('',(#7609,#7610,#7611,#7612));
#2933=EDGE_LOOP('',(#7613,#7614,#7615,#7616));
#2934=EDGE_LOOP('',(#7617,#7618,#7619,#7620));
#2935=EDGE_LOOP('',(#7621,#7622,#7623,#7624));
#2936=EDGE_LOOP('',(#7625,#7626,#7627,#7628));
#2937=EDGE_LOOP('',(#7629,#7630,#7631,#7632));
#2938=EDGE_LOOP('',(#7633,#7634,#7635,#7636));
#2939=EDGE_LOOP('',(#7637,#7638,#7639,#7640));
#2940=EDGE_LOOP('',(#7641,#7642,#7643,#7644));
#2941=EDGE_LOOP('',(#7645,#7646,#7647,#7648));
#2942=EDGE_LOOP('',(#7649,#7650,#7651,#7652));
#2943=EDGE_LOOP('',(#7653,#7654,#7655,#7656));
#2944=EDGE_LOOP('',(#7657,#7658,#7659,#7660));
#2945=EDGE_LOOP('',(#7661,#7662,#7663,#7664));
#2946=EDGE_LOOP('',(#7665,#7666,#7667,#7668));
#2947=EDGE_LOOP('',(#7669,#7670,#7671,#7672));
#2948=EDGE_LOOP('',(#7673,#7674,#7675,#7676));
#2949=EDGE_LOOP('',(#7677,#7678,#7679,#7680));
#2950=EDGE_LOOP('',(#7681,#7682,#7683,#7684));
#2951=EDGE_LOOP('',(#7685,#7686,#7687,#7688));
#2952=EDGE_LOOP('',(#7689,#7690,#7691,#7692));
#2953=EDGE_LOOP('',(#7693,#7694,#7695,#7696));
#2954=EDGE_LOOP('',(#7697,#7698,#7699,#7700));
#2955=EDGE_LOOP('',(#7701,#7702,#7703,#7704));
#2956=EDGE_LOOP('',(#7705,#7706,#7707,#7708,#7709));
#2957=EDGE_LOOP('',(#7710,#7711,#7712,#7713));
#2958=EDGE_LOOP('',(#7714,#7715,#7716,#7717));
#2959=EDGE_LOOP('',(#7718,#7719,#7720,#7721));
#2960=EDGE_LOOP('',(#7722,#7723,#7724,#7725));
#2961=EDGE_LOOP('',(#7726,#7727,#7728,#7729));
#2962=EDGE_LOOP('',(#7730,#7731,#7732,#7733));
#2963=EDGE_LOOP('',(#7734,#7735,#7736,#7737,#7738));
#2964=EDGE_LOOP('',(#7739,#7740,#7741,#7742));
#2965=EDGE_LOOP('',(#7743,#7744,#7745,#7746));
#2966=EDGE_LOOP('',(#7747,#7748,#7749,#7750));
#2967=EDGE_LOOP('',(#7751,#7752,#7753,#7754));
#2968=EDGE_LOOP('',(#7755,#7756,#7757,#7758));
#2969=EDGE_LOOP('',(#7759,#7760,#7761));
#2970=EDGE_LOOP('',(#7762,#7763,#7764,#7765));
#2971=EDGE_LOOP('',(#7766,#7767,#7768));
#2972=EDGE_LOOP('',(#7769,#7770,#7771,#7772));
#2973=EDGE_LOOP('',(#7773,#7774,#7775,#7776));
#2974=EDGE_LOOP('',(#7777,#7778,#7779,#7780));
#2975=EDGE_LOOP('',(#7781,#7782,#7783,#7784));
#2976=EDGE_LOOP('',(#7785,#7786,#7787,#7788));
#2977=EDGE_LOOP('',(#7789,#7790,#7791,#7792,#7793));
#2978=EDGE_LOOP('',(#7794,#7795,#7796,#7797,#7798));
#2979=EDGE_LOOP('',(#7799,#7800,#7801,#7802));
#2980=EDGE_LOOP('',(#7803,#7804,#7805,#7806));
#2981=EDGE_LOOP('',(#7807,#7808,#7809,#7810));
#2982=EDGE_LOOP('',(#7811,#7812,#7813,#7814));
#2983=EDGE_LOOP('',(#7815,#7816,#7817,#7818));
#2984=EDGE_LOOP('',(#7819,#7820,#7821,#7822));
#2985=EDGE_LOOP('',(#7823,#7824,#7825,#7826));
#2986=EDGE_LOOP('',(#7827,#7828,#7829,#7830));
#2987=EDGE_LOOP('',(#7831,#7832,#7833,#7834));
#2988=EDGE_LOOP('',(#7835,#7836,#7837,#7838));
#2989=EDGE_LOOP('',(#7839,#7840,#7841,#7842));
#2990=EDGE_LOOP('',(#7843,#7844,#7845,#7846));
#2991=EDGE_LOOP('',(#7847,#7848,#7849,#7850));
#2992=EDGE_LOOP('',(#7851,#7852,#7853,#7854));
#2993=EDGE_LOOP('',(#7855,#7856,#7857,#7858));
#2994=EDGE_LOOP('',(#7859,#7860,#7861,#7862,#7863,#7864,#7865));
#2995=EDGE_LOOP('',(#7866,#7867,#7868,#7869,#7870,#7871,#7872,#7873,#7874,
#7875));
#2996=EDGE_LOOP('',(#7876));
#2997=EDGE_LOOP('',(#7877));
#2998=EDGE_LOOP('',(#7878,#7879,#7880,#7881,#7882,#7883,#7884,#7885,#7886,
#7887));
#2999=EDGE_LOOP('',(#7888));
#3000=EDGE_LOOP('',(#7889));
#3001=EDGE_LOOP('',(#7890,#7891,#7892,#7893));
#3002=EDGE_LOOP('',(#7894,#7895,#7896,#7897));
#3003=EDGE_LOOP('',(#7898,#7899,#7900,#7901));
#3004=EDGE_LOOP('',(#7902,#7903,#7904,#7905));
#3005=EDGE_LOOP('',(#7906,#7907,#7908,#7909,#7910,#7911,#7912));
#3006=EDGE_LOOP('',(#7913,#7914,#7915,#7916));
#3007=EDGE_LOOP('',(#7917,#7918,#7919,#7920));
#3008=EDGE_LOOP('',(#7921));
#3009=EDGE_LOOP('',(#7922,#7923,#7924,#7925));
#3010=EDGE_LOOP('',(#7926));
#3011=EDGE_LOOP('',(#7927,#7928,#7929,#7930));
#3012=EDGE_LOOP('',(#7931,#7932,#7933,#7934,#7935,#7936));
#3013=EDGE_LOOP('',(#7937,#7938,#7939,#7940,#7941,#7942,#7943,#7944,#7945,
#7946));
#3014=EDGE_LOOP('',(#7947));
#3015=EDGE_LOOP('',(#7948));
#3016=EDGE_LOOP('',(#7949,#7950,#7951,#7952,#7953,#7954,#7955,#7956,#7957,
#7958));
#3017=EDGE_LOOP('',(#7959));
#3018=EDGE_LOOP('',(#7960));
#3019=EDGE_LOOP('',(#7961,#7962,#7963,#7964,#7965,#7966,#7967,#7968));
#3020=EDGE_LOOP('',(#7969,#7970,#7971,#7972));
#3021=EDGE_LOOP('',(#7973,#7974,#7975,#7976));
#3022=EDGE_LOOP('',(#7977,#7978,#7979,#7980));
#3023=EDGE_LOOP('',(#7981,#7982,#7983,#7984,#7985));
#3024=EDGE_LOOP('',(#7986,#7987,#7988,#7989,#7990));
#3025=EDGE_LOOP('',(#7991,#7992,#7993,#7994));
#3026=EDGE_LOOP('',(#7995,#7996,#7997,#7998));
#3027=EDGE_LOOP('',(#7999,#8000,#8001,#8002));
#3028=EDGE_LOOP('',(#8003,#8004,#8005,#8006,#8007));
#3029=EDGE_LOOP('',(#8008,#8009,#8010,#8011));
#3030=EDGE_LOOP('',(#8012,#8013,#8014,#8015,#8016));
#3031=EDGE_LOOP('',(#8017,#8018,#8019,#8020));
#3032=EDGE_LOOP('',(#8021,#8022,#8023,#8024));
#3033=EDGE_LOOP('',(#8025,#8026,#8027,#8028,#8029,#8030,#8031));
#3034=EDGE_LOOP('',(#8032,#8033,#8034,#8035,#8036));
#3035=EDGE_LOOP('',(#8037,#8038,#8039,#8040));
#3036=EDGE_LOOP('',(#8041,#8042,#8043,#8044,#8045,#8046,#8047));
#3037=EDGE_LOOP('',(#8048,#8049,#8050,#8051,#8052,#8053,#8054));
#3038=EDGE_LOOP('',(#8055,#8056,#8057,#8058,#8059));
#3039=EDGE_LOOP('',(#8060,#8061,#8062,#8063));
#3040=EDGE_LOOP('',(#8064,#8065,#8066,#8067,#8068,#8069,#8070));
#3041=EDGE_LOOP('',(#8071,#8072,#8073,#8074,#8075,#8076,#8077,#8078,#8079,
#8080,#8081,#8082));
#3042=EDGE_LOOP('',(#8083,#8084,#8085,#8086,#8087,#8088,#8089,#8090));
#3043=EDGE_LOOP('',(#8091,#8092,#8093,#8094));
#3044=EDGE_LOOP('',(#8095));
#3045=EDGE_LOOP('',(#8096,#8097,#8098,#8099));
#3046=EDGE_LOOP('',(#8100));
#3047=EDGE_LOOP('',(#8101,#8102,#8103));
#3048=EDGE_LOOP('',(#8104,#8105,#8106));
#3049=EDGE_LOOP('',(#8107,#8108,#8109,#8110));
#3050=EDGE_LOOP('',(#8111));
#3051=EDGE_LOOP('',(#8112));
#3052=EDGE_LOOP('',(#8113));
#3053=EDGE_LOOP('',(#8114));
#3054=EDGE_LOOP('',(#8115));
#3055=EDGE_LOOP('',(#8116,#8117,#8118,#8119));
#3056=EDGE_LOOP('',(#8120));
#3057=EDGE_LOOP('',(#8121));
#3058=EDGE_LOOP('',(#8122));
#3059=EDGE_LOOP('',(#8123));
#3060=EDGE_LOOP('',(#8124));
#3061=EDGE_LOOP('',(#8125,#8126,#8127,#8128,#8129,#8130));
#3062=EDGE_LOOP('',(#8131,#8132,#8133,#8134,#8135,#8136,#8137,#8138,#8139,
#8140));
#3063=EDGE_LOOP('',(#8141,#8142,#8143,#8144,#8145,#8146));
#3064=EDGE_LOOP('',(#8147,#8148,#8149,#8150));
#3065=EDGE_LOOP('',(#8151,#8152,#8153,#8154,#8155));
#3066=EDGE_LOOP('',(#8156,#8157,#8158,#8159,#8160));
#3067=EDGE_LOOP('',(#8161,#8162,#8163,#8164,#8165,#8166));
#3068=EDGE_LOOP('',(#8167));
#3069=EDGE_LOOP('',(#8168,#8169,#8170,#8171,#8172,#8173));
#3070=EDGE_LOOP('',(#8174));
#3071=EDGE_LOOP('',(#8175,#8176,#8177,#8178));
#3072=EDGE_LOOP('',(#8179,#8180,#8181,#8182,#8183));
#3073=EDGE_LOOP('',(#8184,#8185,#8186,#8187,#8188));
#3074=EDGE_LOOP('',(#8189,#8190,#8191,#8192,#8193,#8194));
#3075=EDGE_LOOP('',(#8195,#8196,#8197,#8198,#8199,#8200));
#3076=EDGE_LOOP('',(#8201,#8202,#8203,#8204,#8205,#8206,#8207,#8208));
#3077=EDGE_LOOP('',(#8209,#8210,#8211,#8212,#8213));
#3078=EDGE_LOOP('',(#8214,#8215,#8216,#8217,#8218));
#3079=EDGE_LOOP('',(#8219,#8220,#8221,#8222));
#3080=EDGE_LOOP('',(#8223,#8224,#8225,#8226));
#3081=EDGE_LOOP('',(#8227,#8228,#8229,#8230,#8231,#8232,#8233,#8234,#8235,
#8236));
#3082=EDGE_LOOP('',(#8237,#8238,#8239,#8240,#8241));
#3083=EDGE_LOOP('',(#8242,#8243,#8244,#8245));
#3084=EDGE_LOOP('',(#8246,#8247,#8248,#8249));
#3085=EDGE_LOOP('',(#8250,#8251,#8252,#8253,#8254));
#3086=EDGE_LOOP('',(#8255,#8256,#8257,#8258));
#3087=EDGE_LOOP('',(#8259,#8260,#8261,#8262));
#3088=EDGE_LOOP('',(#8263,#8264,#8265,#8266));
#3089=EDGE_LOOP('',(#8267,#8268,#8269,#8270));
#3090=EDGE_LOOP('',(#8271,#8272,#8273,#8274));
#3091=EDGE_LOOP('',(#8275,#8276,#8277,#8278));
#3092=EDGE_LOOP('',(#8279,#8280,#8281,#8282));
#3093=EDGE_LOOP('',(#8283,#8284,#8285,#8286));
#3094=EDGE_LOOP('',(#8287,#8288,#8289,#8290));
#3095=EDGE_LOOP('',(#8291,#8292,#8293,#8294));
#3096=EDGE_LOOP('',(#8295,#8296,#8297,#8298));
#3097=EDGE_LOOP('',(#8299,#8300,#8301,#8302,#8303,#8304,#8305,#8306));
#3098=EDGE_LOOP('',(#8307));
#3099=EDGE_LOOP('',(#8308));
#3100=EDGE_LOOP('',(#8309,#8310,#8311,#8312,#8313,#8314,#8315,#8316));
#3101=EDGE_LOOP('',(#8317));
#3102=EDGE_LOOP('',(#8318));
#3103=EDGE_LOOP('',(#8319,#8320,#8321,#8322));
#3104=EDGE_LOOP('',(#8323,#8324,#8325,#8326));
#3105=EDGE_LOOP('',(#8327,#8328,#8329,#8330));
#3106=EDGE_LOOP('',(#8331,#8332,#8333,#8334));
#3107=EDGE_LOOP('',(#8335,#8336,#8337,#8338));
#3108=EDGE_LOOP('',(#8339,#8340,#8341,#8342));
#3109=EDGE_LOOP('',(#8343,#8344,#8345,#8346));
#3110=EDGE_LOOP('',(#8347,#8348,#8349,#8350));
#3111=EDGE_LOOP('',(#8351,#8352,#8353,#8354));
#3112=EDGE_LOOP('',(#8355,#8356,#8357,#8358));
#3113=EDGE_LOOP('',(#8359,#8360,#8361,#8362));
#3114=EDGE_LOOP('',(#8363,#8364,#8365,#8366));
#3115=EDGE_LOOP('',(#8367,#8368,#8369,#8370));
#3116=EDGE_LOOP('',(#8371,#8372,#8373,#8374));
#3117=EDGE_LOOP('',(#8375,#8376,#8377,#8378));
#3118=EDGE_LOOP('',(#8379,#8380,#8381,#8382));
#3119=EDGE_LOOP('',(#8383,#8384,#8385,#8386));
#3120=EDGE_LOOP('',(#8387,#8388,#8389,#8390));
#3121=EDGE_LOOP('',(#8391,#8392,#8393,#8394));
#3122=EDGE_LOOP('',(#8395,#8396,#8397,#8398));
#3123=EDGE_LOOP('',(#8399,#8400,#8401,#8402));
#3124=CIRCLE('',#9073,3.30718913883074);
#3125=CIRCLE('',#9075,2.);
#3126=CIRCLE('',#9076,2.);
#3127=CIRCLE('',#9078,3.30718913883074);
#3128=CIRCLE('',#9083,0.400000000000007);
#3129=CIRCLE('',#9084,0.400000000000007);
#3130=CIRCLE('',#9085,1.6);
#3131=CIRCLE('',#9086,0.400000000000014);
#3132=CIRCLE('',#9087,0.400000000000014);
#3133=CIRCLE('',#9089,0.400000000000011);
#3134=CIRCLE('',#9090,1.6);
#3135=CIRCLE('',#9091,0.399999999999994);
#3136=CIRCLE('',#9092,0.399999999999994);
#3137=CIRCLE('',#9094,1.39999999999999);
#3138=CIRCLE('',#9095,0.399999999999997);
#3139=CIRCLE('',#9097,0.400000000000009);
#3140=CIRCLE('',#9098,1.4);
#3141=CIRCLE('',#9100,0.400000000000014);
#3142=CIRCLE('',#9101,0.400000000000014);
#3143=CIRCLE('',#9102,0.400000000000014);
#3144=CIRCLE('',#9103,0.400000000000013);
#3145=CIRCLE('',#9104,0.399999999999995);
#3146=CIRCLE('',#9105,0.400000000000011);
#3147=CIRCLE('',#9107,0.400000000000011);
#3148=CIRCLE('',#9108,0.400000000000013);
#3149=CIRCLE('',#9109,0.399999999999995);
#3150=CIRCLE('',#9114,3.30718913883074);
#3151=CIRCLE('',#9116,2.);
#3152=CIRCLE('',#9117,2.);
#3153=CIRCLE('',#9119,3.30718913883074);
#3154=CIRCLE('',#9124,5.);
#3155=CIRCLE('',#9125,5.);
#3156=CIRCLE('',#9126,5.);
#3157=CIRCLE('',#9127,5.);
#3158=CIRCLE('',#9129,39.);
#3159=CIRCLE('',#9130,0.500000000000002);
#3160=CIRCLE('',#9131,39.5);
#3161=CIRCLE('',#9133,39.5);
#3162=CIRCLE('',#9134,0.499999999999999);
#3163=CIRCLE('',#9135,39.);
#3164=CIRCLE('',#9137,5.72168783648703);
#3165=CIRCLE('',#9138,6.15470053837925);
#3166=CIRCLE('',#9139,0.500126081010092);
#3167=CIRCLE('',#9141,6.15470053837925);
#3168=CIRCLE('',#9142,5.72168783648703);
#3169=CIRCLE('',#9143,0.500126081010098);
#3170=CIRCLE('',#9145,5.);
#3171=CIRCLE('',#9147,5.);
#3172=CIRCLE('',#9149,2.);
#3173=CIRCLE('',#9150,2.);
#3174=CIRCLE('',#9152,2.);
#3175=CIRCLE('',#9153,2.);
#3176=CIRCLE('',#9155,15.);
#3177=CIRCLE('',#9156,15.);
#3178=CIRCLE('',#9158,15.);
#3179=CIRCLE('',#9159,15.);
#3180=CIRCLE('',#9161,4.);
#3181=CIRCLE('',#9162,4.);
#3182=CIRCLE('',#9165,4.);
#3183=CIRCLE('',#9181,15.5);
#3184=CIRCLE('',#9182,14.5);
#3185=CIRCLE('',#9192,3.);
#3186=CIRCLE('',#9195,4.5);
#3187=CIRCLE('',#9196,9.5);
#3188=CIRCLE('',#9197,12.2);
#3189=CIRCLE('',#9199,0.5);
#3190=CIRCLE('',#9200,0.5);
#3191=CIRCLE('',#9204,0.5);
#3192=CIRCLE('',#9205,4.);
#3193=CIRCLE('',#9206,4.);
#3194=CIRCLE('',#9207,0.5);
#3195=CIRCLE('',#9208,0.5);
#3196=CIRCLE('',#9209,1.49999774798038);
#3197=CIRCLE('',#9210,1.5);
#3198=CIRCLE('',#9212,15.);
#3199=CIRCLE('',#9213,15.);
#3200=CIRCLE('',#9217,14.5);
#3201=CIRCLE('',#9218,15.5);
#3202=CIRCLE('',#9220,15.5);
#3203=CIRCLE('',#9221,14.5);
#3204=CIRCLE('',#9223,15.);
#3205=CIRCLE('',#9224,15.);
#3206=CIRCLE('',#9239,12.2);
#3207=CIRCLE('',#9240,9.5);
#3208=CIRCLE('',#9241,4.5);
#3209=CIRCLE('',#9246,11.7);
#3210=CIRCLE('',#9247,11.7);
#3211=CIRCLE('',#9248,11.7);
#3212=CIRCLE('',#9249,11.7);
#3213=CIRCLE('',#9251,10.);
#3214=CIRCLE('',#9255,10.);
#3215=CIRCLE('',#9257,10.721687836487);
#3216=CIRCLE('',#9259,10.721687836487);
#3217=CIRCLE('',#9280,0.499999999999998);
#3218=CIRCLE('',#9285,0.499999999999999);
#3219=CIRCLE('',#9287,0.500000000000002);
#3220=CIRCLE('',#9288,0.500000000000001);
#3221=CIRCLE('',#9289,0.500000000000002);
#3222=CIRCLE('',#9290,0.500000000000003);
#3223=CIRCLE('',#9293,4.);
#3224=CIRCLE('',#9297,0.5);
#3225=CIRCLE('',#9299,0.500000000000003);
#3226=CIRCLE('',#9301,0.500000000000003);
#3227=CIRCLE('',#9304,0.5);
#3228=CIRCLE('',#9306,0.500000000000003);
#3229=CIRCLE('',#9308,0.500000000000003);
#3230=CIRCLE('',#9310,0.5);
#3231=CIRCLE('',#9312,0.5);
#3232=CIRCLE('',#9313,0.500000000000001);
#3233=CIRCLE('',#9315,0.500000000000001);
#3234=CIRCLE('',#9316,0.5);
#3235=CIRCLE('',#9318,0.5);
#3236=CIRCLE('',#9320,0.500000000000003);
#3237=CIRCLE('',#9322,0.500000000000003);
#3238=CIRCLE('',#9324,0.5);
#3239=CIRCLE('',#9326,4.0000000000001);
#3240=CIRCLE('',#9329,10.);
#3241=CIRCLE('',#9330,10.);
#3242=CIRCLE('',#9331,0.500000000000003);
#3243=CIRCLE('',#9332,0.499999999999998);
#3244=CIRCLE('',#9334,0.500000000000002);
#3245=CIRCLE('',#9336,0.499999999999998);
#3246=CIRCLE('',#9339,0.499999999999998);
#3247=CIRCLE('',#9341,0.499999999999999);
#3248=CIRCLE('',#9343,0.499999999999998);
#3249=CIRCLE('',#9344,0.500000000000003);
#3250=CIRCLE('',#9347,2.99999999999999);
#3251=CIRCLE('',#9349,2.99999999999999);
#3252=CIRCLE('',#9389,2.99999999999998);
#3253=CIRCLE('',#9391,2.99999999999999);
#3254=CIRCLE('',#9392,2.24999999999998);
#3255=CIRCLE('',#9393,2.99999999999998);
#3256=CIRCLE('',#9405,6.);
#3257=CIRCLE('',#9406,1.);
#3258=CIRCLE('',#9407,6.99999999999999);
#3259=CIRCLE('',#9408,6.99999999999999);
#3260=CIRCLE('',#9409,7.);
#3261=CIRCLE('',#9410,6.99999999999999);
#3262=CIRCLE('',#9411,7.00000000000001);
#3263=CIRCLE('',#9412,6.99999999999999);
#3264=CIRCLE('',#9413,6.99999999999999);
#3265=CIRCLE('',#9414,6.99999999999999);
#3266=CIRCLE('',#9415,7.);
#3267=CIRCLE('',#9416,7.);
#3268=CIRCLE('',#9417,6.99999999999999);
#3269=CIRCLE('',#9418,6.99999999999999);
#3270=CIRCLE('',#9419,7.00000000000002);
#3271=CIRCLE('',#9420,7.);
#3272=CIRCLE('',#9421,7.00000000000001);
#3273=CIRCLE('',#9422,7.);
#3274=CIRCLE('',#9423,6.99999999999999);
#3275=CIRCLE('',#9424,7.00000000000001);
#3276=CIRCLE('',#9425,7.00000000000001);
#3277=CIRCLE('',#9426,6.99999999999999);
#3278=CIRCLE('',#9427,7.00000000000001);
#3279=CIRCLE('',#9428,7.00000000000001);
#3280=CIRCLE('',#9429,7.00000000000001);
#3281=CIRCLE('',#9430,6.99999999999999);
#3282=CIRCLE('',#9431,7.00000000000001);
#3283=CIRCLE('',#9432,6.99999999999999);
#3284=CIRCLE('',#9433,6.99999999999999);
#3285=CIRCLE('',#9435,6.);
#3286=CIRCLE('',#9436,1.);
#3287=CIRCLE('',#9437,7.);
#3288=CIRCLE('',#9438,7.);
#3289=CIRCLE('',#9439,7.);
#3290=CIRCLE('',#9440,7.);
#3291=CIRCLE('',#9441,7.);
#3292=CIRCLE('',#9442,7.);
#3293=CIRCLE('',#9443,7.);
#3294=CIRCLE('',#9444,7.);
#3295=CIRCLE('',#9445,7.00000000000001);
#3296=CIRCLE('',#9446,7.00000000000001);
#3297=CIRCLE('',#9447,7.00000000000001);
#3298=CIRCLE('',#9448,7.);
#3299=CIRCLE('',#9449,6.99999999999999);
#3300=CIRCLE('',#9450,7.);
#3301=CIRCLE('',#9451,7.);
#3302=CIRCLE('',#9452,7.00000000000001);
#3303=CIRCLE('',#9453,7.);
#3304=CIRCLE('',#9454,7.00000000000001);
#3305=CIRCLE('',#9455,7.);
#3306=CIRCLE('',#9456,6.99999999999999);
#3307=CIRCLE('',#9457,6.99999999999999);
#3308=CIRCLE('',#9458,6.99999999999999);
#3309=CIRCLE('',#9459,7.00000000000001);
#3310=CIRCLE('',#9460,7.);
#3311=CIRCLE('',#9461,6.99999999999999);
#3312=CIRCLE('',#9462,7.);
#3313=CIRCLE('',#9463,7.);
#3314=CIRCLE('',#9517,5.9);
#3315=CIRCLE('',#9518,0.500000000000001);
#3316=CIRCLE('',#9519,6.4);
#3317=CIRCLE('',#9520,0.500000000000001);
#3318=CIRCLE('',#9522,6.4);
#3319=CIRCLE('',#9523,0.500000000000001);
#3320=CIRCLE('',#9524,5.9);
#3321=CIRCLE('',#9525,0.500000000000001);
#3322=CIRCLE('',#9527,1.5);
#3323=CIRCLE('',#9528,1.5);
#3324=CIRCLE('',#9530,2.00000000000001);
#3325=CIRCLE('',#9531,2.00000000000001);
#3326=CIRCLE('',#9533,2.);
#3327=CIRCLE('',#9534,2.);
#3328=CIRCLE('',#9536,14.1232719083235);
#3329=CIRCLE('',#9537,1.);
#3330=CIRCLE('',#9538,14.989297312108);
#3331=CIRCLE('',#9540,14.989297312108);
#3332=CIRCLE('',#9541,1.);
#3333=CIRCLE('',#9542,14.1232719083235);
#3334=CIRCLE('',#9544,100.);
#3335=CIRCLE('',#9545,100.);
#3336=CIRCLE('',#9548,100.);
#3337=CIRCLE('',#9549,100.);
#3338=CIRCLE('',#9551,100.);
#3339=CIRCLE('',#9552,390.917804157437);
#3340=CIRCLE('',#9553,100.);
#3341=CIRCLE('',#9554,100.);
#3342=CIRCLE('',#9555,390.917804135939);
#3343=CIRCLE('',#9556,100.);
#3344=CIRCLE('',#9558,100.);
#3345=CIRCLE('',#9559,100.);
#3346=CIRCLE('',#9561,3.);
#3347=CIRCLE('',#9562,3.);
#3348=CIRCLE('',#9564,12.5);
#3349=CIRCLE('',#9565,100.5);
#3350=CIRCLE('',#9566,6.44337567297407);
#3351=CIRCLE('',#9567,106.443375672974);
#3352=CIRCLE('',#9568,27.5);
#3353=CIRCLE('',#9569,35.5);
#3354=CIRCLE('',#9570,3.5);
#3355=CIRCLE('',#9571,15.5);
#3356=CIRCLE('',#9572,6.50000000000001);
#3357=CIRCLE('',#9574,12.5);
#3358=CIRCLE('',#9575,6.50000000000001);
#3359=CIRCLE('',#9576,15.5);
#3360=CIRCLE('',#9577,3.5);
#3361=CIRCLE('',#9578,35.5);
#3362=CIRCLE('',#9579,27.5);
#3363=CIRCLE('',#9580,106.443375672974);
#3364=CIRCLE('',#9581,6.44337567297407);
#3365=CIRCLE('',#9582,100.5);
#3366=CIRCLE('',#9585,16.);
#3367=CIRCLE('',#9586,16.);
#3368=CIRCLE('',#9587,16.);
#3369=CIRCLE('',#9588,16.);
#3370=CIRCLE('',#9590,7.);
#3371=CIRCLE('',#9591,7.);
#3372=CIRCLE('',#9593,12.);
#3373=CIRCLE('',#9594,12.);
#3374=CIRCLE('',#9598,28.);
#3375=CIRCLE('',#9599,28.);
#3376=CIRCLE('',#9602,35.);
#3377=CIRCLE('',#9603,35.);
#3378=CIRCLE('',#9605,5.);
#3379=CIRCLE('',#9606,105.);
#3380=CIRCLE('',#9607,13.5459216391339);
#3381=CIRCLE('',#9609,105.57735026919);
#3382=CIRCLE('',#9613,601.835963345588);
#3383=CIRCLE('',#9614,5.57735026918963);
#3384=CIRCLE('',#9616,5.57735026918963);
#3385=CIRCLE('',#9617,601.835963357857);
#3386=CIRCLE('',#9618,5.);
#3387=CIRCLE('',#9621,13.5459216391339);
#3388=CIRCLE('',#9623,105.57735026919);
#3389=CIRCLE('',#9624,105.);
#3390=CIRCLE('',#9627,0.999999999999998);
#3391=CIRCLE('',#9630,0.999999999999998);
#3392=CIRCLE('',#9633,3.);
#3393=CIRCLE('',#9634,3.);
#3394=CIRCLE('',#9637,3.7);
#3395=CIRCLE('',#9639,3.7);
#3396=CIRCLE('',#9661,0.5);
#3397=CIRCLE('',#9662,0.500000000000001);
#3398=CIRCLE('',#9664,0.500000000000001);
#3399=CIRCLE('',#9667,0.500000000000003);
#3400=CIRCLE('',#9669,0.499999999999998);
#3401=CIRCLE('',#9670,0.500000000000005);
#3402=CIRCLE('',#9672,0.5);
#3403=CIRCLE('',#9673,0.500000000000001);
#3404=CIRCLE('',#9675,0.500000000000001);
#3405=CIRCLE('',#9678,0.500000000000003);
#3406=CIRCLE('',#9680,0.499999999999998);
#3407=CIRCLE('',#9681,0.499999999999992);
#3408=CIRCLE('',#9682,0.500000000000009);
#3409=CIRCLE('',#9683,0.499999999999998);
#3410=CIRCLE('',#9685,0.499999999999998);
#3411=CIRCLE('',#9687,0.5);
#3412=CIRCLE('',#9689,0.5);
#3413=CIRCLE('',#9691,0.499999999999999);
#3414=CIRCLE('',#9693,0.499999999999999);
#3415=CIRCLE('',#9695,0.5);
#3416=CIRCLE('',#9697,0.5);
#3417=CIRCLE('',#9699,0.499999999999998);
#3418=CIRCLE('',#9701,0.499999999999998);
#3419=CIRCLE('',#9702,0.500000000000009);
#3420=CIRCLE('',#9705,75.);
#3421=CIRCLE('',#9706,76.5);
#3422=CIRCLE('',#9708,76.5);
#3423=CIRCLE('',#9709,75.);
#3424=CIRCLE('',#9711,219.);
#3425=CIRCLE('',#9712,222.);
#3426=CIRCLE('',#9714,222.);
#3427=CIRCLE('',#9715,219.);
#3428=CIRCLE('',#9717,220.3);
#3429=CIRCLE('',#9718,220.3);
#3430=CIRCLE('',#9720,2.);
#3431=CIRCLE('',#9721,2.);
#3432=CIRCLE('',#9723,2.);
#3433=CIRCLE('',#9724,2.);
#3434=CIRCLE('',#9726,1.00000000000001);
#3435=CIRCLE('',#9727,1.00000000000001);
#3436=CIRCLE('',#9729,75.);
#3437=CIRCLE('',#9731,2.);
#3438=CIRCLE('',#9732,2.);
#3439=CIRCLE('',#9734,2.);
#3440=CIRCLE('',#9735,2.);
#3441=CIRCLE('',#9737,1.00000000000001);
#3442=CIRCLE('',#9738,1.00000000000001);
#3443=CIRCLE('',#9740,75.);
#3444=CIRCLE('',#9748,2.06253449527014);
#3445=CIRCLE('',#9749,103.);
#3446=CIRCLE('',#9751,2.06253449527014);
#3447=CIRCLE('',#9752,103.);
#3448=CIRCLE('',#9755,100.);
#3449=CIRCLE('',#9756,100.);
#3450=CIRCLE('',#9765,4.43478616545489);
#3451=CIRCLE('',#9767,4.43478616545489);
#3452=CIRCLE('',#9775,2.06253449527014);
#3453=CIRCLE('',#9776,101.7);
#3454=CIRCLE('',#9778,2.06253449527014);
#3455=CIRCLE('',#9779,101.7);
#3456=CIRCLE('',#9795,1.5);
#3457=CIRCLE('',#9798,5.93478616545488);
#3458=CIRCLE('',#9799,1.5);
#3459=CIRCLE('',#9802,1.5);
#3460=CIRCLE('',#9805,1.5);
#3461=CIRCLE('',#9806,5.93478616545488);
#3462=CIRCLE('',#9814,1.20000000000001);
#3463=CIRCLE('',#9815,1.19999999999999);
#3464=CIRCLE('',#9817,1.20000000000001);
#3465=CIRCLE('',#9818,1.19999999999999);
#3466=CIRCLE('',#9820,1.);
#3467=CIRCLE('',#9821,1.);
#3468=CIRCLE('',#9826,3.30718913883074);
#3469=CIRCLE('',#9828,2.);
#3470=CIRCLE('',#9829,2.);
#3471=CIRCLE('',#9831,3.30718913883074);
#3472=CIRCLE('',#9836,0.999999999999998);
#3473=CIRCLE('',#9837,1.);
#3474=CIRCLE('',#9838,0.999999999999998);
#3475=CIRCLE('',#9839,1.);
#3476=CIRCLE('',#9841,0.6);
#3477=CIRCLE('',#9842,0.6);
#3478=CIRCLE('',#9844,1.);
#3479=CIRCLE('',#9845,0.999999999999998);
#3480=CIRCLE('',#9846,1.);
#3481=CIRCLE('',#9847,0.999999999999998);
#3482=CIRCLE('',#9850,33.6360679582853);
#3483=CIRCLE('',#9851,33.6360679582853);
#3484=CIRCLE('',#9853,0.999999999999998);
#3485=CIRCLE('',#9854,33.6360679582853);
#3486=CIRCLE('',#9856,0.999999999999998);
#3487=CIRCLE('',#9858,33.6360679582853);
#3488=CIRCLE('',#9867,0.999999999999997);
#3489=CIRCLE('',#9868,0.999999999999999);
#3490=CIRCLE('',#9869,1.);
#3491=CIRCLE('',#9870,1.);
#3492=CIRCLE('',#9873,2.);
#3493=CIRCLE('',#9874,0.25);
#3494=CIRCLE('',#9875,2.25);
#3495=CIRCLE('',#9877,4.4);
#3496=CIRCLE('',#9878,0.25);
#3497=CIRCLE('',#9879,4.15);
#3498=CIRCLE('',#9880,0.25);
#3499=CIRCLE('',#9882,1.99999999999999);
#3500=CIRCLE('',#9883,0.25);
#3501=CIRCLE('',#9884,2.24999999999999);
#3502=CIRCLE('',#9886,4.15);
#3503=CIRCLE('',#9887,0.25);
#3504=CIRCLE('',#9888,4.4);
#3505=CIRCLE('',#9889,0.25);
#3506=CIRCLE('',#9891,2.25);
#3507=CIRCLE('',#9892,0.25);
#3508=CIRCLE('',#9893,2.);
#3509=CIRCLE('',#9895,2.25);
#3510=CIRCLE('',#9896,0.25);
#3511=CIRCLE('',#9897,2.00000000000001);
#3512=CIRCLE('',#9902,9.75);
#3513=CIRCLE('',#9903,24.25);
#3514=CIRCLE('',#9904,20.25);
#3515=CIRCLE('',#9905,4.15);
#3516=CIRCLE('',#9907,20.25);
#3517=CIRCLE('',#9908,24.25);
#3518=CIRCLE('',#9909,9.74999999999999);
#3519=CIRCLE('',#9910,4.15);
#3520=CIRCLE('',#9913,20.);
#3521=CIRCLE('',#9914,20.);
#3522=CIRCLE('',#9917,4.4);
#3523=CIRCLE('',#9918,4.4);
#3524=CIRCLE('',#9921,9.99999999999999);
#3525=CIRCLE('',#9922,9.99999999999999);
#3526=CIRCLE('',#9924,24.);
#3527=CIRCLE('',#9925,24.);
#3528=CIRCLE('',#9927,0.25);
#3529=CIRCLE('',#9933,0.249999999999998);
#3530=CIRCLE('',#9937,0.249999999999998);
#3531=CIRCLE('',#9939,0.25);
#3532=VERTEX_POINT('',#12218);
#3533=VERTEX_POINT('',#12221);
#3534=VERTEX_POINT('',#12223);
#3535=VERTEX_POINT('',#12227);
#3536=VERTEX_POINT('',#12233);
#3537=VERTEX_POINT('',#12234);
#3538=VERTEX_POINT('',#12237);
#3539=VERTEX_POINT('',#12239);
#3540=VERTEX_POINT('',#12243);
#3541=VERTEX_POINT('',#12245);
#3542=VERTEX_POINT('',#12247);
#3543=VERTEX_POINT('',#12251);
#3544=VERTEX_POINT('',#12255);
#3545=VERTEX_POINT('',#12259);
#3546=VERTEX_POINT('',#12261);
#3547=VERTEX_POINT('',#12263);
#3548=VERTEX_POINT('',#12434);
#3549=VERTEX_POINT('',#12435);
#3550=VERTEX_POINT('',#13661);
#3551=VERTEX_POINT('',#13662);
#3552=VERTEX_POINT('',#14140);
#3553=VERTEX_POINT('',#14141);
#3554=VERTEX_POINT('',#15676);
#3555=VERTEX_POINT('',#15679);
#3556=VERTEX_POINT('',#15681);
#3557=VERTEX_POINT('',#15685);
#3558=VERTEX_POINT('',#15691);
#3559=VERTEX_POINT('',#15692);
#3560=VERTEX_POINT('',#15694);
#3561=VERTEX_POINT('',#15696);
#3562=VERTEX_POINT('',#15698);
#3563=VERTEX_POINT('',#15700);
#3564=VERTEX_POINT('',#15702);
#3565=VERTEX_POINT('',#15704);
#3566=VERTEX_POINT('',#15706);
#3567=VERTEX_POINT('',#15721);
#3568=VERTEX_POINT('',#15722);
#3569=VERTEX_POINT('',#15724);
#3570=VERTEX_POINT('',#15726);
#3571=VERTEX_POINT('',#15739);
#3572=VERTEX_POINT('',#15740);
#3573=VERTEX_POINT('',#15742);
#3574=VERTEX_POINT('',#15744);
#3575=VERTEX_POINT('',#15757);
#3576=VERTEX_POINT('',#15758);
#3577=VERTEX_POINT('',#15760);
#3578=VERTEX_POINT('',#15792);
#3579=VERTEX_POINT('',#15796);
#3580=VERTEX_POINT('',#15797);
#3581=VERTEX_POINT('',#15799);
#3582=VERTEX_POINT('',#15831);
#3583=VERTEX_POINT('',#15835);
#3584=VERTEX_POINT('',#15836);
#3585=VERTEX_POINT('',#15847);
#3586=VERTEX_POINT('',#15848);
#3587=VERTEX_POINT('',#15859);
#3588=VERTEX_POINT('',#15861);
#3589=VERTEX_POINT('',#15865);
#3590=VERTEX_POINT('',#15867);
#3591=VERTEX_POINT('',#15871);
#3592=VERTEX_POINT('',#15873);
#3593=VERTEX_POINT('',#15882);
#3594=VERTEX_POINT('',#15884);
#3595=VERTEX_POINT('',#15888);
#3596=VERTEX_POINT('',#15889);
#3597=VERTEX_POINT('',#15891);
#3598=VERTEX_POINT('',#15903);
#3599=VERTEX_POINT('',#15907);
#3600=VERTEX_POINT('',#15908);
#3601=VERTEX_POINT('',#15921);
#3602=VERTEX_POINT('',#15923);
#3603=VERTEX_POINT('',#15936);
#3604=VERTEX_POINT('',#15938);
#3605=VERTEX_POINT('',#15940);
#3606=VERTEX_POINT('',#15942);
#3607=VERTEX_POINT('',#16082);
#3608=VERTEX_POINT('',#16150);
#3609=VERTEX_POINT('',#16173);
#3610=VERTEX_POINT('',#16175);
#3611=VERTEX_POINT('',#16177);
#3612=VERTEX_POINT('',#16179);
#3613=VERTEX_POINT('',#16212);
#3614=VERTEX_POINT('',#16213);
#3615=VERTEX_POINT('',#16244);
#3616=VERTEX_POINT('',#16246);
#3617=VERTEX_POINT('',#16279);
#3618=VERTEX_POINT('',#16280);
#3619=VERTEX_POINT('',#16311);
#3620=VERTEX_POINT('',#16313);
#3621=VERTEX_POINT('',#16332);
#3622=VERTEX_POINT('',#16336);
#3623=VERTEX_POINT('',#16337);
#3624=VERTEX_POINT('',#16348);
#3625=VERTEX_POINT('',#16350);
#3626=VERTEX_POINT('',#16363);
#3627=VERTEX_POINT('',#16364);
#3628=VERTEX_POINT('',#16375);
#3629=VERTEX_POINT('',#16377);
#3630=VERTEX_POINT('',#16390);
#3631=VERTEX_POINT('',#16391);
#3632=VERTEX_POINT('',#16402);
#3633=VERTEX_POINT('',#16404);
#3634=VERTEX_POINT('',#16417);
#3635=VERTEX_POINT('',#16418);
#3636=VERTEX_POINT('',#16429);
#3637=VERTEX_POINT('',#16431);
#3638=VERTEX_POINT('',#16444);
#3639=VERTEX_POINT('',#16445);
#3640=VERTEX_POINT('',#16456);
#3641=VERTEX_POINT('',#16458);
#3642=VERTEX_POINT('',#16471);
#3643=VERTEX_POINT('',#16472);
#3644=VERTEX_POINT('',#16483);
#3645=VERTEX_POINT('',#16485);
#3646=VERTEX_POINT('',#16498);
#3647=VERTEX_POINT('',#16499);
#3648=VERTEX_POINT('',#16510);
#3649=VERTEX_POINT('',#16512);
#3650=VERTEX_POINT('',#16532);
#3651=VERTEX_POINT('',#16533);
#3652=VERTEX_POINT('',#16571);
#3653=VERTEX_POINT('',#16576);
#3654=VERTEX_POINT('',#16626);
#3655=VERTEX_POINT('',#16627);
#3656=VERTEX_POINT('',#16668);
#3657=VERTEX_POINT('',#16673);
#3658=VERTEX_POINT('',#16723);
#3659=VERTEX_POINT('',#16724);
#3660=VERTEX_POINT('',#16759);
#3661=VERTEX_POINT('',#16764);
#3662=VERTEX_POINT('',#16811);
#3663=VERTEX_POINT('',#16812);
#3664=VERTEX_POINT('',#16850);
#3665=VERTEX_POINT('',#16855);
#3666=VERTEX_POINT('',#16902);
#3667=VERTEX_POINT('',#16903);
#3668=VERTEX_POINT('',#16941);
#3669=VERTEX_POINT('',#16946);
#3670=VERTEX_POINT('',#16993);
#3671=VERTEX_POINT('',#16994);
#3672=VERTEX_POINT('',#17032);
#3673=VERTEX_POINT('',#17037);
#3674=VERTEX_POINT('',#17081);
#3675=VERTEX_POINT('',#17083);
#3676=VERTEX_POINT('',#17085);
#3677=VERTEX_POINT('',#17092);
#3678=VERTEX_POINT('',#17094);
#3679=VERTEX_POINT('',#17101);
#3680=VERTEX_POINT('',#17103);
#3681=VERTEX_POINT('',#17110);
#3682=VERTEX_POINT('',#17112);
#3683=VERTEX_POINT('',#17119);
#3684=VERTEX_POINT('',#17121);
#3685=VERTEX_POINT('',#17128);
#3686=VERTEX_POINT('',#17130);
#3687=VERTEX_POINT('',#17137);
#3688=VERTEX_POINT('',#17139);
#3689=VERTEX_POINT('',#17146);
#3690=VERTEX_POINT('',#17148);
#3691=VERTEX_POINT('',#17155);
#3692=VERTEX_POINT('',#17157);
#3693=VERTEX_POINT('',#17164);
#3694=VERTEX_POINT('',#17166);
#3695=VERTEX_POINT('',#17173);
#3696=VERTEX_POINT('',#17175);
#3697=VERTEX_POINT('',#17182);
#3698=VERTEX_POINT('',#17184);
#3699=VERTEX_POINT('',#17191);
#3700=VERTEX_POINT('',#17193);
#3701=VERTEX_POINT('',#17200);
#3702=VERTEX_POINT('',#17207);
#3703=VERTEX_POINT('',#17209);
#3704=VERTEX_POINT('',#17211);
#3705=VERTEX_POINT('',#17213);
#3706=VERTEX_POINT('',#17216);
#3707=VERTEX_POINT('',#17569);
#3708=VERTEX_POINT('',#17584);
#3709=VERTEX_POINT('',#17614);
#3710=VERTEX_POINT('',#17629);
#3711=VERTEX_POINT('',#17659);
#3712=VERTEX_POINT('',#17676);
#3713=VERTEX_POINT('',#17706);
#3714=VERTEX_POINT('',#17723);
#3715=VERTEX_POINT('',#17755);
#3716=VERTEX_POINT('',#17772);
#3717=VERTEX_POINT('',#17804);
#3718=VERTEX_POINT('',#17823);
#3719=VERTEX_POINT('',#17906);
#3720=VERTEX_POINT('',#17948);
#3721=VERTEX_POINT('',#18046);
#3722=VERTEX_POINT('',#18152);
#3723=VERTEX_POINT('',#18335);
#3724=VERTEX_POINT('',#18337);
#3725=VERTEX_POINT('',#18339);
#3726=VERTEX_POINT('',#18344);
#3727=VERTEX_POINT('',#18345);
#3728=VERTEX_POINT('',#18380);
#3729=VERTEX_POINT('',#18383);
#3730=VERTEX_POINT('',#18385);
#3731=VERTEX_POINT('',#18425);
#3732=VERTEX_POINT('',#18427);
#3733=VERTEX_POINT('',#18431);
#3734=VERTEX_POINT('',#18432);
#3735=VERTEX_POINT('',#18434);
#3736=VERTEX_POINT('',#18436);
#3737=VERTEX_POINT('',#18440);
#3738=VERTEX_POINT('',#18441);
#3739=VERTEX_POINT('',#18454);
#3740=VERTEX_POINT('',#18462);
#3741=VERTEX_POINT('',#18464);
#3742=VERTEX_POINT('',#18466);
#3743=VERTEX_POINT('',#18468);
#3744=VERTEX_POINT('',#18470);
#3745=VERTEX_POINT('',#18472);
#3746=VERTEX_POINT('',#18474);
#3747=VERTEX_POINT('',#18476);
#3748=VERTEX_POINT('',#18479);
#3749=VERTEX_POINT('',#18486);
#3750=VERTEX_POINT('',#18499);
#3751=VERTEX_POINT('',#18501);
#3752=VERTEX_POINT('',#18505);
#3753=VERTEX_POINT('',#18506);
#3754=VERTEX_POINT('',#18508);
#3755=VERTEX_POINT('',#18510);
#3756=VERTEX_POINT('',#18521);
#3757=VERTEX_POINT('',#18548);
#3758=VERTEX_POINT('',#18585);
#3759=VERTEX_POINT('',#18671);
#3760=VERTEX_POINT('',#18673);
#3761=VERTEX_POINT('',#18675);
#3762=VERTEX_POINT('',#18677);
#3763=VERTEX_POINT('',#18681);
#3764=VERTEX_POINT('',#18683);
#3765=VERTEX_POINT('',#18685);
#3766=VERTEX_POINT('',#18687);
#3767=VERTEX_POINT('',#18689);
#3768=VERTEX_POINT('',#19125);
#3769=VERTEX_POINT('',#19126);
#3770=VERTEX_POINT('',#19157);
#3771=VERTEX_POINT('',#19163);
#3772=VERTEX_POINT('',#19171);
#3773=VERTEX_POINT('',#19178);
#3774=VERTEX_POINT('',#19186);
#3775=VERTEX_POINT('',#19193);
#3776=VERTEX_POINT('',#19201);
#3777=VERTEX_POINT('',#19208);
#3778=VERTEX_POINT('',#19216);
#3779=VERTEX_POINT('',#19223);
#3780=VERTEX_POINT('',#19231);
#3781=VERTEX_POINT('',#19238);
#3782=VERTEX_POINT('',#19246);
#3783=VERTEX_POINT('',#19253);
#3784=VERTEX_POINT('',#19261);
#3785=VERTEX_POINT('',#19268);
#3786=VERTEX_POINT('',#19334);
#3787=VERTEX_POINT('',#19336);
#3788=VERTEX_POINT('',#19341);
#3789=VERTEX_POINT('',#19342);
#3790=VERTEX_POINT('',#19344);
#3791=VERTEX_POINT('',#19364);
#3792=VERTEX_POINT('',#19394);
#3793=VERTEX_POINT('',#19399);
#3794=VERTEX_POINT('',#19445);
#3795=VERTEX_POINT('',#19446);
#3796=VERTEX_POINT('',#19454);
#3797=VERTEX_POINT('',#19461);
#3798=VERTEX_POINT('',#19465);
#3799=VERTEX_POINT('',#19466);
#3800=VERTEX_POINT('',#19471);
#3801=VERTEX_POINT('',#19472);
#3802=VERTEX_POINT('',#19474);
#3803=VERTEX_POINT('',#19479);
#3804=VERTEX_POINT('',#19526);
#3805=VERTEX_POINT('',#19528);
#3806=VERTEX_POINT('',#19530);
#3807=VERTEX_POINT('',#19532);
#3808=VERTEX_POINT('',#19582);
#3809=VERTEX_POINT('',#19587);
#3810=VERTEX_POINT('',#19605);
#3811=VERTEX_POINT('',#19607);
#3812=VERTEX_POINT('',#19615);
#3813=VERTEX_POINT('',#19617);
#3814=VERTEX_POINT('',#19619);
#3815=VERTEX_POINT('',#19621);
#3816=VERTEX_POINT('',#19623);
#3817=VERTEX_POINT('',#19625);
#3818=VERTEX_POINT('',#19627);
#3819=VERTEX_POINT('',#19629);
#3820=VERTEX_POINT('',#19631);
#3821=VERTEX_POINT('',#19633);
#3822=VERTEX_POINT('',#19635);
#3823=VERTEX_POINT('',#19637);
#3824=VERTEX_POINT('',#19639);
#3825=VERTEX_POINT('',#19641);
#3826=VERTEX_POINT('',#19643);
#3827=VERTEX_POINT('',#19645);
#3828=VERTEX_POINT('',#19647);
#3829=VERTEX_POINT('',#19649);
#3830=VERTEX_POINT('',#19653);
#3831=VERTEX_POINT('',#19657);
#3832=VERTEX_POINT('',#19658);
#3833=VERTEX_POINT('',#19677);
#3834=VERTEX_POINT('',#19679);
#3835=VERTEX_POINT('',#19681);
#3836=VERTEX_POINT('',#19683);
#3837=VERTEX_POINT('',#19685);
#3838=VERTEX_POINT('',#19687);
#3839=VERTEX_POINT('',#19689);
#3840=VERTEX_POINT('',#19691);
#3841=VERTEX_POINT('',#19693);
#3842=VERTEX_POINT('',#19695);
#3843=VERTEX_POINT('',#19697);
#3844=VERTEX_POINT('',#19699);
#3845=VERTEX_POINT('',#19701);
#3846=VERTEX_POINT('',#19703);
#3847=VERTEX_POINT('',#19705);
#3848=VERTEX_POINT('',#19707);
#3849=VERTEX_POINT('',#19709);
#3850=VERTEX_POINT('',#19711);
#3851=VERTEX_POINT('',#19714);
#3852=VERTEX_POINT('',#19723);
#3853=VERTEX_POINT('',#19736);
#3854=VERTEX_POINT('',#19786);
#3855=VERTEX_POINT('',#19822);
#3856=VERTEX_POINT('',#19971);
#3857=VERTEX_POINT('',#32344);
#3858=VERTEX_POINT('',#32345);
#3859=VERTEX_POINT('',#32347);
#3860=VERTEX_POINT('',#32360);
#3861=VERTEX_POINT('',#32361);
#3862=VERTEX_POINT('',#32399);
#3863=VERTEX_POINT('',#32434);
#3864=VERTEX_POINT('',#32435);
#3865=VERTEX_POINT('',#32510);
#3866=VERTEX_POINT('',#32511);
#3867=VERTEX_POINT('',#32586);
#3868=VERTEX_POINT('',#32587);
#3869=VERTEX_POINT('',#32662);
#3870=VERTEX_POINT('',#32663);
#3871=VERTEX_POINT('',#32738);
#3872=VERTEX_POINT('',#32739);
#3873=VERTEX_POINT('',#32814);
#3874=VERTEX_POINT('',#32815);
#3875=VERTEX_POINT('',#32890);
#3876=VERTEX_POINT('',#32891);
#3877=VERTEX_POINT('',#32966);
#3878=VERTEX_POINT('',#32967);
#3879=VERTEX_POINT('',#33042);
#3880=VERTEX_POINT('',#33043);
#3881=VERTEX_POINT('',#33118);
#3882=VERTEX_POINT('',#33119);
#3883=VERTEX_POINT('',#33194);
#3884=VERTEX_POINT('',#33195);
#3885=VERTEX_POINT('',#33270);
#3886=VERTEX_POINT('',#33271);
#3887=VERTEX_POINT('',#33346);
#3888=VERTEX_POINT('',#33347);
#3889=VERTEX_POINT('',#33422);
#3890=VERTEX_POINT('',#33423);
#3891=VERTEX_POINT('',#33498);
#3892=VERTEX_POINT('',#33499);
#3893=VERTEX_POINT('',#33574);
#3894=VERTEX_POINT('',#33575);
#3895=VERTEX_POINT('',#33650);
#3896=VERTEX_POINT('',#33651);
#3897=VERTEX_POINT('',#33726);
#3898=VERTEX_POINT('',#33727);
#3899=VERTEX_POINT('',#33802);
#3900=VERTEX_POINT('',#33803);
#3901=VERTEX_POINT('',#33878);
#3902=VERTEX_POINT('',#33879);
#3903=VERTEX_POINT('',#33954);
#3904=VERTEX_POINT('',#33955);
#3905=VERTEX_POINT('',#34030);
#3906=VERTEX_POINT('',#34031);
#3907=VERTEX_POINT('',#34106);
#3908=VERTEX_POINT('',#34107);
#3909=VERTEX_POINT('',#34182);
#3910=VERTEX_POINT('',#34183);
#3911=VERTEX_POINT('',#34258);
#3912=VERTEX_POINT('',#34259);
#3913=VERTEX_POINT('',#34334);
#3914=VERTEX_POINT('',#34335);
#3915=VERTEX_POINT('',#34410);
#3916=VERTEX_POINT('',#34411);
#3917=VERTEX_POINT('',#34486);
#3918=VERTEX_POINT('',#34487);
#3919=VERTEX_POINT('',#34562);
#3920=VERTEX_POINT('',#34563);
#3921=VERTEX_POINT('',#34638);
#3922=VERTEX_POINT('',#34639);
#3923=VERTEX_POINT('',#34714);
#3924=VERTEX_POINT('',#34715);
#3925=VERTEX_POINT('',#34790);
#3926=VERTEX_POINT('',#34791);
#3927=VERTEX_POINT('',#34866);
#3928=VERTEX_POINT('',#34867);
#3929=VERTEX_POINT('',#34942);
#3930=VERTEX_POINT('',#34943);
#3931=VERTEX_POINT('',#35018);
#3932=VERTEX_POINT('',#35019);
#3933=VERTEX_POINT('',#35094);
#3934=VERTEX_POINT('',#35095);
#3935=VERTEX_POINT('',#35170);
#3936=VERTEX_POINT('',#35171);
#3937=VERTEX_POINT('',#35246);
#3938=VERTEX_POINT('',#35247);
#3939=VERTEX_POINT('',#35322);
#3940=VERTEX_POINT('',#35323);
#3941=VERTEX_POINT('',#35325);
#3942=VERTEX_POINT('',#35396);
#3943=VERTEX_POINT('',#35398);
#3944=VERTEX_POINT('',#35403);
#3945=VERTEX_POINT('',#35404);
#3946=VERTEX_POINT('',#35437);
#3947=VERTEX_POINT('',#35439);
#3948=VERTEX_POINT('',#35474);
#3949=VERTEX_POINT('',#35475);
#3950=VERTEX_POINT('',#35508);
#3951=VERTEX_POINT('',#35510);
#3952=VERTEX_POINT('',#35545);
#3953=VERTEX_POINT('',#35546);
#3954=VERTEX_POINT('',#35579);
#3955=VERTEX_POINT('',#35581);
#3956=VERTEX_POINT('',#35616);
#3957=VERTEX_POINT('',#35617);
#3958=VERTEX_POINT('',#35650);
#3959=VERTEX_POINT('',#35652);
#3960=VERTEX_POINT('',#35687);
#3961=VERTEX_POINT('',#35688);
#3962=VERTEX_POINT('',#35721);
#3963=VERTEX_POINT('',#35723);
#3964=VERTEX_POINT('',#35758);
#3965=VERTEX_POINT('',#35759);
#3966=VERTEX_POINT('',#35792);
#3967=VERTEX_POINT('',#35794);
#3968=VERTEX_POINT('',#35829);
#3969=VERTEX_POINT('',#35830);
#3970=VERTEX_POINT('',#35863);
#3971=VERTEX_POINT('',#35865);
#3972=VERTEX_POINT('',#35900);
#3973=VERTEX_POINT('',#35901);
#3974=VERTEX_POINT('',#35934);
#3975=VERTEX_POINT('',#35936);
#3976=VERTEX_POINT('',#35971);
#3977=VERTEX_POINT('',#35972);
#3978=VERTEX_POINT('',#36005);
#3979=VERTEX_POINT('',#36007);
#3980=VERTEX_POINT('',#36042);
#3981=VERTEX_POINT('',#36043);
#3982=VERTEX_POINT('',#36076);
#3983=VERTEX_POINT('',#36078);
#3984=VERTEX_POINT('',#36113);
#3985=VERTEX_POINT('',#36115);
#3986=VERTEX_POINT('',#36117);
#3987=VERTEX_POINT('',#36119);
#3988=VERTEX_POINT('',#36152);
#3989=VERTEX_POINT('',#36154);
#3990=VERTEX_POINT('',#36187);
#3991=VERTEX_POINT('',#36189);
#3992=VERTEX_POINT('',#36222);
#3993=VERTEX_POINT('',#36224);
#3994=VERTEX_POINT('',#36257);
#3995=VERTEX_POINT('',#36259);
#3996=VERTEX_POINT('',#36292);
#3997=VERTEX_POINT('',#36294);
#3998=VERTEX_POINT('',#36327);
#3999=VERTEX_POINT('',#36329);
#4000=VERTEX_POINT('',#36362);
#4001=VERTEX_POINT('',#36364);
#4002=VERTEX_POINT('',#36407);
#4003=VERTEX_POINT('',#36409);
#4004=VERTEX_POINT('',#36442);
#4005=VERTEX_POINT('',#36444);
#4006=VERTEX_POINT('',#36477);
#4007=VERTEX_POINT('',#36479);
#4008=VERTEX_POINT('',#36512);
#4009=VERTEX_POINT('',#36514);
#4010=VERTEX_POINT('',#36547);
#4011=VERTEX_POINT('',#36549);
#4012=VERTEX_POINT('',#36582);
#4013=VERTEX_POINT('',#36584);
#4014=VERTEX_POINT('',#36617);
#4015=VERTEX_POINT('',#36619);
#4016=VERTEX_POINT('',#36652);
#4017=VERTEX_POINT('',#36654);
#4018=VERTEX_POINT('',#36689);
#4019=VERTEX_POINT('',#36691);
#4020=VERTEX_POINT('',#36698);
#4021=VERTEX_POINT('',#36700);
#4022=VERTEX_POINT('',#36733);
#4023=VERTEX_POINT('',#36735);
#4024=VERTEX_POINT('',#36768);
#4025=VERTEX_POINT('',#36770);
#4026=VERTEX_POINT('',#36803);
#4027=VERTEX_POINT('',#36805);
#4028=VERTEX_POINT('',#36838);
#4029=VERTEX_POINT('',#36840);
#4030=VERTEX_POINT('',#36873);
#4031=VERTEX_POINT('',#36875);
#4032=VERTEX_POINT('',#36908);
#4033=VERTEX_POINT('',#36910);
#4034=VERTEX_POINT('',#36943);
#4035=VERTEX_POINT('',#36945);
#4036=VERTEX_POINT('',#36978);
#4037=VERTEX_POINT('',#36980);
#4038=VERTEX_POINT('',#37013);
#4039=VERTEX_POINT('',#37015);
#4040=VERTEX_POINT('',#37048);
#4041=VERTEX_POINT('',#37050);
#4042=VERTEX_POINT('',#37083);
#4043=VERTEX_POINT('',#37085);
#4044=VERTEX_POINT('',#37118);
#4045=VERTEX_POINT('',#37120);
#4046=VERTEX_POINT('',#37153);
#4047=VERTEX_POINT('',#37155);
#4048=VERTEX_POINT('',#37188);
#4049=VERTEX_POINT('',#37190);
#4050=VERTEX_POINT('',#37223);
#4051=VERTEX_POINT('',#37225);
#4052=VERTEX_POINT('',#37331);
#4053=VERTEX_POINT('',#37332);
#4054=VERTEX_POINT('',#37372);
#4055=VERTEX_POINT('',#37383);
#4056=VERTEX_POINT('',#44277);
#4057=VERTEX_POINT('',#44278);
#4058=VERTEX_POINT('',#44317);
#4059=VERTEX_POINT('',#44356);
#4060=VERTEX_POINT('',#44357);
#4061=VERTEX_POINT('',#44359);
#4062=VERTEX_POINT('',#44361);
#4063=VERTEX_POINT('',#44365);
#4064=VERTEX_POINT('',#44366);
#4065=VERTEX_POINT('',#44368);
#4066=VERTEX_POINT('',#44370);
#4067=VERTEX_POINT('',#44374);
#4068=VERTEX_POINT('',#44376);
#4069=VERTEX_POINT('',#44380);
#4070=VERTEX_POINT('',#44382);
#4071=VERTEX_POINT('',#44386);
#4072=VERTEX_POINT('',#44388);
#4073=VERTEX_POINT('',#44392);
#4074=VERTEX_POINT('',#44393);
#4075=VERTEX_POINT('',#44395);
#4076=VERTEX_POINT('',#44397);
#4077=VERTEX_POINT('',#44443);
#4078=VERTEX_POINT('',#44444);
#4079=VERTEX_POINT('',#44446);
#4080=VERTEX_POINT('',#44448);
#4081=VERTEX_POINT('',#44459);
#4082=VERTEX_POINT('',#44460);
#4083=VERTEX_POINT('',#44462);
#4084=VERTEX_POINT('',#44464);
#4085=VERTEX_POINT('',#44471);
#4086=VERTEX_POINT('',#44472);
#4087=VERTEX_POINT('',#44474);
#4088=VERTEX_POINT('',#44476);
#4089=VERTEX_POINT('',#44480);
#4090=VERTEX_POINT('',#44481);
#4091=VERTEX_POINT('',#44483);
#4092=VERTEX_POINT('',#44485);
#4093=VERTEX_POINT('',#44526);
#4094=VERTEX_POINT('',#44528);
#4095=VERTEX_POINT('',#44530);
#4096=VERTEX_POINT('',#44532);
#4097=VERTEX_POINT('',#44570);
#4098=VERTEX_POINT('',#44572);
#4099=VERTEX_POINT('',#44576);
#4100=VERTEX_POINT('',#44577);
#4101=VERTEX_POINT('',#44579);
#4102=VERTEX_POINT('',#44581);
#4103=VERTEX_POINT('',#44585);
#4104=VERTEX_POINT('',#44586);
#4105=VERTEX_POINT('',#44588);
#4106=VERTEX_POINT('',#44590);
#4107=VERTEX_POINT('',#44594);
#4108=VERTEX_POINT('',#44595);
#4109=VERTEX_POINT('',#44597);
#4110=VERTEX_POINT('',#44599);
#4111=VERTEX_POINT('',#44602);
#4112=VERTEX_POINT('',#44605);
#4113=VERTEX_POINT('',#44607);
#4114=VERTEX_POINT('',#44609);
#4115=VERTEX_POINT('',#44613);
#4116=VERTEX_POINT('',#44614);
#4117=VERTEX_POINT('',#44616);
#4118=VERTEX_POINT('',#44618);
#4119=VERTEX_POINT('',#44620);
#4120=VERTEX_POINT('',#44623);
#4121=VERTEX_POINT('',#44626);
#4122=VERTEX_POINT('',#44628);
#4123=VERTEX_POINT('',#44633);
#4124=VERTEX_POINT('',#44635);
#4125=VERTEX_POINT('',#44637);
#4126=VERTEX_POINT('',#44639);
#4127=VERTEX_POINT('',#44643);
#4128=VERTEX_POINT('',#44645);
#4129=VERTEX_POINT('',#44647);
#4130=VERTEX_POINT('',#44649);
#4131=VERTEX_POINT('',#44651);
#4132=VERTEX_POINT('',#44653);
#4133=VERTEX_POINT('',#44657);
#4134=VERTEX_POINT('',#44658);
#4135=VERTEX_POINT('',#44660);
#4136=VERTEX_POINT('',#44662);
#4137=VERTEX_POINT('',#44669);
#4138=VERTEX_POINT('',#44671);
#4139=VERTEX_POINT('',#44675);
#4140=VERTEX_POINT('',#44677);
#4141=VERTEX_POINT('',#44685);
#4142=VERTEX_POINT('',#44717);
#4143=VERTEX_POINT('',#44719);
#4144=VERTEX_POINT('',#44721);
#4145=VERTEX_POINT('',#44723);
#4146=VERTEX_POINT('',#44752);
#4147=VERTEX_POINT('',#44765);
#4148=VERTEX_POINT('',#44778);
#4149=VERTEX_POINT('',#44780);
#4150=VERTEX_POINT('',#44782);
#4151=VERTEX_POINT('',#44784);
#4152=VERTEX_POINT('',#44792);
#4153=VERTEX_POINT('',#44794);
#4154=VERTEX_POINT('',#44796);
#4155=VERTEX_POINT('',#44798);
#4156=VERTEX_POINT('',#44800);
#4157=VERTEX_POINT('',#44802);
#4158=VERTEX_POINT('',#44804);
#4159=VERTEX_POINT('',#44806);
#4160=VERTEX_POINT('',#44808);
#4161=VERTEX_POINT('',#44810);
#4162=VERTEX_POINT('',#44812);
#4163=VERTEX_POINT('',#44814);
#4164=VERTEX_POINT('',#44816);
#4165=VERTEX_POINT('',#44819);
#4166=VERTEX_POINT('',#44822);
#4167=VERTEX_POINT('',#44826);
#4168=VERTEX_POINT('',#44843);
#4169=VERTEX_POINT('',#44847);
#4170=VERTEX_POINT('',#44848);
#4171=VERTEX_POINT('',#44850);
#4172=VERTEX_POINT('',#44852);
#4173=VERTEX_POINT('',#44856);
#4174=VERTEX_POINT('',#44865);
#4175=VERTEX_POINT('',#44866);
#4176=VERTEX_POINT('',#44889);
#4177=VERTEX_POINT('',#44892);
#4178=VERTEX_POINT('',#44895);
#4179=VERTEX_POINT('',#44897);
#4180=VERTEX_POINT('',#44899);
#4181=VERTEX_POINT('',#44901);
#4182=VERTEX_POINT('',#44903);
#4183=VERTEX_POINT('',#44905);
#4184=VERTEX_POINT('',#44907);
#4185=VERTEX_POINT('',#44909);
#4186=VERTEX_POINT('',#44911);
#4187=VERTEX_POINT('',#44913);
#4188=VERTEX_POINT('',#44915);
#4189=VERTEX_POINT('',#44917);
#4190=VERTEX_POINT('',#44919);
#4191=VERTEX_POINT('',#45009);
#4192=VERTEX_POINT('',#45011);
#4193=VERTEX_POINT('',#45015);
#4194=VERTEX_POINT('',#45019);
#4195=VERTEX_POINT('',#45247);
#4196=VERTEX_POINT('',#45248);
#4197=VERTEX_POINT('',#45250);
#4198=VERTEX_POINT('',#45265);
#4199=VERTEX_POINT('',#45267);
#4200=VERTEX_POINT('',#45289);
#4201=VERTEX_POINT('',#45290);
#4202=VERTEX_POINT('',#45292);
#4203=VERTEX_POINT('',#45307);
#4204=VERTEX_POINT('',#45309);
#4205=VERTEX_POINT('',#45333);
#4206=VERTEX_POINT('',#45334);
#4207=VERTEX_POINT('',#45336);
#4208=VERTEX_POINT('',#45359);
#4209=VERTEX_POINT('',#45378);
#4210=VERTEX_POINT('',#45379);
#4211=VERTEX_POINT('',#45381);
#4212=VERTEX_POINT('',#45404);
#4213=VERTEX_POINT('',#45423);
#4214=VERTEX_POINT('',#45424);
#4215=VERTEX_POINT('',#45426);
#4216=VERTEX_POINT('',#45428);
#4217=VERTEX_POINT('',#45432);
#4218=VERTEX_POINT('',#45434);
#4219=VERTEX_POINT('',#45438);
#4220=VERTEX_POINT('',#45440);
#4221=VERTEX_POINT('',#45444);
#4222=VERTEX_POINT('',#45446);
#4223=VERTEX_POINT('',#45450);
#4224=VERTEX_POINT('',#45452);
#4225=VERTEX_POINT('',#45456);
#4226=VERTEX_POINT('',#45458);
#4227=VERTEX_POINT('',#45462);
#4228=VERTEX_POINT('',#45464);
#4229=VERTEX_POINT('',#45468);
#4230=VERTEX_POINT('',#45470);
#4231=VERTEX_POINT('',#45474);
#4232=VERTEX_POINT('',#45475);
#4233=VERTEX_POINT('',#45483);
#4234=VERTEX_POINT('',#45487);
#4235=VERTEX_POINT('',#45491);
#4236=VERTEX_POINT('',#45493);
#4237=VERTEX_POINT('',#45497);
#4238=VERTEX_POINT('',#45498);
#4239=VERTEX_POINT('',#45500);
#4240=VERTEX_POINT('',#45502);
#4241=VERTEX_POINT('',#45504);
#4242=VERTEX_POINT('',#45510);
#4243=VERTEX_POINT('',#45512);
#4244=VERTEX_POINT('',#45514);
#4245=VERTEX_POINT('',#45516);
#4246=VERTEX_POINT('',#45518);
#4247=VERTEX_POINT('',#45520);
#4248=VERTEX_POINT('',#45525);
#4249=VERTEX_POINT('',#45527);
#4250=VERTEX_POINT('',#45529);
#4251=VERTEX_POINT('',#45531);
#4252=VERTEX_POINT('',#45533);
#4253=VERTEX_POINT('',#45535);
#4254=VERTEX_POINT('',#45539);
#4255=VERTEX_POINT('',#45540);
#4256=VERTEX_POINT('',#45542);
#4257=VERTEX_POINT('',#45544);
#4258=VERTEX_POINT('',#45548);
#4259=VERTEX_POINT('',#45550);
#4260=VERTEX_POINT('',#45557);
#4261=VERTEX_POINT('',#45558);
#4262=VERTEX_POINT('',#45563);
#4263=VERTEX_POINT('',#45564);
#4264=VERTEX_POINT('',#45566);
#4265=VERTEX_POINT('',#45568);
#4266=VERTEX_POINT('',#45571);
#4267=VERTEX_POINT('',#45575);
#4268=VERTEX_POINT('',#45576);
#4269=VERTEX_POINT('',#45581);
#4270=VERTEX_POINT('',#45582);
#4271=VERTEX_POINT('',#45584);
#4272=VERTEX_POINT('',#45586);
#4273=VERTEX_POINT('',#45590);
#4274=VERTEX_POINT('',#45591);
#4275=VERTEX_POINT('',#45599);
#4276=VERTEX_POINT('',#45600);
#4277=VERTEX_POINT('',#45602);
#4278=VERTEX_POINT('',#45604);
#4279=VERTEX_POINT('',#45610);
#4280=VERTEX_POINT('',#45612);
#4281=VERTEX_POINT('',#45614);
#4282=VERTEX_POINT('',#45619);
#4283=VERTEX_POINT('',#45621);
#4284=VERTEX_POINT('',#45623);
#4285=VERTEX_POINT('',#45627);
#4286=VERTEX_POINT('',#45629);
#4287=VERTEX_POINT('',#45631);
#4288=VERTEX_POINT('',#45633);
#4289=VERTEX_POINT('',#45643);
#4290=VERTEX_POINT('',#45648);
#4291=VERTEX_POINT('',#45851);
#4292=VERTEX_POINT('',#45866);
#4293=VERTEX_POINT('',#45872);
#4294=VERTEX_POINT('',#45887);
#4295=VERTEX_POINT('',#45900);
#4296=VERTEX_POINT('',#45902);
#4297=VERTEX_POINT('',#45905);
#4298=VERTEX_POINT('',#45907);
#4299=VERTEX_POINT('',#45910);
#4300=VERTEX_POINT('',#45912);
#4301=VERTEX_POINT('',#45919);
#4302=VERTEX_POINT('',#45922);
#4303=VERTEX_POINT('',#45924);
#4304=VERTEX_POINT('',#45928);
#4305=VERTEX_POINT('',#45934);
#4306=VERTEX_POINT('',#45936);
#4307=VERTEX_POINT('',#45938);
#4308=VERTEX_POINT('',#45940);
#4309=VERTEX_POINT('',#45944);
#4310=VERTEX_POINT('',#45945);
#4311=VERTEX_POINT('',#45947);
#4312=VERTEX_POINT('',#45949);
#4313=VERTEX_POINT('',#45951);
#4314=VERTEX_POINT('',#45953);
#4315=VERTEX_POINT('',#45955);
#4316=VERTEX_POINT('',#45962);
#4317=VERTEX_POINT('',#46015);
#4318=VERTEX_POINT('',#46017);
#4319=VERTEX_POINT('',#46083);
#4320=VERTEX_POINT('',#46084);
#4321=VERTEX_POINT('',#46086);
#4322=VERTEX_POINT('',#46089);
#4323=VERTEX_POINT('',#46093);
#4324=VERTEX_POINT('',#46094);
#4325=VERTEX_POINT('',#46096);
#4326=VERTEX_POINT('',#46098);
#4327=VERTEX_POINT('',#46113);
#4328=VERTEX_POINT('',#46114);
#4329=VERTEX_POINT('',#46121);
#4330=VERTEX_POINT('',#46128);
#4331=VERTEX_POINT('',#46130);
#4332=VERTEX_POINT('',#46139);
#4333=VERTEX_POINT('',#46155);
#4334=VERTEX_POINT('',#46156);
#4335=VERTEX_POINT('',#46158);
#4336=VERTEX_POINT('',#46160);
#4337=VERTEX_POINT('',#46248);
#4338=VERTEX_POINT('',#46250);
#4339=VERTEX_POINT('',#46397);
#4340=VERTEX_POINT('',#46399);
#4341=VERTEX_POINT('',#46406);
#4342=VERTEX_POINT('',#46415);
#4343=VERTEX_POINT('',#46557);
#4344=VERTEX_POINT('',#46570);
#4345=VERTEX_POINT('',#46629);
#4346=VERTEX_POINT('',#46648);
#4347=VERTEX_POINT('',#46650);
#4348=VERTEX_POINT('',#46669);
#4349=VERTEX_POINT('',#47415);
#4350=VERTEX_POINT('',#47417);
#4351=VERTEX_POINT('',#47421);
#4352=VERTEX_POINT('',#47422);
#4353=VERTEX_POINT('',#47424);
#4354=VERTEX_POINT('',#47426);
#4355=VERTEX_POINT('',#47430);
#4356=VERTEX_POINT('',#47432);
#4357=VERTEX_POINT('',#47436);
#4358=VERTEX_POINT('',#47437);
#4359=VERTEX_POINT('',#47439);
#4360=VERTEX_POINT('',#47441);
#4361=VERTEX_POINT('',#47445);
#4362=VERTEX_POINT('',#47447);
#4363=VERTEX_POINT('',#47451);
#4364=VERTEX_POINT('',#47453);
#4365=VERTEX_POINT('',#47464);
#4366=VERTEX_POINT('',#47465);
#4367=VERTEX_POINT('',#47468);
#4368=VERTEX_POINT('',#47470);
#4369=VERTEX_POINT('',#47472);
#4370=VERTEX_POINT('',#47474);
#4371=VERTEX_POINT('',#47478);
#4372=VERTEX_POINT('',#47479);
#4373=VERTEX_POINT('',#47482);
#4374=VERTEX_POINT('',#47484);
#4375=VERTEX_POINT('',#47486);
#4376=VERTEX_POINT('',#47488);
#4377=VERTEX_POINT('',#47492);
#4378=VERTEX_POINT('',#47493);
#4379=VERTEX_POINT('',#47498);
#4380=VERTEX_POINT('',#47499);
#4381=VERTEX_POINT('',#47504);
#4382=VERTEX_POINT('',#47505);
#4383=VERTEX_POINT('',#47510);
#4384=VERTEX_POINT('',#47511);
#4385=VERTEX_POINT('',#47516);
#4386=VERTEX_POINT('',#47517);
#4387=VERTEX_POINT('',#47522);
#4388=VERTEX_POINT('',#47523);
#4389=EDGE_CURVE('',#3532,#3532,#3124,.T.);
#4390=EDGE_CURVE('',#3533,#3533,#3125,.T.);
#4391=EDGE_CURVE('',#3533,#3534,#883,.T.);
#4392=EDGE_CURVE('',#3534,#3534,#3126,.T.);
#4393=EDGE_CURVE('',#3535,#3535,#3127,.T.);
#4394=EDGE_CURVE('',#3536,#3537,#3128,.T.);
#4395=EDGE_CURVE('',#3537,#3536,#3129,.T.);
#4396=EDGE_CURVE('',#3536,#3538,#3130,.T.);
#4397=EDGE_CURVE('',#3539,#3538,#3131,.T.);
#4398=EDGE_CURVE('',#3538,#3539,#3132,.T.);
#4399=EDGE_CURVE('',#3540,#3540,#3133,.T.);
#4400=EDGE_CURVE('',#3540,#3541,#3134,.T.);
#4401=EDGE_CURVE('',#3542,#3541,#3135,.T.);
#4402=EDGE_CURVE('',#3541,#3542,#3136,.T.);
#4403=EDGE_CURVE('',#3542,#3543,#3137,.T.);
#4404=EDGE_CURVE('',#3543,#3543,#3138,.T.);
#4405=EDGE_CURVE('',#3544,#3544,#3139,.T.);
#4406=EDGE_CURVE('',#3544,#3537,#3140,.T.);
#4407=EDGE_CURVE('',#3539,#3545,#884,.T.);
#4408=EDGE_CURVE('',#3546,#3545,#3141,.T.);
#4409=EDGE_CURVE('',#3547,#3546,#3142,.T.);
#4410=EDGE_CURVE('',#3545,#3547,#3143,.T.);
#4411=EDGE_CURVE('',#3548,#3549,#3144,.T.);
#4412=EDGE_CURVE('',#3548,#3547,#148,.T.);
#4413=EDGE_CURVE('',#3549,#3546,#149,.T.);
#4414=EDGE_CURVE('',#3550,#3551,#3145,.T.);
#4415=EDGE_CURVE('',#3550,#3548,#150,.T.);
#4416=EDGE_CURVE('',#3551,#3549,#151,.T.);
#4417=EDGE_CURVE('',#3552,#3553,#3146,.T.);
#4418=EDGE_CURVE('',#3552,#3550,#152,.T.);
#4419=EDGE_CURVE('',#3553,#3551,#153,.T.);
#4420=EDGE_CURVE('',#3553,#3540,#885,.T.);
#4421=EDGE_CURVE('',#3553,#3552,#3147,.T.);
#4422=EDGE_CURVE('',#3549,#3548,#3148,.T.);
#4423=EDGE_CURVE('',#3551,#3550,#3149,.T.);
#4424=EDGE_CURVE('',#3554,#3554,#3150,.T.);
#4425=EDGE_CURVE('',#3555,#3555,#3151,.T.);
#4426=EDGE_CURVE('',#3555,#3556,#886,.T.);
#4427=EDGE_CURVE('',#3556,#3556,#3152,.T.);
#4428=EDGE_CURVE('',#3557,#3557,#3153,.T.);
#4429=EDGE_CURVE('',#3558,#3559,#3154,.T.);
#4430=EDGE_CURVE('',#3560,#3559,#887,.T.);
#4431=EDGE_CURVE('',#3560,#3561,#3155,.T.);
#4432=EDGE_CURVE('',#3561,#3562,#888,.T.);
#4433=EDGE_CURVE('',#3563,#3562,#3156,.T.);
#4434=EDGE_CURVE('',#3564,#3563,#889,.T.);
#4435=EDGE_CURVE('',#3565,#3564,#3157,.T.);
#4436=EDGE_CURVE('',#3566,#3565,#154,.T.);
#4437=EDGE_CURVE('',#3558,#3566,#890,.T.);
#4438=EDGE_CURVE('',#3567,#3568,#3158,.T.);
#4439=EDGE_CURVE('',#3569,#3567,#3159,.T.);
#4440=EDGE_CURVE('',#3570,#3569,#3160,.T.);
#4441=EDGE_CURVE('',#3568,#3570,#155,.T.);
#4442=EDGE_CURVE('',#3571,#3572,#3161,.T.);
#4443=EDGE_CURVE('',#3573,#3571,#3162,.T.);
#4444=EDGE_CURVE('',#3574,#3573,#3163,.T.);
#4445=EDGE_CURVE('',#3572,#3574,#156,.T.);
#4446=EDGE_CURVE('',#3575,#3576,#3164,.T.);
#4447=EDGE_CURVE('',#3575,#3577,#157,.T.);
#4448=EDGE_CURVE('',#3578,#3577,#3165,.T.);
#4449=EDGE_CURVE('',#3576,#3578,#3166,.T.);
#4450=EDGE_CURVE('',#3579,#3580,#3167,.T.);
#4451=EDGE_CURVE('',#3579,#3581,#158,.T.);
#4452=EDGE_CURVE('',#3582,#3581,#3168,.T.);
#4453=EDGE_CURVE('',#3580,#3582,#3169,.T.);
#4454=EDGE_CURVE('',#3583,#3584,#3170,.T.);
#4455=EDGE_CURVE('',#3582,#3583,#159,.T.);
#4456=EDGE_CURVE('',#3581,#3584,#160,.T.);
#4457=EDGE_CURVE('',#3585,#3586,#3171,.T.);
#4458=EDGE_CURVE('',#3586,#3575,#161,.T.);
#4459=EDGE_CURVE('',#3585,#3576,#162,.T.);
#4460=EDGE_CURVE('',#3587,#3587,#3172,.T.);
#4461=EDGE_CURVE('',#3587,#3588,#891,.T.);
#4462=EDGE_CURVE('',#3588,#3588,#3173,.T.);
#4463=EDGE_CURVE('',#3589,#3589,#3174,.T.);
#4464=EDGE_CURVE('',#3589,#3590,#892,.T.);
#4465=EDGE_CURVE('',#3590,#3590,#3175,.T.);
#4466=EDGE_CURVE('',#3591,#3562,#3176,.T.);
#4467=EDGE_CURVE('',#3561,#3592,#163,.T.);
#4468=EDGE_CURVE('',#3593,#3592,#893,.T.);
#4469=EDGE_CURVE('',#3593,#3594,#3177,.T.);
#4470=EDGE_CURVE('',#3591,#3594,#894,.T.);
#4471=EDGE_CURVE('',#3595,#3596,#3178,.T.);
#4472=EDGE_CURVE('',#3597,#3596,#895,.T.);
#4473=EDGE_CURVE('',#3597,#3558,#164,.T.);
#4474=EDGE_CURVE('',#3566,#3598,#3179,.T.);
#4475=EDGE_CURVE('',#3595,#3598,#896,.T.);
#4476=EDGE_CURVE('',#3599,#3600,#165,.T.);
#4477=EDGE_CURVE('',#3601,#3600,#897,.T.);
#4478=EDGE_CURVE('',#3602,#3601,#166,.F.);
#4479=EDGE_CURVE('',#3603,#3602,#898,.T.);
#4480=EDGE_CURVE('',#3604,#3603,#3180,.T.);
#4481=EDGE_CURVE('',#3605,#3604,#899,.T.);
#4482=EDGE_CURVE('',#3606,#3605,#167,.T.);
#4483=EDGE_CURVE('',#3606,#3607,#168,.T.);
#4484=EDGE_CURVE('',#3608,#3607,#169,.T.);
#4485=EDGE_CURVE('',#3608,#3609,#900,.T.);
#4486=EDGE_CURVE('',#3610,#3609,#3181,.T.);
#4487=EDGE_CURVE('',#3610,#3611,#901,.T.);
#4488=EDGE_CURVE('',#3612,#3611,#170,.F.);
#4489=EDGE_CURVE('',#3599,#3612,#902,.T.);
#4490=EDGE_CURVE('',#3613,#3614,#171,.T.);
#4491=EDGE_CURVE('',#3614,#3615,#903,.T.);
#4492=EDGE_CURVE('',#3616,#3615,#172,.F.);
#4493=EDGE_CURVE('',#3613,#3616,#904,.T.);
#4494=EDGE_CURVE('',#3617,#3618,#173,.T.);
#4495=EDGE_CURVE('',#3618,#3619,#905,.T.);
#4496=EDGE_CURVE('',#3620,#3619,#174,.F.);
#4497=EDGE_CURVE('',#3620,#3621,#3182,.T.);
#4498=EDGE_CURVE('',#3617,#3621,#906,.T.);
#4499=EDGE_CURVE('',#3622,#3623,#175,.F.);
#4500=EDGE_CURVE('',#3622,#3624,#907,.T.);
#4501=EDGE_CURVE('',#3625,#3624,#176,.F.);
#4502=EDGE_CURVE('',#3623,#3625,#908,.T.);
#4503=EDGE_CURVE('',#3626,#3627,#177,.F.);
#4504=EDGE_CURVE('',#3626,#3628,#909,.T.);
#4505=EDGE_CURVE('',#3629,#3628,#178,.F.);
#4506=EDGE_CURVE('',#3627,#3629,#910,.T.);
#4507=EDGE_CURVE('',#3630,#3631,#179,.F.);
#4508=EDGE_CURVE('',#3630,#3632,#911,.T.);
#4509=EDGE_CURVE('',#3633,#3632,#180,.F.);
#4510=EDGE_CURVE('',#3631,#3633,#912,.T.);
#4511=EDGE_CURVE('',#3634,#3635,#181,.F.);
#4512=EDGE_CURVE('',#3634,#3636,#913,.T.);
#4513=EDGE_CURVE('',#3637,#3636,#182,.F.);
#4514=EDGE_CURVE('',#3635,#3637,#914,.T.);
#4515=EDGE_CURVE('',#3638,#3639,#183,.F.);
#4516=EDGE_CURVE('',#3638,#3640,#915,.T.);
#4517=EDGE_CURVE('',#3641,#3640,#184,.F.);
#4518=EDGE_CURVE('',#3639,#3641,#916,.T.);
#4519=EDGE_CURVE('',#3642,#3643,#185,.F.);
#4520=EDGE_CURVE('',#3642,#3644,#917,.T.);
#4521=EDGE_CURVE('',#3645,#3644,#186,.F.);
#4522=EDGE_CURVE('',#3643,#3645,#918,.T.);
#4523=EDGE_CURVE('',#3646,#3647,#187,.F.);
#4524=EDGE_CURVE('',#3646,#3648,#919,.T.);
#4525=EDGE_CURVE('',#3649,#3648,#188,.F.);
#4526=EDGE_CURVE('',#3647,#3649,#920,.T.);
#4527=EDGE_CURVE('',#3650,#3651,#189,.T.);
#4528=EDGE_CURVE('',#3652,#3650,#190,.T.);
#4529=EDGE_CURVE('',#3653,#3652,#191,.T.);
#4530=EDGE_CURVE('',#3651,#3653,#192,.T.);
#4531=EDGE_CURVE('',#3654,#3655,#193,.T.);
#4532=EDGE_CURVE('',#3656,#3654,#194,.T.);
#4533=EDGE_CURVE('',#3657,#3656,#195,.T.);
#4534=EDGE_CURVE('',#3655,#3657,#196,.T.);
#4535=EDGE_CURVE('',#3658,#3659,#197,.T.);
#4536=EDGE_CURVE('',#3660,#3658,#198,.T.);
#4537=EDGE_CURVE('',#3661,#3660,#199,.T.);
#4538=EDGE_CURVE('',#3659,#3661,#200,.T.);
#4539=EDGE_CURVE('',#3662,#3663,#201,.T.);
#4540=EDGE_CURVE('',#3664,#3662,#202,.T.);
#4541=EDGE_CURVE('',#3665,#3664,#203,.T.);
#4542=EDGE_CURVE('',#3663,#3665,#204,.T.);
#4543=EDGE_CURVE('',#3666,#3667,#205,.T.);
#4544=EDGE_CURVE('',#3668,#3666,#206,.T.);
#4545=EDGE_CURVE('',#3669,#3668,#207,.T.);
#4546=EDGE_CURVE('',#3667,#3669,#208,.T.);
#4547=EDGE_CURVE('',#3670,#3671,#209,.T.);
#4548=EDGE_CURVE('',#3672,#3670,#210,.T.);
#4549=EDGE_CURVE('',#3673,#3672,#211,.T.);
#4550=EDGE_CURVE('',#3671,#3673,#212,.T.);
#4551=EDGE_CURVE('',#3616,#3617,#90,.T.);
#4552=EDGE_CURVE('',#3621,#3674,#921,.T.);
#4553=EDGE_CURVE('',#3674,#3675,#922,.T.);
#4554=EDGE_CURVE('',#3675,#3676,#213,.T.);
#4555=EDGE_CURVE('',#3676,#3677,#91,.T.);
#4556=EDGE_CURVE('',#3677,#3678,#214,.T.);
#4557=EDGE_CURVE('',#3678,#3679,#923,.T.);
#4558=EDGE_CURVE('',#3679,#3680,#215,.T.);
#4559=EDGE_CURVE('',#3680,#3681,#92,.T.);
#4560=EDGE_CURVE('',#3681,#3682,#216,.T.);
#4561=EDGE_CURVE('',#3682,#3683,#924,.T.);
#4562=EDGE_CURVE('',#3683,#3684,#217,.T.);
#4563=EDGE_CURVE('',#3684,#3685,#93,.T.);
#4564=EDGE_CURVE('',#3685,#3686,#218,.T.);
#4565=EDGE_CURVE('',#3686,#3687,#925,.T.);
#4566=EDGE_CURVE('',#3687,#3688,#219,.T.);
#4567=EDGE_CURVE('',#3688,#3689,#94,.T.);
#4568=EDGE_CURVE('',#3689,#3690,#220,.T.);
#4569=EDGE_CURVE('',#3690,#3691,#926,.T.);
#4570=EDGE_CURVE('',#3691,#3692,#221,.T.);
#4571=EDGE_CURVE('',#3692,#3693,#95,.T.);
#4572=EDGE_CURVE('',#3693,#3694,#222,.T.);
#4573=EDGE_CURVE('',#3694,#3695,#927,.T.);
#4574=EDGE_CURVE('',#3695,#3696,#223,.T.);
#4575=EDGE_CURVE('',#3696,#3697,#96,.T.);
#4576=EDGE_CURVE('',#3697,#3698,#224,.T.);
#4577=EDGE_CURVE('',#3698,#3699,#928,.T.);
#4578=EDGE_CURVE('',#3699,#3700,#225,.T.);
#4579=EDGE_CURVE('',#3700,#3701,#226,.T.);
#4580=EDGE_CURVE('',#3702,#3701,#929,.T.);
#4581=EDGE_CURVE('',#3702,#3703,#930,.T.);
#4582=EDGE_CURVE('',#3703,#3704,#3183,.T.);
#4583=EDGE_CURVE('',#3704,#3705,#931,.T.);
#4584=EDGE_CURVE('',#3705,#3565,#3184,.T.);
#4585=EDGE_CURVE('',#3706,#3564,#932,.T.);
#4586=EDGE_CURVE('',#3605,#3706,#227,.T.);
#4587=EDGE_CURVE('',#3603,#3604,#933,.T.);
#4588=EDGE_CURVE('',#3602,#3599,#97,.T.);
#4589=EDGE_CURVE('',#3612,#3613,#98,.T.);
#4590=EDGE_CURVE('',#3625,#3659,#228,.T.);
#4591=EDGE_CURVE('',#3661,#3623,#229,.T.);
#4592=EDGE_CURVE('',#3629,#3663,#230,.T.);
#4593=EDGE_CURVE('',#3665,#3627,#231,.T.);
#4594=EDGE_CURVE('',#3633,#3667,#232,.T.);
#4595=EDGE_CURVE('',#3669,#3631,#233,.T.);
#4596=EDGE_CURVE('',#3637,#3671,#234,.T.);
#4597=EDGE_CURVE('',#3673,#3635,#235,.T.);
#4598=EDGE_CURVE('',#3641,#3655,#236,.T.);
#4599=EDGE_CURVE('',#3657,#3639,#237,.T.);
#4600=EDGE_CURVE('',#3645,#3651,#238,.T.);
#4601=EDGE_CURVE('',#3653,#3643,#239,.T.);
#4602=EDGE_CURVE('',#3650,#3707,#240,.T.);
#4603=EDGE_CURVE('',#3707,#3708,#934,.T.);
#4604=EDGE_CURVE('',#3708,#3652,#241,.T.);
#4605=EDGE_CURVE('',#3654,#3709,#242,.T.);
#4606=EDGE_CURVE('',#3709,#3710,#935,.T.);
#4607=EDGE_CURVE('',#3710,#3656,#243,.T.);
#4608=EDGE_CURVE('',#3670,#3711,#244,.T.);
#4609=EDGE_CURVE('',#3711,#3712,#936,.T.);
#4610=EDGE_CURVE('',#3712,#3672,#245,.T.);
#4611=EDGE_CURVE('',#3666,#3713,#246,.T.);
#4612=EDGE_CURVE('',#3713,#3714,#937,.T.);
#4613=EDGE_CURVE('',#3714,#3668,#247,.T.);
#4614=EDGE_CURVE('',#3662,#3715,#248,.T.);
#4615=EDGE_CURVE('',#3715,#3716,#938,.T.);
#4616=EDGE_CURVE('',#3716,#3664,#249,.T.);
#4617=EDGE_CURVE('',#3658,#3717,#250,.T.);
#4618=EDGE_CURVE('',#3717,#3718,#939,.T.);
#4619=EDGE_CURVE('',#3718,#3660,#251,.T.);
#4620=EDGE_CURVE('',#3699,#3707,#59,.T.);
#4621=EDGE_CURVE('',#3708,#3698,#60,.T.);
#4622=EDGE_CURVE('',#3695,#3709,#61,.T.);
#4623=EDGE_CURVE('',#3710,#3694,#62,.T.);
#4624=EDGE_CURVE('',#3691,#3711,#63,.T.);
#4625=EDGE_CURVE('',#3712,#3690,#64,.T.);
#4626=EDGE_CURVE('',#3687,#3713,#65,.T.);
#4627=EDGE_CURVE('',#3714,#3686,#66,.T.);
#4628=EDGE_CURVE('',#3683,#3715,#67,.T.);
#4629=EDGE_CURVE('',#3716,#3682,#68,.T.);
#4630=EDGE_CURVE('',#3679,#3717,#69,.T.);
#4631=EDGE_CURVE('',#3718,#3678,#70,.T.);
#4632=EDGE_CURVE('',#3675,#3719,#71,.T.);
#4633=EDGE_CURVE('',#3719,#3674,#3185,.T.);
#4634=EDGE_CURVE('',#3620,#3719,#252,.T.);
#4635=EDGE_CURVE('',#3720,#3606,#253,.T.);
#4636=EDGE_CURVE('',#3720,#3721,#940,.T.);
#4637=EDGE_CURVE('',#3607,#3721,#254,.T.);
#4638=EDGE_CURVE('',#3722,#3608,#255,.T.);
#4639=EDGE_CURVE('',#3721,#3722,#256,.T.);
#4640=EDGE_CURVE('',#3706,#3720,#257,.T.);
#4641=EDGE_CURVE('',#3568,#3723,#941,.T.);
#4642=EDGE_CURVE('',#3723,#3724,#3186,.T.);
#4643=EDGE_CURVE('',#3724,#3725,#3187,.T.);
#4644=EDGE_CURVE('',#3725,#3579,#3188,.T.);
#4645=EDGE_CURVE('',#3580,#3567,#942,.T.);
#4646=EDGE_CURVE('',#3726,#3727,#258,.T.);
#4647=EDGE_CURVE('',#3727,#3593,#943,.T.);
#4648=EDGE_CURVE('',#3592,#3723,#3189,.T.);
#4649=EDGE_CURVE('',#3572,#3570,#944,.T.);
#4650=EDGE_CURVE('',#3574,#3728,#945,.T.);
#4651=EDGE_CURVE('',#3728,#3597,#3190,.T.);
#4652=EDGE_CURVE('',#3596,#3729,#946,.T.);
#4653=EDGE_CURVE('',#3729,#3730,#259,.T.);
#4654=EDGE_CURVE('',#3730,#3726,#947,.T.);
#4655=EDGE_CURVE('',#3594,#3731,#948,.T.);
#4656=EDGE_CURVE('',#3731,#3732,#949,.T.);
#4657=EDGE_CURVE('',#3591,#3732,#950,.T.);
#4658=EDGE_CURVE('',#3733,#3734,#951,.T.);
#4659=EDGE_CURVE('',#3734,#3735,#952,.T.);
#4660=EDGE_CURVE('',#3736,#3735,#953,.T.);
#4661=EDGE_CURVE('',#3733,#3736,#954,.T.);
#4662=EDGE_CURVE('',#3737,#3738,#260,.T.);
#4663=EDGE_CURVE('',#3738,#3739,#261,.T.);
#4664=EDGE_CURVE('',#3736,#3739,#955,.T.);
#4665=EDGE_CURVE('',#3735,#3740,#3191,.T.);
#4666=EDGE_CURVE('',#3740,#3741,#956,.T.);
#4667=EDGE_CURVE('',#3741,#3742,#3192,.T.);
#4668=EDGE_CURVE('',#3743,#3742,#957,.T.);
#4669=EDGE_CURVE('',#3743,#3744,#3193,.T.);
#4670=EDGE_CURVE('',#3745,#3744,#958,.T.);
#4671=EDGE_CURVE('',#3745,#3746,#3194,.T.);
#4672=EDGE_CURVE('',#3746,#3747,#959,.T.);
#4673=EDGE_CURVE('',#3747,#3702,#3195,.T.);
#4674=EDGE_CURVE('',#3701,#3748,#262,.T.);
#4675=EDGE_CURVE('',#3748,#3749,#263,.T.);
#4676=EDGE_CURVE('',#3750,#3749,#3196,.T.);
#4677=EDGE_CURVE('',#3750,#3751,#960,.T.);
#4678=EDGE_CURVE('',#3737,#3751,#3197,.T.);
#4679=EDGE_CURVE('',#3752,#3753,#961,.T.);
#4680=EDGE_CURVE('',#3752,#3754,#3198,.T.);
#4681=EDGE_CURVE('',#3755,#3754,#962,.T.);
#4682=EDGE_CURVE('',#3755,#3753,#3199,.T.);
#4683=EDGE_CURVE('',#3742,#3756,#264,.T.);
#4684=EDGE_CURVE('',#3756,#3757,#963,.T.);
#4685=EDGE_CURVE('',#3757,#3743,#265,.T.);
#4686=EDGE_CURVE('',#3598,#3752,#964,.T.);
#4687=EDGE_CURVE('',#3753,#3595,#965,.T.);
#4688=EDGE_CURVE('',#3754,#3747,#966,.T.);
#4689=EDGE_CURVE('',#3746,#3755,#967,.T.);
#4690=EDGE_CURVE('',#3744,#3758,#266,.T.);
#4691=EDGE_CURVE('',#3758,#3759,#968,.T.);
#4692=EDGE_CURVE('',#3759,#3760,#3200,.T.);
#4693=EDGE_CURVE('',#3760,#3761,#969,.T.);
#4694=EDGE_CURVE('',#3761,#3762,#3201,.T.);
#4695=EDGE_CURVE('',#3762,#3745,#970,.T.);
#4696=EDGE_CURVE('',#3740,#3763,#971,.T.);
#4697=EDGE_CURVE('',#3763,#3764,#3202,.T.);
#4698=EDGE_CURVE('',#3764,#3765,#972,.T.);
#4699=EDGE_CURVE('',#3765,#3766,#3203,.T.);
#4700=EDGE_CURVE('',#3766,#3767,#973,.T.);
#4701=EDGE_CURVE('',#3767,#3741,#267,.T.);
#4702=EDGE_CURVE('',#3731,#3734,#3204,.T.);
#4703=EDGE_CURVE('',#3733,#3732,#3205,.T.);
#4704=EDGE_CURVE('',#3767,#3756,#268,.T.);
#4705=EDGE_CURVE('',#3757,#3758,#269,.T.);
#4706=EDGE_CURVE('',#3768,#3769,#270,.T.);
#4707=EDGE_CURVE('',#3751,#3768,#271,.T.);
#4708=EDGE_CURVE('',#3769,#3750,#974,.T.);
#4709=EDGE_CURVE('',#3619,#3770,#99,.T.);
#4710=EDGE_CURVE('',#3615,#3618,#100,.T.);
#4711=EDGE_CURVE('',#3611,#3614,#101,.T.);
#4712=EDGE_CURVE('',#3610,#3609,#975,.T.);
#4713=EDGE_CURVE('',#3722,#3563,#976,.T.);
#4714=EDGE_CURVE('',#3771,#3739,#102,.T.);
#4715=EDGE_CURVE('',#3648,#3771,#272,.T.);
#4716=EDGE_CURVE('',#3772,#3646,#273,.T.);
#4717=EDGE_CURVE('',#3773,#3772,#103,.T.);
#4718=EDGE_CURVE('',#3644,#3773,#274,.T.);
#4719=EDGE_CURVE('',#3774,#3642,#275,.T.);
#4720=EDGE_CURVE('',#3775,#3774,#104,.T.);
#4721=EDGE_CURVE('',#3640,#3775,#276,.T.);
#4722=EDGE_CURVE('',#3776,#3638,#277,.T.);
#4723=EDGE_CURVE('',#3777,#3776,#105,.T.);
#4724=EDGE_CURVE('',#3636,#3777,#278,.T.);
#4725=EDGE_CURVE('',#3778,#3634,#279,.T.);
#4726=EDGE_CURVE('',#3779,#3778,#106,.T.);
#4727=EDGE_CURVE('',#3632,#3779,#280,.T.);
#4728=EDGE_CURVE('',#3780,#3630,#281,.T.);
#4729=EDGE_CURVE('',#3781,#3780,#107,.T.);
#4730=EDGE_CURVE('',#3628,#3781,#282,.T.);
#4731=EDGE_CURVE('',#3782,#3626,#283,.T.);
#4732=EDGE_CURVE('',#3783,#3782,#108,.T.);
#4733=EDGE_CURVE('',#3624,#3783,#284,.T.);
#4734=EDGE_CURVE('',#3784,#3622,#285,.T.);
#4735=EDGE_CURVE('',#3785,#3784,#977,.T.);
#4736=EDGE_CURVE('',#3770,#3785,#978,.T.);
#4737=EDGE_CURVE('',#3649,#3737,#286,.T.);
#4738=EDGE_CURVE('',#3768,#3647,#287,.T.);
#4739=EDGE_CURVE('',#3749,#3769,#288,.T.);
#4740=EDGE_CURVE('',#3577,#3786,#3206,.T.);
#4741=EDGE_CURVE('',#3786,#3787,#3207,.T.);
#4742=EDGE_CURVE('',#3787,#3728,#3208,.T.);
#4743=EDGE_CURVE('',#3573,#3578,#979,.T.);
#4744=EDGE_CURVE('',#3788,#3789,#980,.T.);
#4745=EDGE_CURVE('',#3788,#3790,#289,.T.);
#4746=EDGE_CURVE('',#3790,#3791,#290,.T.);
#4747=EDGE_CURVE('',#3791,#3571,#291,.T.);
#4748=EDGE_CURVE('',#3569,#3792,#292,.T.);
#4749=EDGE_CURVE('',#3792,#3793,#293,.T.);
#4750=EDGE_CURVE('',#3793,#3789,#294,.T.);
#4751=EDGE_CURVE('',#3794,#3795,#981,.T.);
#4752=EDGE_CURVE('',#3795,#3788,#295,.T.);
#4753=EDGE_CURVE('',#3789,#3796,#296,.T.);
#4754=EDGE_CURVE('',#3797,#3796,#982,.T.);
#4755=EDGE_CURVE('',#3794,#3797,#983,.T.);
#4756=EDGE_CURVE('',#3798,#3799,#984,.T.);
#4757=EDGE_CURVE('',#3799,#3794,#985,.T.);
#4758=EDGE_CURVE('',#3798,#3797,#986,.T.);
#4759=EDGE_CURVE('',#3800,#3801,#3209,.T.);
#4760=EDGE_CURVE('',#3800,#3802,#297,.T.);
#4761=EDGE_CURVE('',#3802,#3803,#298,.T.);
#4762=EDGE_CURVE('',#3803,#3804,#3210,.T.);
#4763=EDGE_CURVE('',#3804,#3805,#987,.T.);
#4764=EDGE_CURVE('',#3805,#3806,#3211,.T.);
#4765=EDGE_CURVE('',#3806,#3807,#299,.T.);
#4766=EDGE_CURVE('',#3807,#3808,#300,.T.);
#4767=EDGE_CURVE('',#3808,#3809,#3212,.T.);
#4768=EDGE_CURVE('',#3801,#3809,#988,.T.);
#4769=EDGE_CURVE('',#3808,#3586,#301,.T.);
#4770=EDGE_CURVE('',#3810,#3585,#989,.T.);
#4771=EDGE_CURVE('',#3810,#3811,#3213,.T.);
#4772=EDGE_CURVE('',#3811,#3795,#302,.T.);
#4773=EDGE_CURVE('',#3812,#3799,#990,.T.);
#4774=EDGE_CURVE('',#3813,#3812,#991,.T.);
#4775=EDGE_CURVE('',#3814,#3813,#992,.T.);
#4776=EDGE_CURVE('',#3815,#3814,#993,.T.);
#4777=EDGE_CURVE('',#3816,#3815,#994,.T.);
#4778=EDGE_CURVE('',#3817,#3816,#995,.T.);
#4779=EDGE_CURVE('',#3818,#3817,#996,.T.);
#4780=EDGE_CURVE('',#3819,#3818,#997,.T.);
#4781=EDGE_CURVE('',#3820,#3819,#998,.T.);
#4782=EDGE_CURVE('',#3821,#3820,#999,.T.);
#4783=EDGE_CURVE('',#3822,#3821,#1000,.T.);
#4784=EDGE_CURVE('',#3823,#3822,#1001,.T.);
#4785=EDGE_CURVE('',#3824,#3823,#1002,.T.);
#4786=EDGE_CURVE('',#3825,#3824,#1003,.T.);
#4787=EDGE_CURVE('',#3826,#3825,#1004,.T.);
#4788=EDGE_CURVE('',#3827,#3826,#1005,.T.);
#4789=EDGE_CURVE('',#3828,#3827,#1006,.T.);
#4790=EDGE_CURVE('',#3829,#3828,#1007,.T.);
#4791=EDGE_CURVE('',#3809,#3829,#1008,.T.);
#4792=EDGE_CURVE('',#3576,#3830,#1009,.T.);
#4793=EDGE_CURVE('',#3830,#3810,#1010,.T.);
#4794=EDGE_CURVE('',#3831,#3832,#1011,.T.);
#4795=EDGE_CURVE('',#3832,#3582,#1012,.T.);
#4796=EDGE_CURVE('',#3831,#3583,#1013,.T.);
#4797=EDGE_CURVE('',#3584,#3800,#303,.T.);
#4798=EDGE_CURVE('',#3801,#3833,#1014,.T.);
#4799=EDGE_CURVE('',#3833,#3834,#1015,.T.);
#4800=EDGE_CURVE('',#3834,#3835,#1016,.T.);
#4801=EDGE_CURVE('',#3835,#3836,#1017,.T.);
#4802=EDGE_CURVE('',#3836,#3837,#1018,.T.);
#4803=EDGE_CURVE('',#3837,#3838,#1019,.T.);
#4804=EDGE_CURVE('',#3838,#3839,#1020,.T.);
#4805=EDGE_CURVE('',#3839,#3840,#1021,.T.);
#4806=EDGE_CURVE('',#3840,#3841,#1022,.T.);
#4807=EDGE_CURVE('',#3841,#3842,#1023,.T.);
#4808=EDGE_CURVE('',#3842,#3843,#1024,.T.);
#4809=EDGE_CURVE('',#3843,#3844,#1025,.T.);
#4810=EDGE_CURVE('',#3844,#3845,#1026,.T.);
#4811=EDGE_CURVE('',#3845,#3846,#1027,.T.);
#4812=EDGE_CURVE('',#3846,#3847,#1028,.T.);
#4813=EDGE_CURVE('',#3847,#3848,#1029,.T.);
#4814=EDGE_CURVE('',#3848,#3849,#1030,.T.);
#4815=EDGE_CURVE('',#3849,#3850,#1031,.T.);
#4816=EDGE_CURVE('',#3850,#3798,#1032,.T.);
#4817=EDGE_CURVE('',#3796,#3851,#304,.T.);
#4818=EDGE_CURVE('',#3851,#3831,#3214,.T.);
#4819=EDGE_CURVE('',#3851,#3852,#305,.T.);
#4820=EDGE_CURVE('',#3852,#3832,#3215,.T.);
#4821=EDGE_CURVE('',#3830,#3853,#3216,.T.);
#4822=EDGE_CURVE('',#3853,#3811,#306,.T.);
#4823=EDGE_CURVE('',#3850,#3812,#1033,.T.);
#4824=EDGE_CURVE('',#3849,#3813,#1034,.T.);
#4825=EDGE_CURVE('',#3848,#3814,#1035,.T.);
#4826=EDGE_CURVE('',#3847,#3815,#1036,.T.);
#4827=EDGE_CURVE('',#3846,#3816,#1037,.T.);
#4828=EDGE_CURVE('',#3845,#3817,#1038,.T.);
#4829=EDGE_CURVE('',#3844,#3818,#1039,.T.);
#4830=EDGE_CURVE('',#3843,#3819,#1040,.T.);
#4831=EDGE_CURVE('',#3842,#3820,#1041,.T.);
#4832=EDGE_CURVE('',#3841,#3821,#1042,.T.);
#4833=EDGE_CURVE('',#3840,#3822,#1043,.T.);
#4834=EDGE_CURVE('',#3839,#3823,#1044,.T.);
#4835=EDGE_CURVE('',#3838,#3824,#1045,.T.);
#4836=EDGE_CURVE('',#3837,#3825,#1046,.T.);
#4837=EDGE_CURVE('',#3836,#3826,#1047,.T.);
#4838=EDGE_CURVE('',#3835,#3827,#1048,.T.);
#4839=EDGE_CURVE('',#3834,#3828,#1049,.T.);
#4840=EDGE_CURVE('',#3833,#3829,#1050,.T.);
#4841=EDGE_CURVE('',#3854,#3832,#3217,.T.);
#4842=EDGE_CURVE('',#3854,#3567,#109,.T.);
#4843=EDGE_CURVE('',#3852,#3854,#307,.T.);
#4844=EDGE_CURVE('',#3573,#3855,#110,.T.);
#4845=EDGE_CURVE('',#3830,#3855,#3218,.T.);
#4846=EDGE_CURVE('',#3855,#3853,#308,.T.);
#4847=EDGE_CURVE('',#3855,#3791,#3219,.T.);
#4848=EDGE_CURVE('',#3853,#3790,#3220,.T.);
#4849=EDGE_CURVE('',#3792,#3854,#3221,.T.);
#4850=EDGE_CURVE('',#3793,#3852,#3222,.T.);
#4851=EDGE_CURVE('',#3785,#3856,#3223,.T.);
#4852=EDGE_CURVE('',#3856,#3770,#72,.T.);
#4853=EDGE_CURVE('',#3784,#3856,#309,.T.);
#4854=EDGE_CURVE('',#3703,#3754,#3224,.T.);
#4855=EDGE_CURVE('',#3704,#3752,#3225,.T.);
#4856=EDGE_CURVE('',#3705,#3598,#3226,.T.);
#4857=EDGE_CURVE('',#3755,#3762,#3227,.T.);
#4858=EDGE_CURVE('',#3753,#3761,#3228,.T.);
#4859=EDGE_CURVE('',#3595,#3760,#3229,.T.);
#4860=EDGE_CURVE('',#3596,#3759,#3230,.T.);
#4861=EDGE_CURVE('',#3729,#3758,#3231,.T.);
#4862=EDGE_CURVE('',#3730,#3757,#3232,.T.);
#4863=EDGE_CURVE('',#3726,#3756,#3233,.T.);
#4864=EDGE_CURVE('',#3727,#3767,#3234,.T.);
#4865=EDGE_CURVE('',#3593,#3766,#3235,.T.);
#4866=EDGE_CURVE('',#3594,#3765,#3236,.T.);
#4867=EDGE_CURVE('',#3731,#3764,#3237,.T.);
#4868=EDGE_CURVE('',#3734,#3763,#3238,.T.);
#4869=EDGE_CURVE('',#3677,#3856,#73,.T.);
#4870=EDGE_CURVE('',#3676,#3620,#74,.T.);
#4871=EDGE_CURVE('',#3600,#3601,#3239,.T.);
#4872=EDGE_CURVE('',#3700,#3773,#75,.T.);
#4873=EDGE_CURVE('',#3748,#3772,#76,.T.);
#4874=EDGE_CURVE('',#3697,#3774,#77,.T.);
#4875=EDGE_CURVE('',#3696,#3775,#78,.T.);
#4876=EDGE_CURVE('',#3693,#3776,#79,.T.);
#4877=EDGE_CURVE('',#3692,#3777,#80,.T.);
#4878=EDGE_CURVE('',#3689,#3778,#81,.T.);
#4879=EDGE_CURVE('',#3688,#3779,#82,.T.);
#4880=EDGE_CURVE('',#3685,#3780,#83,.T.);
#4881=EDGE_CURVE('',#3684,#3781,#84,.T.);
#4882=EDGE_CURVE('',#3681,#3782,#85,.T.);
#4883=EDGE_CURVE('',#3680,#3783,#86,.T.);
#4884=EDGE_CURVE('',#3738,#3771,#87,.T.);
#4885=EDGE_CURVE('',#3804,#3560,#3240,.T.);
#4886=EDGE_CURVE('',#3559,#3805,#3241,.T.);
#4887=EDGE_CURVE('',#3802,#3581,#3242,.T.);
#4888=EDGE_CURVE('',#3803,#3579,#3243,.T.);
#4889=EDGE_CURVE('',#3804,#3725,#3244,.T.);
#4890=EDGE_CURVE('',#3560,#3724,#3245,.T.);
#4891=EDGE_CURVE('',#3559,#3787,#3246,.T.);
#4892=EDGE_CURVE('',#3805,#3786,#3247,.T.);
#4893=EDGE_CURVE('',#3806,#3577,#3248,.T.);
#4894=EDGE_CURVE('',#3807,#3575,#3249,.T.);
#4895=EDGE_CURVE('',#3857,#3858,#1051,.T.);
#4896=EDGE_CURVE('',#3857,#3859,#310,.T.);
#4897=EDGE_CURVE('',#3859,#3858,#3250,.T.);
#4898=EDGE_CURVE('',#3860,#3861,#1052,.T.);
#4899=EDGE_CURVE('',#3860,#3857,#311,.T.);
#4900=EDGE_CURVE('',#3858,#3862,#3251,.T.);
#4901=EDGE_CURVE('',#3861,#3862,#312,.F.);
#4902=EDGE_CURVE('',#3863,#3864,#1053,.T.);
#4903=EDGE_CURVE('',#3863,#3860,#313,.T.);
#4904=EDGE_CURVE('',#3864,#3861,#314,.F.);
#4905=EDGE_CURVE('',#3865,#3866,#1054,.T.);
#4906=EDGE_CURVE('',#3865,#3863,#315,.T.);
#4907=EDGE_CURVE('',#3866,#3864,#316,.F.);
#4908=EDGE_CURVE('',#3867,#3868,#1055,.T.);
#4909=EDGE_CURVE('',#3867,#3865,#317,.T.);
#4910=EDGE_CURVE('',#3868,#3866,#318,.F.);
#4911=EDGE_CURVE('',#3869,#3870,#1056,.T.);
#4912=EDGE_CURVE('',#3869,#3867,#319,.T.);
#4913=EDGE_CURVE('',#3870,#3868,#320,.F.);
#4914=EDGE_CURVE('',#3871,#3872,#1057,.T.);
#4915=EDGE_CURVE('',#3871,#3869,#321,.T.);
#4916=EDGE_CURVE('',#3872,#3870,#322,.F.);
#4917=EDGE_CURVE('',#3873,#3874,#1058,.T.);
#4918=EDGE_CURVE('',#3873,#3871,#323,.T.);
#4919=EDGE_CURVE('',#3874,#3872,#324,.F.);
#4920=EDGE_CURVE('',#3875,#3876,#1059,.T.);
#4921=EDGE_CURVE('',#3875,#3873,#325,.T.);
#4922=EDGE_CURVE('',#3876,#3874,#326,.F.);
#4923=EDGE_CURVE('',#3877,#3878,#1060,.T.);
#4924=EDGE_CURVE('',#3877,#3875,#327,.T.);
#4925=EDGE_CURVE('',#3878,#3876,#328,.F.);
#4926=EDGE_CURVE('',#3879,#3880,#1061,.T.);
#4927=EDGE_CURVE('',#3879,#3877,#329,.T.);
#4928=EDGE_CURVE('',#3880,#3878,#330,.F.);
#4929=EDGE_CURVE('',#3881,#3882,#1062,.T.);
#4930=EDGE_CURVE('',#3881,#3879,#331,.T.);
#4931=EDGE_CURVE('',#3882,#3880,#332,.F.);
#4932=EDGE_CURVE('',#3883,#3884,#1063,.T.);
#4933=EDGE_CURVE('',#3883,#3881,#333,.T.);
#4934=EDGE_CURVE('',#3884,#3882,#334,.F.);
#4935=EDGE_CURVE('',#3885,#3886,#1064,.T.);
#4936=EDGE_CURVE('',#3885,#3883,#335,.T.);
#4937=EDGE_CURVE('',#3886,#3884,#336,.F.);
#4938=EDGE_CURVE('',#3887,#3888,#1065,.T.);
#4939=EDGE_CURVE('',#3887,#3885,#337,.T.);
#4940=EDGE_CURVE('',#3888,#3886,#338,.F.);
#4941=EDGE_CURVE('',#3889,#3890,#1066,.T.);
#4942=EDGE_CURVE('',#3889,#3887,#339,.T.);
#4943=EDGE_CURVE('',#3890,#3888,#340,.F.);
#4944=EDGE_CURVE('',#3891,#3892,#1067,.T.);
#4945=EDGE_CURVE('',#3891,#3889,#341,.T.);
#4946=EDGE_CURVE('',#3892,#3890,#342,.F.);
#4947=EDGE_CURVE('',#3893,#3894,#1068,.T.);
#4948=EDGE_CURVE('',#3893,#3891,#343,.T.);
#4949=EDGE_CURVE('',#3894,#3892,#344,.F.);
#4950=EDGE_CURVE('',#3895,#3896,#1069,.T.);
#4951=EDGE_CURVE('',#3895,#3893,#345,.T.);
#4952=EDGE_CURVE('',#3896,#3894,#346,.F.);
#4953=EDGE_CURVE('',#3897,#3898,#1070,.T.);
#4954=EDGE_CURVE('',#3897,#3895,#347,.T.);
#4955=EDGE_CURVE('',#3898,#3896,#348,.F.);
#4956=EDGE_CURVE('',#3899,#3900,#1071,.T.);
#4957=EDGE_CURVE('',#3899,#3897,#349,.T.);
#4958=EDGE_CURVE('',#3900,#3898,#350,.F.);
#4959=EDGE_CURVE('',#3901,#3902,#1072,.T.);
#4960=EDGE_CURVE('',#3901,#3899,#351,.T.);
#4961=EDGE_CURVE('',#3902,#3900,#352,.F.);
#4962=EDGE_CURVE('',#3903,#3904,#1073,.T.);
#4963=EDGE_CURVE('',#3903,#3901,#353,.T.);
#4964=EDGE_CURVE('',#3904,#3902,#354,.F.);
#4965=EDGE_CURVE('',#3905,#3906,#1074,.T.);
#4966=EDGE_CURVE('',#3905,#3903,#355,.T.);
#4967=EDGE_CURVE('',#3906,#3904,#356,.F.);
#4968=EDGE_CURVE('',#3907,#3908,#1075,.T.);
#4969=EDGE_CURVE('',#3907,#3905,#357,.T.);
#4970=EDGE_CURVE('',#3908,#3906,#358,.F.);
#4971=EDGE_CURVE('',#3909,#3910,#1076,.T.);
#4972=EDGE_CURVE('',#3909,#3907,#359,.T.);
#4973=EDGE_CURVE('',#3910,#3908,#360,.F.);
#4974=EDGE_CURVE('',#3911,#3912,#1077,.T.);
#4975=EDGE_CURVE('',#3911,#3909,#361,.T.);
#4976=EDGE_CURVE('',#3912,#3910,#362,.F.);
#4977=EDGE_CURVE('',#3913,#3914,#1078,.T.);
#4978=EDGE_CURVE('',#3913,#3911,#363,.T.);
#4979=EDGE_CURVE('',#3914,#3912,#364,.F.);
#4980=EDGE_CURVE('',#3915,#3916,#1079,.T.);
#4981=EDGE_CURVE('',#3915,#3913,#365,.T.);
#4982=EDGE_CURVE('',#3916,#3914,#366,.F.);
#4983=EDGE_CURVE('',#3917,#3918,#1080,.T.);
#4984=EDGE_CURVE('',#3917,#3915,#367,.T.);
#4985=EDGE_CURVE('',#3918,#3916,#368,.F.);
#4986=EDGE_CURVE('',#3919,#3920,#1081,.T.);
#4987=EDGE_CURVE('',#3919,#3917,#369,.T.);
#4988=EDGE_CURVE('',#3920,#3918,#370,.F.);
#4989=EDGE_CURVE('',#3921,#3922,#1082,.T.);
#4990=EDGE_CURVE('',#3921,#3919,#371,.T.);
#4991=EDGE_CURVE('',#3922,#3920,#372,.F.);
#4992=EDGE_CURVE('',#3923,#3924,#1083,.T.);
#4993=EDGE_CURVE('',#3923,#3921,#373,.T.);
#4994=EDGE_CURVE('',#3924,#3922,#374,.F.);
#4995=EDGE_CURVE('',#3925,#3926,#1084,.T.);
#4996=EDGE_CURVE('',#3925,#3923,#375,.T.);
#4997=EDGE_CURVE('',#3926,#3924,#376,.F.);
#4998=EDGE_CURVE('',#3927,#3928,#1085,.T.);
#4999=EDGE_CURVE('',#3927,#3925,#377,.T.);
#5000=EDGE_CURVE('',#3928,#3926,#378,.F.);
#5001=EDGE_CURVE('',#3929,#3930,#1086,.T.);
#5002=EDGE_CURVE('',#3929,#3927,#379,.T.);
#5003=EDGE_CURVE('',#3930,#3928,#380,.F.);
#5004=EDGE_CURVE('',#3931,#3932,#1087,.T.);
#5005=EDGE_CURVE('',#3931,#3929,#381,.T.);
#5006=EDGE_CURVE('',#3932,#3930,#382,.F.);
#5007=EDGE_CURVE('',#3933,#3934,#1088,.T.);
#5008=EDGE_CURVE('',#3933,#3931,#383,.T.);
#5009=EDGE_CURVE('',#3934,#3932,#384,.F.);
#5010=EDGE_CURVE('',#3935,#3936,#1089,.T.);
#5011=EDGE_CURVE('',#3935,#3933,#385,.T.);
#5012=EDGE_CURVE('',#3936,#3934,#386,.F.);
#5013=EDGE_CURVE('',#3937,#3938,#1090,.T.);
#5014=EDGE_CURVE('',#3937,#3935,#387,.T.);
#5015=EDGE_CURVE('',#3938,#3936,#388,.F.);
#5016=EDGE_CURVE('',#3939,#3940,#1091,.T.);
#5017=EDGE_CURVE('',#3941,#3939,#3252,.T.);
#5018=EDGE_CURVE('',#3941,#3937,#389,.T.);
#5019=EDGE_CURVE('',#3940,#3938,#390,.F.);
#5020=EDGE_CURVE('',#3942,#3941,#3253,.T.);
#5021=EDGE_CURVE('',#3939,#3943,#1092,.T.);
#5022=EDGE_CURVE('',#3943,#3943,#3254,.T.);
#5023=EDGE_CURVE('',#3939,#3942,#3255,.T.);
#5024=EDGE_CURVE('',#3944,#3945,#391,.T.);
#5025=EDGE_CURVE('',#3945,#3946,#1093,.T.);
#5026=EDGE_CURVE('',#3946,#3947,#392,.T.);
#5027=EDGE_CURVE('',#3947,#3944,#1094,.T.);
#5028=EDGE_CURVE('',#3948,#3949,#393,.T.);
#5029=EDGE_CURVE('',#3949,#3950,#1095,.T.);
#5030=EDGE_CURVE('',#3950,#3951,#394,.T.);
#5031=EDGE_CURVE('',#3951,#3948,#1096,.T.);
#5032=EDGE_CURVE('',#3952,#3953,#395,.T.);
#5033=EDGE_CURVE('',#3953,#3954,#1097,.T.);
#5034=EDGE_CURVE('',#3954,#3955,#396,.T.);
#5035=EDGE_CURVE('',#3955,#3952,#1098,.T.);
#5036=EDGE_CURVE('',#3956,#3957,#397,.T.);
#5037=EDGE_CURVE('',#3957,#3958,#1099,.T.);
#5038=EDGE_CURVE('',#3958,#3959,#398,.T.);
#5039=EDGE_CURVE('',#3959,#3956,#1100,.T.);
#5040=EDGE_CURVE('',#3960,#3961,#399,.T.);
#5041=EDGE_CURVE('',#3961,#3962,#1101,.T.);
#5042=EDGE_CURVE('',#3962,#3963,#400,.T.);
#5043=EDGE_CURVE('',#3963,#3960,#1102,.T.);
#5044=EDGE_CURVE('',#3964,#3965,#401,.T.);
#5045=EDGE_CURVE('',#3965,#3966,#1103,.T.);
#5046=EDGE_CURVE('',#3966,#3967,#402,.T.);
#5047=EDGE_CURVE('',#3967,#3964,#1104,.T.);
#5048=EDGE_CURVE('',#3968,#3969,#403,.T.);
#5049=EDGE_CURVE('',#3969,#3970,#1105,.T.);
#5050=EDGE_CURVE('',#3970,#3971,#404,.T.);
#5051=EDGE_CURVE('',#3971,#3968,#1106,.T.);
#5052=EDGE_CURVE('',#3972,#3973,#405,.T.);
#5053=EDGE_CURVE('',#3973,#3974,#1107,.T.);
#5054=EDGE_CURVE('',#3974,#3975,#406,.T.);
#5055=EDGE_CURVE('',#3975,#3972,#1108,.T.);
#5056=EDGE_CURVE('',#3976,#3977,#407,.T.);
#5057=EDGE_CURVE('',#3977,#3978,#1109,.T.);
#5058=EDGE_CURVE('',#3978,#3979,#408,.T.);
#5059=EDGE_CURVE('',#3979,#3976,#1110,.T.);
#5060=EDGE_CURVE('',#3980,#3981,#409,.T.);
#5061=EDGE_CURVE('',#3981,#3982,#1111,.T.);
#5062=EDGE_CURVE('',#3982,#3983,#410,.T.);
#5063=EDGE_CURVE('',#3983,#3980,#1112,.T.);
#5064=EDGE_CURVE('',#3984,#3984,#3256,.T.);
#5065=EDGE_CURVE('',#3984,#3985,#3257,.T.);
#5066=EDGE_CURVE('',#3986,#3985,#3258,.T.);
#5067=EDGE_CURVE('',#3987,#3986,#411,.T.);
#5068=EDGE_CURVE('',#3988,#3987,#3259,.T.);
#5069=EDGE_CURVE('',#3989,#3988,#412,.T.);
#5070=EDGE_CURVE('',#3990,#3989,#3260,.T.);
#5071=EDGE_CURVE('',#3991,#3990,#413,.T.);
#5072=EDGE_CURVE('',#3992,#3991,#3261,.T.);
#5073=EDGE_CURVE('',#3993,#3992,#414,.T.);
#5074=EDGE_CURVE('',#3994,#3993,#3262,.T.);
#5075=EDGE_CURVE('',#3995,#3994,#415,.T.);
#5076=EDGE_CURVE('',#3996,#3995,#3263,.T.);
#5077=EDGE_CURVE('',#3997,#3996,#416,.T.);
#5078=EDGE_CURVE('',#3998,#3997,#3264,.T.);
#5079=EDGE_CURVE('',#3999,#3998,#417,.T.);
#5080=EDGE_CURVE('',#4000,#3999,#3265,.T.);
#5081=EDGE_CURVE('',#4001,#4000,#418,.T.);
#5082=EDGE_CURVE('',#3945,#4001,#3266,.T.);
#5083=EDGE_CURVE('',#3949,#3944,#3267,.T.);
#5084=EDGE_CURVE('',#3953,#3948,#3268,.T.);
#5085=EDGE_CURVE('',#3957,#3952,#3269,.T.);
#5086=EDGE_CURVE('',#3961,#3956,#3270,.T.);
#5087=EDGE_CURVE('',#3965,#3960,#3271,.T.);
#5088=EDGE_CURVE('',#3969,#3964,#3272,.T.);
#5089=EDGE_CURVE('',#3973,#3968,#3273,.T.);
#5090=EDGE_CURVE('',#3977,#3972,#3274,.T.);
#5091=EDGE_CURVE('',#3981,#3976,#3275,.T.);
#5092=EDGE_CURVE('',#4002,#3980,#3276,.T.);
#5093=EDGE_CURVE('',#4003,#4002,#419,.T.);
#5094=EDGE_CURVE('',#4004,#4003,#3277,.T.);
#5095=EDGE_CURVE('',#4005,#4004,#420,.T.);
#5096=EDGE_CURVE('',#4006,#4005,#3278,.T.);
#5097=EDGE_CURVE('',#4007,#4006,#421,.T.);
#5098=EDGE_CURVE('',#4008,#4007,#3279,.T.);
#5099=EDGE_CURVE('',#4009,#4008,#422,.T.);
#5100=EDGE_CURVE('',#4010,#4009,#3280,.T.);
#5101=EDGE_CURVE('',#4011,#4010,#423,.T.);
#5102=EDGE_CURVE('',#4012,#4011,#3281,.T.);
#5103=EDGE_CURVE('',#4013,#4012,#424,.T.);
#5104=EDGE_CURVE('',#4014,#4013,#3282,.T.);
#5105=EDGE_CURVE('',#4015,#4014,#425,.T.);
#5106=EDGE_CURVE('',#4016,#4015,#3283,.T.);
#5107=EDGE_CURVE('',#4017,#4016,#426,.T.);
#5108=EDGE_CURVE('',#3985,#4017,#3284,.T.);
#5109=EDGE_CURVE('',#4018,#4018,#3285,.T.);
#5110=EDGE_CURVE('',#4018,#4019,#3286,.T.);
#5111=EDGE_CURVE('',#3963,#4019,#3287,.T.);
#5112=EDGE_CURVE('',#3959,#3962,#3288,.T.);
#5113=EDGE_CURVE('',#3955,#3958,#3289,.T.);
#5114=EDGE_CURVE('',#3951,#3954,#3290,.T.);
#5115=EDGE_CURVE('',#3947,#3950,#3291,.T.);
#5116=EDGE_CURVE('',#4020,#3946,#3292,.T.);
#5117=EDGE_CURVE('',#4021,#4020,#427,.T.);
#5118=EDGE_CURVE('',#4022,#4021,#3293,.T.);
#5119=EDGE_CURVE('',#4023,#4022,#428,.T.);
#5120=EDGE_CURVE('',#4024,#4023,#3294,.T.);
#5121=EDGE_CURVE('',#4025,#4024,#429,.T.);
#5122=EDGE_CURVE('',#4026,#4025,#3295,.T.);
#5123=EDGE_CURVE('',#4027,#4026,#430,.T.);
#5124=EDGE_CURVE('',#4028,#4027,#3296,.T.);
#5125=EDGE_CURVE('',#4029,#4028,#431,.T.);
#5126=EDGE_CURVE('',#4030,#4029,#3297,.T.);
#5127=EDGE_CURVE('',#4031,#4030,#432,.T.);
#5128=EDGE_CURVE('',#4032,#4031,#3298,.T.);
#5129=EDGE_CURVE('',#4033,#4032,#433,.T.);
#5130=EDGE_CURVE('',#4034,#4033,#3299,.T.);
#5131=EDGE_CURVE('',#4035,#4034,#434,.T.);
#5132=EDGE_CURVE('',#4036,#4035,#3300,.T.);
#5133=EDGE_CURVE('',#4037,#4036,#435,.T.);
#5134=EDGE_CURVE('',#4038,#4037,#3301,.T.);
#5135=EDGE_CURVE('',#4039,#4038,#436,.T.);
#5136=EDGE_CURVE('',#4040,#4039,#3302,.T.);
#5137=EDGE_CURVE('',#4041,#4040,#437,.T.);
#5138=EDGE_CURVE('',#4042,#4041,#3303,.T.);
#5139=EDGE_CURVE('',#4043,#4042,#438,.T.);
#5140=EDGE_CURVE('',#4044,#4043,#3304,.T.);
#5141=EDGE_CURVE('',#4045,#4044,#439,.T.);
#5142=EDGE_CURVE('',#4046,#4045,#3305,.T.);
#5143=EDGE_CURVE('',#4047,#4046,#440,.T.);
#5144=EDGE_CURVE('',#4048,#4047,#3306,.T.);
#5145=EDGE_CURVE('',#4049,#4048,#441,.T.);
#5146=EDGE_CURVE('',#4050,#4049,#3307,.T.);
#5147=EDGE_CURVE('',#4051,#4050,#442,.T.);
#5148=EDGE_CURVE('',#3983,#4051,#3308,.T.);
#5149=EDGE_CURVE('',#3979,#3982,#3309,.T.);
#5150=EDGE_CURVE('',#3975,#3978,#3310,.T.);
#5151=EDGE_CURVE('',#3971,#3974,#3311,.T.);
#5152=EDGE_CURVE('',#3967,#3970,#3312,.T.);
#5153=EDGE_CURVE('',#4019,#3966,#3313,.T.);
#5154=EDGE_CURVE('',#3942,#3940,#443,.F.);
#5155=EDGE_CURVE('',#4020,#4001,#1113,.T.);
#5156=EDGE_CURVE('',#4002,#4051,#1114,.T.);
#5157=EDGE_CURVE('',#4050,#4003,#1115,.T.);
#5158=EDGE_CURVE('',#4004,#4049,#1116,.T.);
#5159=EDGE_CURVE('',#4048,#4005,#1117,.T.);
#5160=EDGE_CURVE('',#4006,#4047,#1118,.T.);
#5161=EDGE_CURVE('',#4046,#4007,#1119,.T.);
#5162=EDGE_CURVE('',#4008,#4045,#1120,.T.);
#5163=EDGE_CURVE('',#4044,#4009,#1121,.T.);
#5164=EDGE_CURVE('',#4010,#4043,#1122,.T.);
#5165=EDGE_CURVE('',#4042,#4011,#1123,.T.);
#5166=EDGE_CURVE('',#4012,#4041,#1124,.T.);
#5167=EDGE_CURVE('',#4040,#4013,#1125,.T.);
#5168=EDGE_CURVE('',#4014,#4039,#1126,.T.);
#5169=EDGE_CURVE('',#4038,#4015,#1127,.T.);
#5170=EDGE_CURVE('',#4016,#4037,#1128,.T.);
#5171=EDGE_CURVE('',#4036,#4017,#1129,.T.);
#5172=EDGE_CURVE('',#3986,#4035,#1130,.T.);
#5173=EDGE_CURVE('',#4034,#3987,#1131,.T.);
#5174=EDGE_CURVE('',#3988,#4033,#1132,.T.);
#5175=EDGE_CURVE('',#4032,#3989,#1133,.T.);
#5176=EDGE_CURVE('',#3990,#4031,#1134,.T.);
#5177=EDGE_CURVE('',#4030,#3991,#1135,.T.);
#5178=EDGE_CURVE('',#3992,#4029,#1136,.T.);
#5179=EDGE_CURVE('',#4028,#3993,#1137,.T.);
#5180=EDGE_CURVE('',#3994,#4027,#1138,.T.);
#5181=EDGE_CURVE('',#4026,#3995,#1139,.T.);
#5182=EDGE_CURVE('',#3996,#4025,#1140,.T.);
#5183=EDGE_CURVE('',#4024,#3997,#1141,.T.);
#5184=EDGE_CURVE('',#3998,#4023,#1142,.T.);
#5185=EDGE_CURVE('',#4052,#4053,#444,.T.);
#5186=EDGE_CURVE('',#4053,#3862,#445,.T.);
#5187=EDGE_CURVE('',#3859,#4052,#446,.T.);
#5188=EDGE_CURVE('',#4000,#4021,#1143,.T.);
#5189=EDGE_CURVE('',#4022,#3999,#1144,.T.);
#5190=EDGE_CURVE('',#3941,#4054,#447,.T.);
#5191=EDGE_CURVE('',#4055,#3942,#448,.T.);
#5192=EDGE_CURVE('',#4054,#4055,#449,.T.);
#5193=EDGE_CURVE('',#4055,#4053,#88,.T.);
#5194=EDGE_CURVE('',#4054,#4052,#89,.T.);
#5195=EDGE_CURVE('',#4056,#4057,#450,.T.);
#5196=EDGE_CURVE('',#4057,#4056,#451,.T.);
#5197=EDGE_CURVE('',#4058,#4058,#452,.T.);
#5198=EDGE_CURVE('',#4058,#4057,#1145,.T.);
#5199=EDGE_CURVE('',#4059,#4060,#3314,.T.);
#5200=EDGE_CURVE('',#4061,#4059,#3315,.T.);
#5201=EDGE_CURVE('',#4062,#4061,#3316,.T.);
#5202=EDGE_CURVE('',#4062,#4060,#3317,.T.);
#5203=EDGE_CURVE('',#4063,#4064,#3318,.T.);
#5204=EDGE_CURVE('',#4065,#4063,#3319,.T.);
#5205=EDGE_CURVE('',#4066,#4065,#3320,.T.);
#5206=EDGE_CURVE('',#4066,#4064,#3321,.T.);
#5207=EDGE_CURVE('',#4067,#4067,#3322,.T.);
#5208=EDGE_CURVE('',#4067,#4068,#1146,.T.);
#5209=EDGE_CURVE('',#4068,#4068,#3323,.T.);
#5210=EDGE_CURVE('',#4069,#4069,#3324,.T.);
#5211=EDGE_CURVE('',#4069,#4070,#1147,.T.);
#5212=EDGE_CURVE('',#4070,#4070,#3325,.T.);
#5213=EDGE_CURVE('',#4071,#4071,#3326,.T.);
#5214=EDGE_CURVE('',#4071,#4072,#1148,.T.);
#5215=EDGE_CURVE('',#4072,#4072,#3327,.T.);
#5216=EDGE_CURVE('',#4073,#4074,#3328,.T.);
#5217=EDGE_CURVE('',#4073,#4075,#3329,.T.);
#5218=EDGE_CURVE('',#4076,#4075,#3330,.T.);
#5219=EDGE_CURVE('',#4076,#4074,#453,.T.);
#5220=EDGE_CURVE('',#4077,#4078,#3331,.T.);
#5221=EDGE_CURVE('',#4077,#4079,#3332,.T.);
#5222=EDGE_CURVE('',#4080,#4079,#3333,.T.);
#5223=EDGE_CURVE('',#4080,#4078,#454,.T.);
#5224=EDGE_CURVE('',#4081,#4082,#3334,.T.);
#5225=EDGE_CURVE('',#4081,#4083,#1149,.T.);
#5226=EDGE_CURVE('',#4083,#4084,#3335,.T.);
#5227=EDGE_CURVE('',#4082,#4084,#1150,.T.);
#5228=EDGE_CURVE('',#4061,#4063,#1151,.T.);
#5229=EDGE_CURVE('',#4062,#4064,#1152,.T.);
#5230=EDGE_CURVE('',#4085,#4086,#3336,.T.);
#5231=EDGE_CURVE('',#4086,#4087,#1153,.T.);
#5232=EDGE_CURVE('',#4088,#4087,#3337,.T.);
#5233=EDGE_CURVE('',#4088,#4085,#1154,.T.);
#5234=EDGE_CURVE('',#4089,#4090,#3338,.T.);
#5235=EDGE_CURVE('',#4089,#4091,#3339,.T.);
#5236=EDGE_CURVE('',#4091,#4092,#455,.T.);
#5237=EDGE_CURVE('',#4092,#4093,#3340,.T.);
#5238=EDGE_CURVE('',#4093,#4094,#1155,.T.);
#5239=EDGE_CURVE('',#4094,#4095,#3341,.T.);
#5240=EDGE_CURVE('',#4095,#4096,#456,.T.);
#5241=EDGE_CURVE('',#4096,#4097,#3342,.T.);
#5242=EDGE_CURVE('',#4097,#4098,#3343,.T.);
#5243=EDGE_CURVE('',#4098,#4090,#1156,.T.);
#5244=EDGE_CURVE('',#4099,#4100,#3344,.T.);
#5245=EDGE_CURVE('',#4100,#4101,#1157,.T.);
#5246=EDGE_CURVE('',#4102,#4101,#3345,.T.);
#5247=EDGE_CURVE('',#4102,#4099,#1158,.T.);
#5248=EDGE_CURVE('',#4103,#4104,#1159,.T.);
#5249=EDGE_CURVE('',#4103,#4105,#3346,.T.);
#5250=EDGE_CURVE('',#4106,#4105,#1160,.T.);
#5251=EDGE_CURVE('',#4104,#4106,#3347,.T.);
#5252=EDGE_CURVE('',#4107,#4108,#3348,.T.);
#5253=EDGE_CURVE('',#4108,#4109,#3349,.T.);
#5254=EDGE_CURVE('',#4109,#4110,#3350,.T.);
#5255=EDGE_CURVE('',#4110,#4077,#3351,.T.);
#5256=EDGE_CURVE('',#4078,#4111,#3352,.T.);
#5257=EDGE_CURVE('',#4111,#4059,#3353,.T.);
#5258=EDGE_CURVE('',#4060,#4112,#1161,.T.);
#5259=EDGE_CURVE('',#4112,#4113,#3354,.T.);
#5260=EDGE_CURVE('',#4113,#4114,#3355,.T.);
#5261=EDGE_CURVE('',#4114,#4107,#3356,.T.);
#5262=EDGE_CURVE('',#4115,#4116,#3357,.T.);
#5263=EDGE_CURVE('',#4116,#4117,#3358,.T.);
#5264=EDGE_CURVE('',#4117,#4118,#3359,.T.);
#5265=EDGE_CURVE('',#4118,#4119,#3360,.T.);
#5266=EDGE_CURVE('',#4119,#4066,#1162,.T.);
#5267=EDGE_CURVE('',#4065,#4120,#3361,.T.);
#5268=EDGE_CURVE('',#4120,#4076,#3362,.T.);
#5269=EDGE_CURVE('',#4075,#4121,#3363,.T.);
#5270=EDGE_CURVE('',#4121,#4122,#3364,.T.);
#5271=EDGE_CURVE('',#4122,#4115,#3365,.T.);
#5272=EDGE_CURVE('',#4064,#4103,#1163,.T.);
#5273=EDGE_CURVE('',#4104,#4123,#1164,.T.);
#5274=EDGE_CURVE('',#4124,#4123,#1165,.T.);
#5275=EDGE_CURVE('',#4125,#4124,#1166,.T.);
#5276=EDGE_CURVE('',#4125,#4126,#1167,.T.);
#5277=EDGE_CURVE('',#4126,#4062,#1168,.T.);
#5278=EDGE_CURVE('',#4105,#4127,#3366,.T.);
#5279=EDGE_CURVE('',#4127,#4128,#1169,.T.);
#5280=EDGE_CURVE('',#4128,#4129,#3367,.T.);
#5281=EDGE_CURVE('',#4129,#4130,#1170,.T.);
#5282=EDGE_CURVE('',#4130,#4131,#3368,.T.);
#5283=EDGE_CURVE('',#4132,#4131,#1171,.T.);
#5284=EDGE_CURVE('',#4106,#4132,#3369,.T.);
#5285=EDGE_CURVE('',#4133,#4134,#1172,.T.);
#5286=EDGE_CURVE('',#4133,#4135,#3370,.T.);
#5287=EDGE_CURVE('',#4135,#4136,#1173,.T.);
#5288=EDGE_CURVE('',#4136,#4134,#3371,.T.);
#5289=EDGE_CURVE('',#4093,#4133,#3372,.T.);
#5290=EDGE_CURVE('',#4134,#4094,#3373,.T.);
#5291=EDGE_CURVE('',#4084,#4137,#1174,.T.);
#5292=EDGE_CURVE('',#4138,#4137,#1175,.T.);
#5293=EDGE_CURVE('',#4082,#4138,#1176,.T.);
#5294=EDGE_CURVE('',#4137,#4139,#111,.T.);
#5295=EDGE_CURVE('',#4139,#4140,#457,.T.);
#5296=EDGE_CURVE('',#4140,#4141,#458,.T.);
#5297=EDGE_CURVE('',#4141,#4142,#3374,.T.);
#5298=EDGE_CURVE('',#4143,#4142,#1177,.T.);
#5299=EDGE_CURVE('',#4143,#4144,#3375,.T.);
#5300=EDGE_CURVE('',#4144,#4145,#459,.T.);
#5301=EDGE_CURVE('',#4145,#4146,#460,.T.);
#5302=EDGE_CURVE('',#4138,#4146,#112,.T.);
#5303=EDGE_CURVE('',#4061,#4143,#3376,.T.);
#5304=EDGE_CURVE('',#4142,#4063,#3377,.T.);
#5305=EDGE_CURVE('',#4097,#4147,#461,.T.);
#5306=EDGE_CURVE('',#4147,#4148,#3378,.T.);
#5307=EDGE_CURVE('',#4149,#4148,#3379,.T.);
#5308=EDGE_CURVE('',#4150,#4149,#3380,.T.);
#5309=EDGE_CURVE('',#4150,#4151,#462,.T.);
#5310=EDGE_CURVE('',#4137,#4151,#1178,.T.);
#5311=EDGE_CURVE('',#4083,#4152,#1179,.T.);
#5312=EDGE_CURVE('',#4152,#4153,#1180,.T.);
#5313=EDGE_CURVE('',#4153,#4154,#1181,.T.);
#5314=EDGE_CURVE('',#4154,#4155,#1182,.T.);
#5315=EDGE_CURVE('',#4155,#4156,#1183,.T.);
#5316=EDGE_CURVE('',#4156,#4157,#1184,.T.);
#5317=EDGE_CURVE('',#4157,#4158,#1185,.T.);
#5318=EDGE_CURVE('',#4158,#4159,#1186,.T.);
#5319=EDGE_CURVE('',#4159,#4160,#1187,.T.);
#5320=EDGE_CURVE('',#4160,#4161,#1188,.T.);
#5321=EDGE_CURVE('',#4161,#4162,#1189,.T.);
#5322=EDGE_CURVE('',#4162,#4163,#1190,.T.);
#5323=EDGE_CURVE('',#4163,#4164,#1191,.T.);
#5324=EDGE_CURVE('',#4164,#4100,#1192,.T.);
#5325=EDGE_CURVE('',#4099,#4165,#1193,.T.);
#5326=EDGE_CURVE('',#4165,#4086,#1194,.T.);
#5327=EDGE_CURVE('',#4085,#4166,#1195,.T.);
#5328=EDGE_CURVE('',#4166,#4098,#1196,.T.);
#5329=EDGE_CURVE('',#4167,#4148,#1197,.T.);
#5330=EDGE_CURVE('',#4167,#4073,#3381,.T.);
#5331=EDGE_CURVE('',#4073,#4149,#1198,.T.);
#5332=EDGE_CURVE('',#4074,#4150,#463,.T.);
#5333=EDGE_CURVE('',#4151,#4139,#464,.T.);
#5334=EDGE_CURVE('',#4147,#4168,#3382,.T.);
#5335=EDGE_CURVE('',#4168,#4167,#3383,.T.);
#5336=EDGE_CURVE('',#4169,#4170,#3384,.T.);
#5337=EDGE_CURVE('',#4170,#4171,#3385,.T.);
#5338=EDGE_CURVE('',#4171,#4172,#3386,.T.);
#5339=EDGE_CURVE('',#4172,#4169,#1199,.T.);
#5340=EDGE_CURVE('',#4146,#4173,#465,.T.);
#5341=EDGE_CURVE('',#4138,#4173,#1200,.T.);
#5342=EDGE_CURVE('',#4174,#4175,#3387,.T.);
#5343=EDGE_CURVE('',#4174,#4080,#466,.T.);
#5344=EDGE_CURVE('',#4175,#4079,#1201,.T.);
#5345=EDGE_CURVE('',#4079,#4169,#3388,.T.);
#5346=EDGE_CURVE('',#4175,#4172,#3389,.T.);
#5347=EDGE_CURVE('',#4171,#4089,#467,.T.);
#5348=EDGE_CURVE('',#4176,#4090,#1202,.T.);
#5349=EDGE_CURVE('',#4088,#4176,#1203,.T.);
#5350=EDGE_CURVE('',#4177,#4087,#1204,.T.);
#5351=EDGE_CURVE('',#4102,#4177,#1205,.T.);
#5352=EDGE_CURVE('',#4178,#4101,#1206,.T.);
#5353=EDGE_CURVE('',#4179,#4178,#1207,.T.);
#5354=EDGE_CURVE('',#4180,#4179,#1208,.T.);
#5355=EDGE_CURVE('',#4181,#4180,#1209,.T.);
#5356=EDGE_CURVE('',#4182,#4181,#1210,.T.);
#5357=EDGE_CURVE('',#4183,#4182,#1211,.T.);
#5358=EDGE_CURVE('',#4184,#4183,#1212,.T.);
#5359=EDGE_CURVE('',#4185,#4184,#1213,.T.);
#5360=EDGE_CURVE('',#4186,#4185,#1214,.T.);
#5361=EDGE_CURVE('',#4187,#4186,#1215,.T.);
#5362=EDGE_CURVE('',#4188,#4187,#1216,.T.);
#5363=EDGE_CURVE('',#4189,#4188,#1217,.T.);
#5364=EDGE_CURVE('',#4190,#4189,#1218,.T.);
#5365=EDGE_CURVE('',#4081,#4190,#1219,.T.);
#5366=EDGE_CURVE('',#4173,#4174,#468,.T.);
#5367=EDGE_CURVE('',#4109,#4170,#469,.T.);
#5368=EDGE_CURVE('',#4110,#4169,#3390,.T.);
#5369=EDGE_CURVE('',#4168,#4122,#470,.T.);
#5370=EDGE_CURVE('',#4167,#4121,#3391,.T.);
#5371=EDGE_CURVE('',#4129,#4126,#3392,.T.);
#5372=EDGE_CURVE('',#4125,#4130,#3393,.T.);
#5373=EDGE_CURVE('',#4191,#4132,#1220,.T.);
#5374=EDGE_CURVE('',#4192,#4131,#1221,.T.);
#5375=EDGE_CURVE('',#4192,#4191,#1222,.T.);
#5376=EDGE_CURVE('',#4124,#4193,#1223,.T.);
#5377=EDGE_CURVE('',#4193,#4192,#3394,.T.);
#5378=EDGE_CURVE('',#4194,#4191,#3395,.T.);
#5379=EDGE_CURVE('',#4123,#4194,#1224,.T.);
#5380=EDGE_CURVE('',#4193,#4194,#1225,.T.);
#5381=EDGE_CURVE('',#4189,#4153,#1226,.T.);
#5382=EDGE_CURVE('',#4152,#4190,#1227,.T.);
#5383=EDGE_CURVE('',#4154,#4188,#1228,.T.);
#5384=EDGE_CURVE('',#4156,#4186,#1229,.T.);
#5385=EDGE_CURVE('',#4187,#4155,#1230,.T.);
#5386=EDGE_CURVE('',#4158,#4184,#1231,.T.);
#5387=EDGE_CURVE('',#4185,#4157,#1232,.T.);
#5388=EDGE_CURVE('',#4160,#4182,#1233,.T.);
#5389=EDGE_CURVE('',#4183,#4159,#1234,.T.);
#5390=EDGE_CURVE('',#4162,#4180,#1235,.T.);
#5391=EDGE_CURVE('',#4181,#4161,#1236,.T.);
#5392=EDGE_CURVE('',#4164,#4178,#1237,.T.);
#5393=EDGE_CURVE('',#4179,#4163,#1238,.T.);
#5394=EDGE_CURVE('',#4166,#4176,#1239,.T.);
#5395=EDGE_CURVE('',#4165,#4177,#1240,.T.);
#5396=EDGE_CURVE('',#4117,#4127,#3396,.T.);
#5397=EDGE_CURVE('',#4118,#4105,#3397,.T.);
#5398=EDGE_CURVE('',#4119,#4103,#3398,.T.);
#5399=EDGE_CURVE('',#4120,#4142,#3399,.T.);
#5400=EDGE_CURVE('',#4076,#4141,#3400,.T.);
#5401=EDGE_CURVE('',#4074,#4140,#3401,.T.);
#5402=EDGE_CURVE('',#4128,#4114,#3402,.T.);
#5403=EDGE_CURVE('',#4129,#4113,#3403,.T.);
#5404=EDGE_CURVE('',#4126,#4112,#3404,.T.);
#5405=EDGE_CURVE('',#4143,#4111,#3405,.T.);
#5406=EDGE_CURVE('',#4144,#4078,#3406,.T.);
#5407=EDGE_CURVE('',#4145,#4080,#3407,.T.);
#5408=EDGE_CURVE('',#4168,#4096,#3408,.T.);
#5409=EDGE_CURVE('',#4122,#4095,#3409,.T.);
#5410=EDGE_CURVE('',#4115,#4094,#3410,.T.);
#5411=EDGE_CURVE('',#4116,#4134,#3411,.T.);
#5412=EDGE_CURVE('',#4117,#4136,#3412,.T.);
#5413=EDGE_CURVE('',#4127,#4136,#3413,.T.);
#5414=EDGE_CURVE('',#4128,#4135,#3414,.T.);
#5415=EDGE_CURVE('',#4114,#4135,#3415,.T.);
#5416=EDGE_CURVE('',#4107,#4133,#3416,.T.);
#5417=EDGE_CURVE('',#4108,#4093,#3417,.T.);
#5418=EDGE_CURVE('',#4109,#4092,#3418,.T.);
#5419=EDGE_CURVE('',#4170,#4091,#3419,.T.);
#5420=EDGE_CURVE('',#4195,#4196,#3420,.T.);
#5421=EDGE_CURVE('',#4197,#4195,#471,.T.);
#5422=EDGE_CURVE('',#4198,#4197,#3421,.T.);
#5423=EDGE_CURVE('',#4199,#4198,#472,.T.);
#5424=EDGE_CURVE('',#4196,#4199,#473,.T.);
#5425=EDGE_CURVE('',#4200,#4201,#3422,.T.);
#5426=EDGE_CURVE('',#4202,#4200,#474,.T.);
#5427=EDGE_CURVE('',#4203,#4202,#3423,.T.);
#5428=EDGE_CURVE('',#4204,#4203,#475,.T.);
#5429=EDGE_CURVE('',#4201,#4204,#476,.T.);
#5430=EDGE_CURVE('',#4205,#4206,#3424,.T.);
#5431=EDGE_CURVE('',#4207,#4205,#477,.T.);
#5432=EDGE_CURVE('',#4208,#4207,#3425,.T.);
#5433=EDGE_CURVE('',#4206,#4208,#478,.T.);
#5434=EDGE_CURVE('',#4209,#4210,#3426,.T.);
#5435=EDGE_CURVE('',#4211,#4209,#479,.T.);
#5436=EDGE_CURVE('',#4212,#4211,#3427,.T.);
#5437=EDGE_CURVE('',#4210,#4212,#480,.T.);
#5438=EDGE_CURVE('',#4213,#4214,#3428,.T.);
#5439=EDGE_CURVE('',#4215,#4214,#1241,.T.);
#5440=EDGE_CURVE('',#4216,#4215,#3429,.T.);
#5441=EDGE_CURVE('',#4213,#4216,#1242,.T.);
#5442=EDGE_CURVE('',#4217,#4217,#3430,.T.);
#5443=EDGE_CURVE('',#4217,#4218,#1243,.T.);
#5444=EDGE_CURVE('',#4218,#4218,#3431,.T.);
#5445=EDGE_CURVE('',#4219,#4219,#3432,.T.);
#5446=EDGE_CURVE('',#4219,#4220,#1244,.T.);
#5447=EDGE_CURVE('',#4220,#4220,#3433,.T.);
#5448=EDGE_CURVE('',#4221,#4221,#3434,.T.);
#5449=EDGE_CURVE('',#4221,#4222,#1245,.T.);
#5450=EDGE_CURVE('',#4222,#4222,#3435,.T.);
#5451=EDGE_CURVE('',#4196,#4223,#1246,.T.);
#5452=EDGE_CURVE('',#4223,#4224,#3436,.T.);
#5453=EDGE_CURVE('',#4195,#4224,#1247,.T.);
#5454=EDGE_CURVE('',#4225,#4225,#3437,.T.);
#5455=EDGE_CURVE('',#4225,#4226,#1248,.T.);
#5456=EDGE_CURVE('',#4226,#4226,#3438,.T.);
#5457=EDGE_CURVE('',#4227,#4227,#3439,.T.);
#5458=EDGE_CURVE('',#4227,#4228,#1249,.T.);
#5459=EDGE_CURVE('',#4228,#4228,#3440,.T.);
#5460=EDGE_CURVE('',#4229,#4229,#3441,.T.);
#5461=EDGE_CURVE('',#4229,#4230,#1250,.T.);
#5462=EDGE_CURVE('',#4230,#4230,#3442,.T.);
#5463=EDGE_CURVE('',#4231,#4232,#3443,.T.);
#5464=EDGE_CURVE('',#4231,#4203,#1251,.T.);
#5465=EDGE_CURVE('',#4232,#4202,#1252,.T.);
#5466=EDGE_CURVE('',#4207,#4209,#1253,.T.);
#5467=EDGE_CURVE('',#4208,#4210,#1254,.T.);
#5468=EDGE_CURVE('',#4233,#4204,#1255,.T.);
#5469=EDGE_CURVE('',#4233,#4231,#1256,.T.);
#5470=EDGE_CURVE('',#4199,#4234,#1257,.T.);
#5471=EDGE_CURVE('',#4234,#4223,#1258,.T.);
#5472=EDGE_CURVE('',#4202,#4235,#1259,.T.);
#5473=EDGE_CURVE('',#4236,#4235,#1260,.T.);
#5474=EDGE_CURVE('',#4232,#4236,#1261,.T.);
#5475=EDGE_CURVE('',#4237,#4238,#1262,.T.);
#5476=EDGE_CURVE('',#4238,#4239,#1263,.T.);
#5477=EDGE_CURVE('',#4240,#4239,#1264,.T.);
#5478=EDGE_CURVE('',#4241,#4240,#1265,.T.);
#5479=EDGE_CURVE('',#4236,#4241,#1266,.T.);
#5480=EDGE_CURVE('',#4235,#4237,#113,.T.);
#5481=EDGE_CURVE('',#4206,#4198,#3444,.T.);
#5482=EDGE_CURVE('',#4197,#4242,#1267,.T.);
#5483=EDGE_CURVE('',#4242,#4243,#1268,.T.);
#5484=EDGE_CURVE('',#4243,#4244,#1269,.T.);
#5485=EDGE_CURVE('',#4244,#4245,#1270,.T.);
#5486=EDGE_CURVE('',#4245,#4246,#1271,.T.);
#5487=EDGE_CURVE('',#4246,#4247,#3445,.T.);
#5488=EDGE_CURVE('',#4247,#4205,#1272,.T.);
#5489=EDGE_CURVE('',#4212,#4201,#3446,.T.);
#5490=EDGE_CURVE('',#4211,#4248,#1273,.T.);
#5491=EDGE_CURVE('',#4248,#4249,#3447,.T.);
#5492=EDGE_CURVE('',#4249,#4250,#1274,.T.);
#5493=EDGE_CURVE('',#4250,#4251,#1275,.T.);
#5494=EDGE_CURVE('',#4252,#4251,#1276,.T.);
#5495=EDGE_CURVE('',#4252,#4253,#1277,.T.);
#5496=EDGE_CURVE('',#4253,#4200,#1278,.T.);
#5497=EDGE_CURVE('',#4254,#4255,#1279,.T.);
#5498=EDGE_CURVE('',#4255,#4256,#1280,.T.);
#5499=EDGE_CURVE('',#4257,#4256,#1281,.T.);
#5500=EDGE_CURVE('',#4257,#4254,#1282,.T.);
#5501=EDGE_CURVE('',#4256,#4258,#3448,.T.);
#5502=EDGE_CURVE('',#4259,#4258,#1283,.T.);
#5503=EDGE_CURVE('',#4259,#4257,#3449,.T.);
#5504=EDGE_CURVE('',#4258,#4209,#1284,.T.);
#5505=EDGE_CURVE('',#4207,#4259,#1285,.T.);
#5506=EDGE_CURVE('',#4260,#4261,#1286,.T.);
#5507=EDGE_CURVE('',#4260,#4195,#1287,.T.);
#5508=EDGE_CURVE('',#4224,#4261,#1288,.T.);
#5509=EDGE_CURVE('',#4262,#4263,#1289,.T.);
#5510=EDGE_CURVE('',#4263,#4264,#1290,.T.);
#5511=EDGE_CURVE('',#4264,#4265,#1291,.T.);
#5512=EDGE_CURVE('',#4265,#4260,#114,.T.);
#5513=EDGE_CURVE('',#4261,#4266,#1292,.T.);
#5514=EDGE_CURVE('',#4262,#4266,#1293,.T.);
#5515=EDGE_CURVE('',#4267,#4268,#1294,.T.);
#5516=EDGE_CURVE('',#4268,#4252,#115,.T.);
#5517=EDGE_CURVE('',#4251,#4267,#116,.T.);
#5518=EDGE_CURVE('',#4269,#4270,#1295,.T.);
#5519=EDGE_CURVE('',#4270,#4271,#1296,.T.);
#5520=EDGE_CURVE('',#4271,#4272,#3450,.T.);
#5521=EDGE_CURVE('',#4272,#4269,#1297,.T.);
#5522=EDGE_CURVE('',#4273,#4274,#3451,.T.);
#5523=EDGE_CURVE('',#4274,#4268,#1298,.T.);
#5524=EDGE_CURVE('',#4267,#4273,#1299,.T.);
#5525=EDGE_CURVE('',#4243,#4270,#117,.T.);
#5526=EDGE_CURVE('',#4269,#4244,#118,.T.);
#5527=EDGE_CURVE('',#4275,#4276,#1300,.T.);
#5528=EDGE_CURVE('',#4276,#4277,#1301,.T.);
#5529=EDGE_CURVE('',#4277,#4278,#1302,.T.);
#5530=EDGE_CURVE('',#4278,#4255,#119,.T.);
#5531=EDGE_CURVE('',#4254,#4275,#120,.T.);
#5532=EDGE_CURVE('',#4214,#4234,#3452,.T.);
#5533=EDGE_CURVE('',#4279,#4213,#1303,.T.);
#5534=EDGE_CURVE('',#4280,#4279,#3453,.T.);
#5535=EDGE_CURVE('',#4281,#4280,#1304,.T.);
#5536=EDGE_CURVE('',#4266,#4281,#1305,.T.);
#5537=EDGE_CURVE('',#4215,#4233,#3454,.T.);
#5538=EDGE_CURVE('',#4241,#4282,#1306,.T.);
#5539=EDGE_CURVE('',#4282,#4283,#1307,.T.);
#5540=EDGE_CURVE('',#4283,#4284,#3455,.T.);
#5541=EDGE_CURVE('',#4284,#4216,#1308,.T.);
#5542=EDGE_CURVE('',#4282,#4285,#1309,.T.);
#5543=EDGE_CURVE('',#4286,#4285,#1310,.T.);
#5544=EDGE_CURVE('',#4287,#4286,#1311,.T.);
#5545=EDGE_CURVE('',#4287,#4288,#1312,.T.);
#5546=EDGE_CURVE('',#4288,#4281,#1313,.T.);
#5547=EDGE_CURVE('',#4280,#4283,#1314,.T.);
#5548=EDGE_CURVE('',#4279,#4284,#1315,.T.);
#5549=EDGE_CURVE('',#4285,#4240,#1316,.T.);
#5550=EDGE_CURVE('',#4289,#4287,#1317,.T.);
#5551=EDGE_CURVE('',#4289,#4263,#1318,.T.);
#5552=EDGE_CURVE('',#4288,#4262,#1319,.T.);
#5553=EDGE_CURVE('',#4290,#4239,#1320,.T.);
#5554=EDGE_CURVE('',#4290,#4286,#1321,.T.);
#5555=EDGE_CURVE('',#4289,#4290,#1322,.T.);
#5556=EDGE_CURVE('',#4248,#4258,#481,.T.);
#5557=EDGE_CURVE('',#4249,#4256,#482,.T.);
#5558=EDGE_CURVE('',#4278,#4250,#483,.T.);
#5559=EDGE_CURVE('',#4259,#4247,#484,.T.);
#5560=EDGE_CURVE('',#4257,#4246,#485,.T.);
#5561=EDGE_CURVE('',#4245,#4275,#486,.T.);
#5562=EDGE_CURVE('',#4291,#4277,#1323,.T.);
#5563=EDGE_CURVE('',#4273,#4291,#3456,.T.);
#5564=EDGE_CURVE('',#4237,#4253,#487,.T.);
#5565=EDGE_CURVE('',#4292,#4291,#3457,.T.);
#5566=EDGE_CURVE('',#4274,#4292,#3458,.T.);
#5567=EDGE_CURVE('',#4238,#4292,#1324,.T.);
#5568=EDGE_CURVE('',#4293,#4272,#3459,.T.);
#5569=EDGE_CURVE('',#4276,#4293,#1325,.T.);
#5570=EDGE_CURVE('',#4242,#4265,#488,.T.);
#5571=EDGE_CURVE('',#4294,#4271,#3460,.T.);
#5572=EDGE_CURVE('',#4293,#4294,#3461,.T.);
#5573=EDGE_CURVE('',#4294,#4264,#1326,.T.);
#5574=EDGE_CURVE('',#4276,#4264,#1327,.T.);
#5575=EDGE_CURVE('',#4277,#4238,#1328,.T.);
#5576=EDGE_CURVE('',#4295,#4295,#3462,.T.);
#5577=EDGE_CURVE('',#4295,#4296,#3463,.T.);
#5578=EDGE_CURVE('',#4297,#4297,#3464,.T.);
#5579=EDGE_CURVE('',#4298,#4297,#3465,.T.);
#5580=EDGE_CURVE('',#4299,#4299,#3466,.T.);
#5581=EDGE_CURVE('',#4299,#4300,#1329,.T.);
#5582=EDGE_CURVE('',#4300,#4300,#3467,.T.);
#5583=EDGE_CURVE('',#4301,#4301,#3468,.T.);
#5584=EDGE_CURVE('',#4302,#4302,#3469,.T.);
#5585=EDGE_CURVE('',#4302,#4303,#1330,.T.);
#5586=EDGE_CURVE('',#4303,#4303,#3470,.T.);
#5587=EDGE_CURVE('',#4304,#4304,#3471,.T.);
#5588=EDGE_CURVE('',#4305,#4305,#3472,.T.);
#5589=EDGE_CURVE('',#4305,#4306,#1331,.T.);
#5590=EDGE_CURVE('',#4307,#4306,#3473,.T.);
#5591=EDGE_CURVE('',#4308,#4307,#3474,.T.);
#5592=EDGE_CURVE('',#4306,#4308,#3475,.T.);
#5593=EDGE_CURVE('',#4309,#4310,#3476,.T.);
#5594=EDGE_CURVE('',#4309,#4311,#1332,.T.);
#5595=EDGE_CURVE('',#4311,#4312,#1333,.T.);
#5596=EDGE_CURVE('',#4312,#4313,#1334,.T.);
#5597=EDGE_CURVE('',#4313,#4314,#3477,.T.);
#5598=EDGE_CURVE('',#4314,#4315,#489,.T.);
#5599=EDGE_CURVE('',#4315,#4316,#490,.T.);
#5600=EDGE_CURVE('',#4317,#4316,#1335,.T.);
#5601=EDGE_CURVE('',#4317,#4318,#491,.T.);
#5602=EDGE_CURVE('',#4318,#4310,#492,.T.);
#5603=EDGE_CURVE('',#4319,#4320,#3478,.T.);
#5604=EDGE_CURVE('',#4320,#4321,#1336,.T.);
#5605=EDGE_CURVE('',#4321,#4321,#3479,.T.);
#5606=EDGE_CURVE('',#4320,#4322,#3480,.T.);
#5607=EDGE_CURVE('',#4322,#4319,#3481,.T.);
#5608=EDGE_CURVE('',#4323,#4324,#1337,.T.);
#5609=EDGE_CURVE('',#4324,#4325,#1338,.T.);
#5610=EDGE_CURVE('',#4325,#4326,#1339,.T.);
#5611=EDGE_CURVE('',#4326,#4323,#1340,.T.);
#5612=EDGE_CURVE('',#4327,#4328,#493,.T.);
#5613=EDGE_CURVE('',#4327,#4329,#494,.T.);
#5614=EDGE_CURVE('',#4329,#4330,#1341,.T.);
#5615=EDGE_CURVE('',#4330,#4331,#495,.T.);
#5616=EDGE_CURVE('',#4328,#4331,#1342,.T.);
#5617=EDGE_CURVE('',#4328,#4332,#3482,.T.);
#5618=EDGE_CURVE('',#4331,#4313,#3483,.T.);
#5619=EDGE_CURVE('',#4312,#4332,#496,.T.);
#5620=EDGE_CURVE('',#4333,#4334,#1343,.T.);
#5621=EDGE_CURVE('',#4334,#4335,#3484,.T.);
#5622=EDGE_CURVE('',#4335,#4336,#497,.T.);
#5623=EDGE_CURVE('',#4336,#4309,#3485,.T.);
#5624=EDGE_CURVE('',#4310,#4333,#498,.T.);
#5625=EDGE_CURVE('',#4330,#4337,#3486,.T.);
#5626=EDGE_CURVE('',#4337,#4338,#1344,.T.);
#5627=EDGE_CURVE('',#4338,#4314,#499,.T.);
#5628=EDGE_CURVE('',#4316,#4324,#500,.T.);
#5629=EDGE_CURVE('',#4323,#4317,#501,.T.);
#5630=EDGE_CURVE('',#4335,#4339,#1345,.T.);
#5631=EDGE_CURVE('',#4339,#4340,#502,.T.);
#5632=EDGE_CURVE('',#4340,#4341,#503,.T.);
#5633=EDGE_CURVE('',#4336,#4341,#1346,.T.);
#5634=EDGE_CURVE('',#4341,#4342,#3487,.T.);
#5635=EDGE_CURVE('',#4342,#4311,#504,.T.);
#5636=EDGE_CURVE('',#4340,#4307,#505,.T.);
#5637=EDGE_CURVE('',#4308,#4342,#506,.T.);
#5638=EDGE_CURVE('',#4332,#4322,#507,.T.);
#5639=EDGE_CURVE('',#4319,#4327,#508,.T.);
#5640=EDGE_CURVE('',#4311,#4343,#509,.T.);
#5641=EDGE_CURVE('',#4343,#4344,#510,.T.);
#5642=EDGE_CURVE('',#4344,#4345,#511,.T.);
#5643=EDGE_CURVE('',#4345,#4346,#1347,.T.);
#5644=EDGE_CURVE('',#4346,#4347,#512,.T.);
#5645=EDGE_CURVE('',#4347,#4348,#513,.T.);
#5646=EDGE_CURVE('',#4348,#4312,#121,.T.);
#5647=EDGE_CURVE('',#4324,#4338,#514,.T.);
#5648=EDGE_CURVE('',#4333,#4323,#515,.T.);
#5649=EDGE_CURVE('',#4325,#4337,#122,.T.);
#5650=EDGE_CURVE('',#4334,#4326,#123,.T.);
#5651=EDGE_CURVE('',#4329,#4346,#516,.T.);
#5652=EDGE_CURVE('',#4345,#4339,#517,.T.);
#5653=EDGE_CURVE('',#4307,#4344,#3488,.T.);
#5654=EDGE_CURVE('',#4308,#4343,#3489,.T.);
#5655=EDGE_CURVE('',#4347,#4319,#3490,.T.);
#5656=EDGE_CURVE('',#4348,#4322,#3491,.T.);
#5657=EDGE_CURVE('',#4349,#4349,#3492,.T.);
#5658=EDGE_CURVE('',#4349,#4350,#3493,.T.);
#5659=EDGE_CURVE('',#4350,#4350,#3494,.T.);
#5660=EDGE_CURVE('',#4351,#4352,#3495,.T.);
#5661=EDGE_CURVE('',#4351,#4353,#3496,.T.);
#5662=EDGE_CURVE('',#4354,#4353,#3497,.T.);
#5663=EDGE_CURVE('',#4352,#4354,#3498,.T.);
#5664=EDGE_CURVE('',#4355,#4355,#3499,.T.);
#5665=EDGE_CURVE('',#4355,#4356,#3500,.T.);
#5666=EDGE_CURVE('',#4356,#4356,#3501,.T.);
#5667=EDGE_CURVE('',#4357,#4358,#3502,.T.);
#5668=EDGE_CURVE('',#4359,#4357,#3503,.T.);
#5669=EDGE_CURVE('',#4360,#4359,#3504,.T.);
#5670=EDGE_CURVE('',#4360,#4358,#3505,.T.);
#5671=EDGE_CURVE('',#4361,#4361,#3506,.T.);
#5672=EDGE_CURVE('',#4361,#4362,#3507,.T.);
#5673=EDGE_CURVE('',#4362,#4362,#3508,.T.);
#5674=EDGE_CURVE('',#4363,#4363,#3509,.T.);
#5675=EDGE_CURVE('',#4363,#4364,#3510,.T.);
#5676=EDGE_CURVE('',#4364,#4364,#3511,.T.);
#5677=EDGE_CURVE('',#4364,#4355,#1348,.T.);
#5678=EDGE_CURVE('',#4362,#4349,#1349,.T.);
#5679=EDGE_CURVE('',#4359,#4351,#1350,.T.);
#5680=EDGE_CURVE('',#4360,#4352,#1351,.T.);
#5681=EDGE_CURVE('',#4365,#4366,#3512,.T.);
#5682=EDGE_CURVE('',#4366,#4357,#3513,.T.);
#5683=EDGE_CURVE('',#4358,#4367,#1352,.T.);
#5684=EDGE_CURVE('',#4367,#4368,#3514,.T.);
#5685=EDGE_CURVE('',#4368,#4369,#1353,.T.);
#5686=EDGE_CURVE('',#4369,#4370,#3515,.T.);
#5687=EDGE_CURVE('',#4370,#4365,#1354,.T.);
#5688=EDGE_CURVE('',#4371,#4372,#3516,.T.);
#5689=EDGE_CURVE('',#4372,#4354,#1355,.T.);
#5690=EDGE_CURVE('',#4353,#4373,#3517,.T.);
#5691=EDGE_CURVE('',#4373,#4374,#3518,.T.);
#5692=EDGE_CURVE('',#4374,#4375,#1356,.T.);
#5693=EDGE_CURVE('',#4375,#4376,#3519,.T.);
#5694=EDGE_CURVE('',#4376,#4371,#1357,.T.);
#5695=EDGE_CURVE('',#4377,#4378,#1358,.T.);
#5696=EDGE_CURVE('',#4377,#4360,#1359,.T.);
#5697=EDGE_CURVE('',#4352,#4378,#1360,.T.);
#5698=EDGE_CURVE('',#4379,#4380,#1361,.T.);
#5699=EDGE_CURVE('',#4379,#4377,#3520,.T.);
#5700=EDGE_CURVE('',#4378,#4380,#3521,.T.);
#5701=EDGE_CURVE('',#4381,#4382,#1362,.T.);
#5702=EDGE_CURVE('',#4381,#4379,#1363,.T.);
#5703=EDGE_CURVE('',#4380,#4382,#1364,.T.);
#5704=EDGE_CURVE('',#4383,#4384,#1365,.T.);
#5705=EDGE_CURVE('',#4383,#4381,#3522,.T.);
#5706=EDGE_CURVE('',#4382,#4384,#3523,.T.);
#5707=EDGE_CURVE('',#4385,#4386,#1366,.T.);
#5708=EDGE_CURVE('',#4385,#4383,#1367,.T.);
#5709=EDGE_CURVE('',#4384,#4386,#1368,.T.);
#5710=EDGE_CURVE('',#4387,#4388,#1369,.T.);
#5711=EDGE_CURVE('',#4387,#4385,#3524,.T.);
#5712=EDGE_CURVE('',#4386,#4388,#3525,.T.);
#5713=EDGE_CURVE('',#4359,#4387,#3526,.T.);
#5714=EDGE_CURVE('',#4388,#4351,#3527,.T.);
#5715=EDGE_CURVE('',#4379,#4368,#518,.T.);
#5716=EDGE_CURVE('',#4369,#4381,#3528,.T.);
#5717=EDGE_CURVE('',#4370,#4383,#519,.T.);
#5718=EDGE_CURVE('',#4377,#4367,#520,.T.);
#5719=EDGE_CURVE('',#4365,#4385,#521,.T.);
#5720=EDGE_CURVE('',#4366,#4387,#3529,.T.);
#5721=EDGE_CURVE('',#4375,#4384,#522,.T.);
#5722=EDGE_CURVE('',#4386,#4374,#523,.T.);
#5723=EDGE_CURVE('',#4388,#4373,#3530,.T.);
#5724=EDGE_CURVE('',#4376,#4382,#3531,.T.);
#5725=EDGE_CURVE('',#4371,#4380,#524,.T.);
#5726=EDGE_CURVE('',#4372,#4378,#525,.T.);
#5727=ORIENTED_EDGE('',*,*,#4389,.T.);
#5728=ORIENTED_EDGE('',*,*,#4390,.F.);
#5729=ORIENTED_EDGE('',*,*,#4391,.T.);
#5730=ORIENTED_EDGE('',*,*,#4392,.T.);
#5731=ORIENTED_EDGE('',*,*,#4391,.F.);
#5732=ORIENTED_EDGE('',*,*,#4393,.F.);
#5733=ORIENTED_EDGE('',*,*,#4393,.T.);
#5734=ORIENTED_EDGE('',*,*,#4392,.F.);
#5735=ORIENTED_EDGE('',*,*,#4389,.F.);
#5736=ORIENTED_EDGE('',*,*,#4390,.T.);
#5737=ORIENTED_EDGE('',*,*,#4394,.T.);
#5738=ORIENTED_EDGE('',*,*,#4395,.T.);
#5739=ORIENTED_EDGE('',*,*,#4396,.T.);
#5740=ORIENTED_EDGE('',*,*,#4397,.F.);
#5741=ORIENTED_EDGE('',*,*,#4398,.F.);
#5742=ORIENTED_EDGE('',*,*,#4396,.F.);
#5743=ORIENTED_EDGE('',*,*,#4399,.T.);
#5744=ORIENTED_EDGE('',*,*,#4400,.T.);
#5745=ORIENTED_EDGE('',*,*,#4401,.F.);
#5746=ORIENTED_EDGE('',*,*,#4402,.F.);
#5747=ORIENTED_EDGE('',*,*,#4400,.F.);
#5748=ORIENTED_EDGE('',*,*,#4402,.T.);
#5749=ORIENTED_EDGE('',*,*,#4403,.T.);
#5750=ORIENTED_EDGE('',*,*,#4404,.F.);
#5751=ORIENTED_EDGE('',*,*,#4403,.F.);
#5752=ORIENTED_EDGE('',*,*,#4401,.T.);
#5753=ORIENTED_EDGE('',*,*,#4405,.T.);
#5754=ORIENTED_EDGE('',*,*,#4406,.T.);
#5755=ORIENTED_EDGE('',*,*,#4394,.F.);
#5756=ORIENTED_EDGE('',*,*,#4395,.F.);
#5757=ORIENTED_EDGE('',*,*,#4406,.F.);
#5758=ORIENTED_EDGE('',*,*,#4397,.T.);
#5759=ORIENTED_EDGE('',*,*,#4398,.T.);
#5760=ORIENTED_EDGE('',*,*,#4407,.T.);
#5761=ORIENTED_EDGE('',*,*,#4408,.F.);
#5762=ORIENTED_EDGE('',*,*,#4409,.F.);
#5763=ORIENTED_EDGE('',*,*,#4410,.F.);
#5764=ORIENTED_EDGE('',*,*,#4407,.F.);
#5765=ORIENTED_EDGE('',*,*,#4411,.F.);
#5766=ORIENTED_EDGE('',*,*,#4412,.T.);
#5767=ORIENTED_EDGE('',*,*,#4409,.T.);
#5768=ORIENTED_EDGE('',*,*,#4413,.F.);
#5769=ORIENTED_EDGE('',*,*,#4414,.F.);
#5770=ORIENTED_EDGE('',*,*,#4415,.T.);
#5771=ORIENTED_EDGE('',*,*,#4411,.T.);
#5772=ORIENTED_EDGE('',*,*,#4416,.F.);
#5773=ORIENTED_EDGE('',*,*,#4417,.F.);
#5774=ORIENTED_EDGE('',*,*,#4418,.T.);
#5775=ORIENTED_EDGE('',*,*,#4414,.T.);
#5776=ORIENTED_EDGE('',*,*,#4419,.F.);
#5777=ORIENTED_EDGE('',*,*,#4417,.T.);
#5778=ORIENTED_EDGE('',*,*,#4420,.T.);
#5779=ORIENTED_EDGE('',*,*,#4399,.F.);
#5780=ORIENTED_EDGE('',*,*,#4420,.F.);
#5781=ORIENTED_EDGE('',*,*,#4421,.T.);
#5782=ORIENTED_EDGE('',*,*,#4412,.F.);
#5783=ORIENTED_EDGE('',*,*,#4422,.F.);
#5784=ORIENTED_EDGE('',*,*,#4413,.T.);
#5785=ORIENTED_EDGE('',*,*,#4408,.T.);
#5786=ORIENTED_EDGE('',*,*,#4410,.T.);
#5787=ORIENTED_EDGE('',*,*,#4415,.F.);
#5788=ORIENTED_EDGE('',*,*,#4423,.F.);
#5789=ORIENTED_EDGE('',*,*,#4416,.T.);
#5790=ORIENTED_EDGE('',*,*,#4422,.T.);
#5791=ORIENTED_EDGE('',*,*,#4418,.F.);
#5792=ORIENTED_EDGE('',*,*,#4421,.F.);
#5793=ORIENTED_EDGE('',*,*,#4419,.T.);
#5794=ORIENTED_EDGE('',*,*,#4423,.T.);
#5795=ORIENTED_EDGE('',*,*,#4405,.F.);
#5796=ORIENTED_EDGE('',*,*,#4404,.T.);
#5797=ORIENTED_EDGE('',*,*,#4424,.T.);
#5798=ORIENTED_EDGE('',*,*,#4425,.F.);
#5799=ORIENTED_EDGE('',*,*,#4426,.T.);
#5800=ORIENTED_EDGE('',*,*,#4427,.T.);
#5801=ORIENTED_EDGE('',*,*,#4426,.F.);
#5802=ORIENTED_EDGE('',*,*,#4428,.F.);
#5803=ORIENTED_EDGE('',*,*,#4428,.T.);
#5804=ORIENTED_EDGE('',*,*,#4427,.F.);
#5805=ORIENTED_EDGE('',*,*,#4424,.F.);
#5806=ORIENTED_EDGE('',*,*,#4425,.T.);
#5807=ORIENTED_EDGE('',*,*,#4429,.T.);
#5808=ORIENTED_EDGE('',*,*,#4430,.F.);
#5809=ORIENTED_EDGE('',*,*,#4431,.T.);
#5810=ORIENTED_EDGE('',*,*,#4432,.T.);
#5811=ORIENTED_EDGE('',*,*,#4433,.F.);
#5812=ORIENTED_EDGE('',*,*,#4434,.F.);
#5813=ORIENTED_EDGE('',*,*,#4435,.F.);
#5814=ORIENTED_EDGE('',*,*,#4436,.F.);
#5815=ORIENTED_EDGE('',*,*,#4437,.F.);
#5816=ORIENTED_EDGE('',*,*,#4438,.F.);
#5817=ORIENTED_EDGE('',*,*,#4439,.F.);
#5818=ORIENTED_EDGE('',*,*,#4440,.F.);
#5819=ORIENTED_EDGE('',*,*,#4441,.F.);
#5820=ORIENTED_EDGE('',*,*,#4442,.F.);
#5821=ORIENTED_EDGE('',*,*,#4443,.F.);
#5822=ORIENTED_EDGE('',*,*,#4444,.F.);
#5823=ORIENTED_EDGE('',*,*,#4445,.F.);
#5824=ORIENTED_EDGE('',*,*,#4446,.F.);
#5825=ORIENTED_EDGE('',*,*,#4447,.T.);
#5826=ORIENTED_EDGE('',*,*,#4448,.F.);
#5827=ORIENTED_EDGE('',*,*,#4449,.F.);
#5828=ORIENTED_EDGE('',*,*,#4450,.F.);
#5829=ORIENTED_EDGE('',*,*,#4451,.T.);
#5830=ORIENTED_EDGE('',*,*,#4452,.F.);
#5831=ORIENTED_EDGE('',*,*,#4453,.F.);
#5832=ORIENTED_EDGE('',*,*,#4454,.F.);
#5833=ORIENTED_EDGE('',*,*,#4455,.F.);
#5834=ORIENTED_EDGE('',*,*,#4452,.T.);
#5835=ORIENTED_EDGE('',*,*,#4456,.T.);
#5836=ORIENTED_EDGE('',*,*,#4457,.T.);
#5837=ORIENTED_EDGE('',*,*,#4458,.T.);
#5838=ORIENTED_EDGE('',*,*,#4446,.T.);
#5839=ORIENTED_EDGE('',*,*,#4459,.F.);
#5840=ORIENTED_EDGE('',*,*,#4460,.F.);
#5841=ORIENTED_EDGE('',*,*,#4461,.T.);
#5842=ORIENTED_EDGE('',*,*,#4462,.T.);
#5843=ORIENTED_EDGE('',*,*,#4461,.F.);
#5844=ORIENTED_EDGE('',*,*,#4463,.F.);
#5845=ORIENTED_EDGE('',*,*,#4464,.T.);
#5846=ORIENTED_EDGE('',*,*,#4465,.T.);
#5847=ORIENTED_EDGE('',*,*,#4464,.F.);
#5848=ORIENTED_EDGE('',*,*,#4466,.T.);
#5849=ORIENTED_EDGE('',*,*,#4432,.F.);
#5850=ORIENTED_EDGE('',*,*,#4467,.T.);
#5851=ORIENTED_EDGE('',*,*,#4468,.F.);
#5852=ORIENTED_EDGE('',*,*,#4469,.T.);
#5853=ORIENTED_EDGE('',*,*,#4470,.F.);
#5854=ORIENTED_EDGE('',*,*,#4471,.T.);
#5855=ORIENTED_EDGE('',*,*,#4472,.F.);
#5856=ORIENTED_EDGE('',*,*,#4473,.T.);
#5857=ORIENTED_EDGE('',*,*,#4437,.T.);
#5858=ORIENTED_EDGE('',*,*,#4474,.T.);
#5859=ORIENTED_EDGE('',*,*,#4475,.F.);
#5860=ORIENTED_EDGE('',*,*,#4476,.T.);
#5861=ORIENTED_EDGE('',*,*,#4477,.F.);
#5862=ORIENTED_EDGE('',*,*,#4478,.F.);
#5863=ORIENTED_EDGE('',*,*,#4479,.F.);
#5864=ORIENTED_EDGE('',*,*,#4480,.F.);
#5865=ORIENTED_EDGE('',*,*,#4481,.F.);
#5866=ORIENTED_EDGE('',*,*,#4482,.F.);
#5867=ORIENTED_EDGE('',*,*,#4483,.T.);
#5868=ORIENTED_EDGE('',*,*,#4484,.F.);
#5869=ORIENTED_EDGE('',*,*,#4485,.T.);
#5870=ORIENTED_EDGE('',*,*,#4486,.F.);
#5871=ORIENTED_EDGE('',*,*,#4487,.T.);
#5872=ORIENTED_EDGE('',*,*,#4488,.F.);
#5873=ORIENTED_EDGE('',*,*,#4489,.F.);
#5874=ORIENTED_EDGE('',*,*,#4490,.T.);
#5875=ORIENTED_EDGE('',*,*,#4491,.T.);
#5876=ORIENTED_EDGE('',*,*,#4492,.F.);
#5877=ORIENTED_EDGE('',*,*,#4493,.F.);
#5878=ORIENTED_EDGE('',*,*,#4494,.T.);
#5879=ORIENTED_EDGE('',*,*,#4495,.T.);
#5880=ORIENTED_EDGE('',*,*,#4496,.F.);
#5881=ORIENTED_EDGE('',*,*,#4497,.T.);
#5882=ORIENTED_EDGE('',*,*,#4498,.F.);
#5883=ORIENTED_EDGE('',*,*,#4499,.F.);
#5884=ORIENTED_EDGE('',*,*,#4500,.T.);
#5885=ORIENTED_EDGE('',*,*,#4501,.F.);
#5886=ORIENTED_EDGE('',*,*,#4502,.F.);
#5887=ORIENTED_EDGE('',*,*,#4503,.F.);
#5888=ORIENTED_EDGE('',*,*,#4504,.T.);
#5889=ORIENTED_EDGE('',*,*,#4505,.F.);
#5890=ORIENTED_EDGE('',*,*,#4506,.F.);
#5891=ORIENTED_EDGE('',*,*,#4507,.F.);
#5892=ORIENTED_EDGE('',*,*,#4508,.T.);
#5893=ORIENTED_EDGE('',*,*,#4509,.F.);
#5894=ORIENTED_EDGE('',*,*,#4510,.F.);
#5895=ORIENTED_EDGE('',*,*,#4511,.F.);
#5896=ORIENTED_EDGE('',*,*,#4512,.T.);
#5897=ORIENTED_EDGE('',*,*,#4513,.F.);
#5898=ORIENTED_EDGE('',*,*,#4514,.F.);
#5899=ORIENTED_EDGE('',*,*,#4515,.F.);
#5900=ORIENTED_EDGE('',*,*,#4516,.T.);
#5901=ORIENTED_EDGE('',*,*,#4517,.F.);
#5902=ORIENTED_EDGE('',*,*,#4518,.F.);
#5903=ORIENTED_EDGE('',*,*,#4519,.F.);
#5904=ORIENTED_EDGE('',*,*,#4520,.T.);
#5905=ORIENTED_EDGE('',*,*,#4521,.F.);
#5906=ORIENTED_EDGE('',*,*,#4522,.F.);
#5907=ORIENTED_EDGE('',*,*,#4523,.F.);
#5908=ORIENTED_EDGE('',*,*,#4524,.T.);
#5909=ORIENTED_EDGE('',*,*,#4525,.F.);
#5910=ORIENTED_EDGE('',*,*,#4526,.F.);
#5911=ORIENTED_EDGE('',*,*,#4527,.F.);
#5912=ORIENTED_EDGE('',*,*,#4528,.F.);
#5913=ORIENTED_EDGE('',*,*,#4529,.F.);
#5914=ORIENTED_EDGE('',*,*,#4530,.F.);
#5915=ORIENTED_EDGE('',*,*,#4531,.F.);
#5916=ORIENTED_EDGE('',*,*,#4532,.F.);
#5917=ORIENTED_EDGE('',*,*,#4533,.F.);
#5918=ORIENTED_EDGE('',*,*,#4534,.F.);
#5919=ORIENTED_EDGE('',*,*,#4535,.F.);
#5920=ORIENTED_EDGE('',*,*,#4536,.F.);
#5921=ORIENTED_EDGE('',*,*,#4537,.F.);
#5922=ORIENTED_EDGE('',*,*,#4538,.F.);
#5923=ORIENTED_EDGE('',*,*,#4539,.F.);
#5924=ORIENTED_EDGE('',*,*,#4540,.F.);
#5925=ORIENTED_EDGE('',*,*,#4541,.F.);
#5926=ORIENTED_EDGE('',*,*,#4542,.F.);
#5927=ORIENTED_EDGE('',*,*,#4543,.F.);
#5928=ORIENTED_EDGE('',*,*,#4544,.F.);
#5929=ORIENTED_EDGE('',*,*,#4545,.F.);
#5930=ORIENTED_EDGE('',*,*,#4546,.F.);
#5931=ORIENTED_EDGE('',*,*,#4547,.F.);
#5932=ORIENTED_EDGE('',*,*,#4548,.F.);
#5933=ORIENTED_EDGE('',*,*,#4549,.F.);
#5934=ORIENTED_EDGE('',*,*,#4550,.F.);
#5935=ORIENTED_EDGE('',*,*,#4493,.T.);
#5936=ORIENTED_EDGE('',*,*,#4551,.T.);
#5937=ORIENTED_EDGE('',*,*,#4498,.T.);
#5938=ORIENTED_EDGE('',*,*,#4552,.T.);
#5939=ORIENTED_EDGE('',*,*,#4553,.T.);
#5940=ORIENTED_EDGE('',*,*,#4554,.T.);
#5941=ORIENTED_EDGE('',*,*,#4555,.T.);
#5942=ORIENTED_EDGE('',*,*,#4556,.T.);
#5943=ORIENTED_EDGE('',*,*,#4557,.T.);
#5944=ORIENTED_EDGE('',*,*,#4558,.T.);
#5945=ORIENTED_EDGE('',*,*,#4559,.T.);
#5946=ORIENTED_EDGE('',*,*,#4560,.T.);
#5947=ORIENTED_EDGE('',*,*,#4561,.T.);
#5948=ORIENTED_EDGE('',*,*,#4562,.T.);
#5949=ORIENTED_EDGE('',*,*,#4563,.T.);
#5950=ORIENTED_EDGE('',*,*,#4564,.T.);
#5951=ORIENTED_EDGE('',*,*,#4565,.T.);
#5952=ORIENTED_EDGE('',*,*,#4566,.T.);
#5953=ORIENTED_EDGE('',*,*,#4567,.T.);
#5954=ORIENTED_EDGE('',*,*,#4568,.T.);
#5955=ORIENTED_EDGE('',*,*,#4569,.T.);
#5956=ORIENTED_EDGE('',*,*,#4570,.T.);
#5957=ORIENTED_EDGE('',*,*,#4571,.T.);
#5958=ORIENTED_EDGE('',*,*,#4572,.T.);
#5959=ORIENTED_EDGE('',*,*,#4573,.T.);
#5960=ORIENTED_EDGE('',*,*,#4574,.T.);
#5961=ORIENTED_EDGE('',*,*,#4575,.T.);
#5962=ORIENTED_EDGE('',*,*,#4576,.T.);
#5963=ORIENTED_EDGE('',*,*,#4577,.T.);
#5964=ORIENTED_EDGE('',*,*,#4578,.T.);
#5965=ORIENTED_EDGE('',*,*,#4579,.T.);
#5966=ORIENTED_EDGE('',*,*,#4580,.F.);
#5967=ORIENTED_EDGE('',*,*,#4581,.T.);
#5968=ORIENTED_EDGE('',*,*,#4582,.T.);
#5969=ORIENTED_EDGE('',*,*,#4583,.T.);
#5970=ORIENTED_EDGE('',*,*,#4584,.T.);
#5971=ORIENTED_EDGE('',*,*,#4435,.T.);
#5972=ORIENTED_EDGE('',*,*,#4585,.F.);
#5973=ORIENTED_EDGE('',*,*,#4586,.F.);
#5974=ORIENTED_EDGE('',*,*,#4481,.T.);
#5975=ORIENTED_EDGE('',*,*,#4587,.F.);
#5976=ORIENTED_EDGE('',*,*,#4479,.T.);
#5977=ORIENTED_EDGE('',*,*,#4588,.T.);
#5978=ORIENTED_EDGE('',*,*,#4489,.T.);
#5979=ORIENTED_EDGE('',*,*,#4589,.T.);
#5980=ORIENTED_EDGE('',*,*,#4460,.T.);
#5981=ORIENTED_EDGE('',*,*,#4502,.T.);
#5982=ORIENTED_EDGE('',*,*,#4590,.T.);
#5983=ORIENTED_EDGE('',*,*,#4538,.T.);
#5984=ORIENTED_EDGE('',*,*,#4591,.T.);
#5985=ORIENTED_EDGE('',*,*,#4506,.T.);
#5986=ORIENTED_EDGE('',*,*,#4592,.T.);
#5987=ORIENTED_EDGE('',*,*,#4542,.T.);
#5988=ORIENTED_EDGE('',*,*,#4593,.T.);
#5989=ORIENTED_EDGE('',*,*,#4510,.T.);
#5990=ORIENTED_EDGE('',*,*,#4594,.T.);
#5991=ORIENTED_EDGE('',*,*,#4546,.T.);
#5992=ORIENTED_EDGE('',*,*,#4595,.T.);
#5993=ORIENTED_EDGE('',*,*,#4514,.T.);
#5994=ORIENTED_EDGE('',*,*,#4596,.T.);
#5995=ORIENTED_EDGE('',*,*,#4550,.T.);
#5996=ORIENTED_EDGE('',*,*,#4597,.T.);
#5997=ORIENTED_EDGE('',*,*,#4518,.T.);
#5998=ORIENTED_EDGE('',*,*,#4598,.T.);
#5999=ORIENTED_EDGE('',*,*,#4534,.T.);
#6000=ORIENTED_EDGE('',*,*,#4599,.T.);
#6001=ORIENTED_EDGE('',*,*,#4522,.T.);
#6002=ORIENTED_EDGE('',*,*,#4600,.T.);
#6003=ORIENTED_EDGE('',*,*,#4530,.T.);
#6004=ORIENTED_EDGE('',*,*,#4601,.T.);
#6005=ORIENTED_EDGE('',*,*,#4528,.T.);
#6006=ORIENTED_EDGE('',*,*,#4602,.T.);
#6007=ORIENTED_EDGE('',*,*,#4603,.T.);
#6008=ORIENTED_EDGE('',*,*,#4604,.T.);
#6009=ORIENTED_EDGE('',*,*,#4532,.T.);
#6010=ORIENTED_EDGE('',*,*,#4605,.T.);
#6011=ORIENTED_EDGE('',*,*,#4606,.T.);
#6012=ORIENTED_EDGE('',*,*,#4607,.T.);
#6013=ORIENTED_EDGE('',*,*,#4548,.T.);
#6014=ORIENTED_EDGE('',*,*,#4608,.T.);
#6015=ORIENTED_EDGE('',*,*,#4609,.T.);
#6016=ORIENTED_EDGE('',*,*,#4610,.T.);
#6017=ORIENTED_EDGE('',*,*,#4544,.T.);
#6018=ORIENTED_EDGE('',*,*,#4611,.T.);
#6019=ORIENTED_EDGE('',*,*,#4612,.T.);
#6020=ORIENTED_EDGE('',*,*,#4613,.T.);
#6021=ORIENTED_EDGE('',*,*,#4540,.T.);
#6022=ORIENTED_EDGE('',*,*,#4614,.T.);
#6023=ORIENTED_EDGE('',*,*,#4615,.T.);
#6024=ORIENTED_EDGE('',*,*,#4616,.T.);
#6025=ORIENTED_EDGE('',*,*,#4536,.T.);
#6026=ORIENTED_EDGE('',*,*,#4617,.T.);
#6027=ORIENTED_EDGE('',*,*,#4618,.T.);
#6028=ORIENTED_EDGE('',*,*,#4619,.T.);
#6029=ORIENTED_EDGE('',*,*,#4620,.F.);
#6030=ORIENTED_EDGE('',*,*,#4577,.F.);
#6031=ORIENTED_EDGE('',*,*,#4621,.F.);
#6032=ORIENTED_EDGE('',*,*,#4603,.F.);
#6033=ORIENTED_EDGE('',*,*,#4622,.F.);
#6034=ORIENTED_EDGE('',*,*,#4573,.F.);
#6035=ORIENTED_EDGE('',*,*,#4623,.F.);
#6036=ORIENTED_EDGE('',*,*,#4606,.F.);
#6037=ORIENTED_EDGE('',*,*,#4624,.F.);
#6038=ORIENTED_EDGE('',*,*,#4569,.F.);
#6039=ORIENTED_EDGE('',*,*,#4625,.F.);
#6040=ORIENTED_EDGE('',*,*,#4609,.F.);
#6041=ORIENTED_EDGE('',*,*,#4626,.F.);
#6042=ORIENTED_EDGE('',*,*,#4565,.F.);
#6043=ORIENTED_EDGE('',*,*,#4627,.F.);
#6044=ORIENTED_EDGE('',*,*,#4612,.F.);
#6045=ORIENTED_EDGE('',*,*,#4628,.F.);
#6046=ORIENTED_EDGE('',*,*,#4561,.F.);
#6047=ORIENTED_EDGE('',*,*,#4629,.F.);
#6048=ORIENTED_EDGE('',*,*,#4615,.F.);
#6049=ORIENTED_EDGE('',*,*,#4630,.F.);
#6050=ORIENTED_EDGE('',*,*,#4557,.F.);
#6051=ORIENTED_EDGE('',*,*,#4631,.F.);
#6052=ORIENTED_EDGE('',*,*,#4618,.F.);
#6053=ORIENTED_EDGE('',*,*,#4632,.F.);
#6054=ORIENTED_EDGE('',*,*,#4553,.F.);
#6055=ORIENTED_EDGE('',*,*,#4633,.F.);
#6056=ORIENTED_EDGE('',*,*,#4497,.F.);
#6057=ORIENTED_EDGE('',*,*,#4634,.T.);
#6058=ORIENTED_EDGE('',*,*,#4633,.T.);
#6059=ORIENTED_EDGE('',*,*,#4552,.F.);
#6060=ORIENTED_EDGE('',*,*,#4483,.F.);
#6061=ORIENTED_EDGE('',*,*,#4635,.F.);
#6062=ORIENTED_EDGE('',*,*,#4636,.T.);
#6063=ORIENTED_EDGE('',*,*,#4637,.F.);
#6064=ORIENTED_EDGE('',*,*,#4638,.T.);
#6065=ORIENTED_EDGE('',*,*,#4484,.T.);
#6066=ORIENTED_EDGE('',*,*,#4637,.T.);
#6067=ORIENTED_EDGE('',*,*,#4639,.T.);
#6068=ORIENTED_EDGE('',*,*,#4635,.T.);
#6069=ORIENTED_EDGE('',*,*,#4482,.T.);
#6070=ORIENTED_EDGE('',*,*,#4586,.T.);
#6071=ORIENTED_EDGE('',*,*,#4640,.T.);
#6072=ORIENTED_EDGE('',*,*,#4641,.T.);
#6073=ORIENTED_EDGE('',*,*,#4642,.T.);
#6074=ORIENTED_EDGE('',*,*,#4643,.T.);
#6075=ORIENTED_EDGE('',*,*,#4644,.T.);
#6076=ORIENTED_EDGE('',*,*,#4450,.T.);
#6077=ORIENTED_EDGE('',*,*,#4645,.T.);
#6078=ORIENTED_EDGE('',*,*,#4438,.T.);
#6079=ORIENTED_EDGE('',*,*,#4646,.T.);
#6080=ORIENTED_EDGE('',*,*,#4647,.T.);
#6081=ORIENTED_EDGE('',*,*,#4468,.T.);
#6082=ORIENTED_EDGE('',*,*,#4648,.T.);
#6083=ORIENTED_EDGE('',*,*,#4641,.F.);
#6084=ORIENTED_EDGE('',*,*,#4441,.T.);
#6085=ORIENTED_EDGE('',*,*,#4649,.F.);
#6086=ORIENTED_EDGE('',*,*,#4445,.T.);
#6087=ORIENTED_EDGE('',*,*,#4650,.T.);
#6088=ORIENTED_EDGE('',*,*,#4651,.T.);
#6089=ORIENTED_EDGE('',*,*,#4472,.T.);
#6090=ORIENTED_EDGE('',*,*,#4652,.T.);
#6091=ORIENTED_EDGE('',*,*,#4653,.T.);
#6092=ORIENTED_EDGE('',*,*,#4654,.T.);
#6093=ORIENTED_EDGE('',*,*,#4470,.T.);
#6094=ORIENTED_EDGE('',*,*,#4655,.T.);
#6095=ORIENTED_EDGE('',*,*,#4656,.T.);
#6096=ORIENTED_EDGE('',*,*,#4657,.F.);
#6097=ORIENTED_EDGE('',*,*,#4658,.T.);
#6098=ORIENTED_EDGE('',*,*,#4659,.T.);
#6099=ORIENTED_EDGE('',*,*,#4660,.F.);
#6100=ORIENTED_EDGE('',*,*,#4661,.F.);
#6101=ORIENTED_EDGE('',*,*,#4662,.T.);
#6102=ORIENTED_EDGE('',*,*,#4663,.T.);
#6103=ORIENTED_EDGE('',*,*,#4664,.F.);
#6104=ORIENTED_EDGE('',*,*,#4660,.T.);
#6105=ORIENTED_EDGE('',*,*,#4665,.T.);
#6106=ORIENTED_EDGE('',*,*,#4666,.T.);
#6107=ORIENTED_EDGE('',*,*,#4667,.T.);
#6108=ORIENTED_EDGE('',*,*,#4668,.F.);
#6109=ORIENTED_EDGE('',*,*,#4669,.T.);
#6110=ORIENTED_EDGE('',*,*,#4670,.F.);
#6111=ORIENTED_EDGE('',*,*,#4671,.T.);
#6112=ORIENTED_EDGE('',*,*,#4672,.T.);
#6113=ORIENTED_EDGE('',*,*,#4673,.T.);
#6114=ORIENTED_EDGE('',*,*,#4580,.T.);
#6115=ORIENTED_EDGE('',*,*,#4674,.T.);
#6116=ORIENTED_EDGE('',*,*,#4675,.T.);
#6117=ORIENTED_EDGE('',*,*,#4676,.F.);
#6118=ORIENTED_EDGE('',*,*,#4677,.T.);
#6119=ORIENTED_EDGE('',*,*,#4678,.F.);
#6120=ORIENTED_EDGE('',*,*,#4679,.F.);
#6121=ORIENTED_EDGE('',*,*,#4680,.T.);
#6122=ORIENTED_EDGE('',*,*,#4681,.F.);
#6123=ORIENTED_EDGE('',*,*,#4682,.T.);
#6124=ORIENTED_EDGE('',*,*,#4683,.T.);
#6125=ORIENTED_EDGE('',*,*,#4684,.T.);
#6126=ORIENTED_EDGE('',*,*,#4685,.T.);
#6127=ORIENTED_EDGE('',*,*,#4668,.T.);
#6128=ORIENTED_EDGE('',*,*,#4475,.T.);
#6129=ORIENTED_EDGE('',*,*,#4686,.T.);
#6130=ORIENTED_EDGE('',*,*,#4679,.T.);
#6131=ORIENTED_EDGE('',*,*,#4687,.T.);
#6132=ORIENTED_EDGE('',*,*,#4681,.T.);
#6133=ORIENTED_EDGE('',*,*,#4688,.T.);
#6134=ORIENTED_EDGE('',*,*,#4672,.F.);
#6135=ORIENTED_EDGE('',*,*,#4689,.T.);
#6136=ORIENTED_EDGE('',*,*,#4690,.T.);
#6137=ORIENTED_EDGE('',*,*,#4691,.T.);
#6138=ORIENTED_EDGE('',*,*,#4692,.T.);
#6139=ORIENTED_EDGE('',*,*,#4693,.T.);
#6140=ORIENTED_EDGE('',*,*,#4694,.T.);
#6141=ORIENTED_EDGE('',*,*,#4695,.T.);
#6142=ORIENTED_EDGE('',*,*,#4670,.T.);
#6143=ORIENTED_EDGE('',*,*,#4462,.F.);
#6144=ORIENTED_EDGE('',*,*,#4666,.F.);
#6145=ORIENTED_EDGE('',*,*,#4696,.T.);
#6146=ORIENTED_EDGE('',*,*,#4697,.T.);
#6147=ORIENTED_EDGE('',*,*,#4698,.T.);
#6148=ORIENTED_EDGE('',*,*,#4699,.T.);
#6149=ORIENTED_EDGE('',*,*,#4700,.T.);
#6150=ORIENTED_EDGE('',*,*,#4701,.T.);
#6151=ORIENTED_EDGE('',*,*,#4463,.T.);
#6152=ORIENTED_EDGE('',*,*,#4656,.F.);
#6153=ORIENTED_EDGE('',*,*,#4702,.T.);
#6154=ORIENTED_EDGE('',*,*,#4658,.F.);
#6155=ORIENTED_EDGE('',*,*,#4703,.T.);
#6156=ORIENTED_EDGE('',*,*,#4701,.F.);
#6157=ORIENTED_EDGE('',*,*,#4704,.T.);
#6158=ORIENTED_EDGE('',*,*,#4683,.F.);
#6159=ORIENTED_EDGE('',*,*,#4667,.F.);
#6160=ORIENTED_EDGE('',*,*,#4685,.F.);
#6161=ORIENTED_EDGE('',*,*,#4705,.T.);
#6162=ORIENTED_EDGE('',*,*,#4690,.F.);
#6163=ORIENTED_EDGE('',*,*,#4669,.F.);
#6164=ORIENTED_EDGE('',*,*,#4706,.F.);
#6165=ORIENTED_EDGE('',*,*,#4707,.F.);
#6166=ORIENTED_EDGE('',*,*,#4677,.F.);
#6167=ORIENTED_EDGE('',*,*,#4708,.F.);
#6168=ORIENTED_EDGE('',*,*,#4709,.F.);
#6169=ORIENTED_EDGE('',*,*,#4495,.F.);
#6170=ORIENTED_EDGE('',*,*,#4710,.F.);
#6171=ORIENTED_EDGE('',*,*,#4491,.F.);
#6172=ORIENTED_EDGE('',*,*,#4711,.F.);
#6173=ORIENTED_EDGE('',*,*,#4487,.F.);
#6174=ORIENTED_EDGE('',*,*,#4712,.T.);
#6175=ORIENTED_EDGE('',*,*,#4485,.F.);
#6176=ORIENTED_EDGE('',*,*,#4638,.F.);
#6177=ORIENTED_EDGE('',*,*,#4713,.T.);
#6178=ORIENTED_EDGE('',*,*,#4433,.T.);
#6179=ORIENTED_EDGE('',*,*,#4466,.F.);
#6180=ORIENTED_EDGE('',*,*,#4657,.T.);
#6181=ORIENTED_EDGE('',*,*,#4703,.F.);
#6182=ORIENTED_EDGE('',*,*,#4661,.T.);
#6183=ORIENTED_EDGE('',*,*,#4664,.T.);
#6184=ORIENTED_EDGE('',*,*,#4714,.F.);
#6185=ORIENTED_EDGE('',*,*,#4715,.F.);
#6186=ORIENTED_EDGE('',*,*,#4524,.F.);
#6187=ORIENTED_EDGE('',*,*,#4716,.F.);
#6188=ORIENTED_EDGE('',*,*,#4717,.F.);
#6189=ORIENTED_EDGE('',*,*,#4718,.F.);
#6190=ORIENTED_EDGE('',*,*,#4520,.F.);
#6191=ORIENTED_EDGE('',*,*,#4719,.F.);
#6192=ORIENTED_EDGE('',*,*,#4720,.F.);
#6193=ORIENTED_EDGE('',*,*,#4721,.F.);
#6194=ORIENTED_EDGE('',*,*,#4516,.F.);
#6195=ORIENTED_EDGE('',*,*,#4722,.F.);
#6196=ORIENTED_EDGE('',*,*,#4723,.F.);
#6197=ORIENTED_EDGE('',*,*,#4724,.F.);
#6198=ORIENTED_EDGE('',*,*,#4512,.F.);
#6199=ORIENTED_EDGE('',*,*,#4725,.F.);
#6200=ORIENTED_EDGE('',*,*,#4726,.F.);
#6201=ORIENTED_EDGE('',*,*,#4727,.F.);
#6202=ORIENTED_EDGE('',*,*,#4508,.F.);
#6203=ORIENTED_EDGE('',*,*,#4728,.F.);
#6204=ORIENTED_EDGE('',*,*,#4729,.F.);
#6205=ORIENTED_EDGE('',*,*,#4730,.F.);
#6206=ORIENTED_EDGE('',*,*,#4504,.F.);
#6207=ORIENTED_EDGE('',*,*,#4731,.F.);
#6208=ORIENTED_EDGE('',*,*,#4732,.F.);
#6209=ORIENTED_EDGE('',*,*,#4733,.F.);
#6210=ORIENTED_EDGE('',*,*,#4500,.F.);
#6211=ORIENTED_EDGE('',*,*,#4734,.F.);
#6212=ORIENTED_EDGE('',*,*,#4735,.F.);
#6213=ORIENTED_EDGE('',*,*,#4736,.F.);
#6214=ORIENTED_EDGE('',*,*,#4465,.F.);
#6215=ORIENTED_EDGE('',*,*,#4526,.T.);
#6216=ORIENTED_EDGE('',*,*,#4737,.T.);
#6217=ORIENTED_EDGE('',*,*,#4678,.T.);
#6218=ORIENTED_EDGE('',*,*,#4707,.T.);
#6219=ORIENTED_EDGE('',*,*,#4738,.T.);
#6220=ORIENTED_EDGE('',*,*,#4676,.T.);
#6221=ORIENTED_EDGE('',*,*,#4739,.T.);
#6222=ORIENTED_EDGE('',*,*,#4708,.T.);
#6223=ORIENTED_EDGE('',*,*,#4585,.T.);
#6224=ORIENTED_EDGE('',*,*,#4434,.T.);
#6225=ORIENTED_EDGE('',*,*,#4713,.F.);
#6226=ORIENTED_EDGE('',*,*,#4639,.F.);
#6227=ORIENTED_EDGE('',*,*,#4636,.F.);
#6228=ORIENTED_EDGE('',*,*,#4640,.F.);
#6229=ORIENTED_EDGE('',*,*,#4448,.T.);
#6230=ORIENTED_EDGE('',*,*,#4740,.T.);
#6231=ORIENTED_EDGE('',*,*,#4741,.T.);
#6232=ORIENTED_EDGE('',*,*,#4742,.T.);
#6233=ORIENTED_EDGE('',*,*,#4650,.F.);
#6234=ORIENTED_EDGE('',*,*,#4444,.T.);
#6235=ORIENTED_EDGE('',*,*,#4743,.T.);
#6236=ORIENTED_EDGE('',*,*,#4744,.F.);
#6237=ORIENTED_EDGE('',*,*,#4745,.T.);
#6238=ORIENTED_EDGE('',*,*,#4746,.T.);
#6239=ORIENTED_EDGE('',*,*,#4747,.T.);
#6240=ORIENTED_EDGE('',*,*,#4442,.T.);
#6241=ORIENTED_EDGE('',*,*,#4649,.T.);
#6242=ORIENTED_EDGE('',*,*,#4440,.T.);
#6243=ORIENTED_EDGE('',*,*,#4748,.T.);
#6244=ORIENTED_EDGE('',*,*,#4749,.T.);
#6245=ORIENTED_EDGE('',*,*,#4750,.T.);
#6246=ORIENTED_EDGE('',*,*,#4751,.T.);
#6247=ORIENTED_EDGE('',*,*,#4752,.T.);
#6248=ORIENTED_EDGE('',*,*,#4744,.T.);
#6249=ORIENTED_EDGE('',*,*,#4753,.T.);
#6250=ORIENTED_EDGE('',*,*,#4754,.F.);
#6251=ORIENTED_EDGE('',*,*,#4755,.F.);
#6252=ORIENTED_EDGE('',*,*,#4756,.T.);
#6253=ORIENTED_EDGE('',*,*,#4757,.T.);
#6254=ORIENTED_EDGE('',*,*,#4755,.T.);
#6255=ORIENTED_EDGE('',*,*,#4758,.F.);
#6256=ORIENTED_EDGE('',*,*,#4759,.F.);
#6257=ORIENTED_EDGE('',*,*,#4760,.T.);
#6258=ORIENTED_EDGE('',*,*,#4761,.T.);
#6259=ORIENTED_EDGE('',*,*,#4762,.T.);
#6260=ORIENTED_EDGE('',*,*,#4763,.T.);
#6261=ORIENTED_EDGE('',*,*,#4764,.T.);
#6262=ORIENTED_EDGE('',*,*,#4765,.T.);
#6263=ORIENTED_EDGE('',*,*,#4766,.T.);
#6264=ORIENTED_EDGE('',*,*,#4767,.T.);
#6265=ORIENTED_EDGE('',*,*,#4768,.F.);
#6266=ORIENTED_EDGE('',*,*,#4767,.F.);
#6267=ORIENTED_EDGE('',*,*,#4769,.T.);
#6268=ORIENTED_EDGE('',*,*,#4457,.F.);
#6269=ORIENTED_EDGE('',*,*,#4770,.F.);
#6270=ORIENTED_EDGE('',*,*,#4771,.T.);
#6271=ORIENTED_EDGE('',*,*,#4772,.T.);
#6272=ORIENTED_EDGE('',*,*,#4751,.F.);
#6273=ORIENTED_EDGE('',*,*,#4757,.F.);
#6274=ORIENTED_EDGE('',*,*,#4773,.F.);
#6275=ORIENTED_EDGE('',*,*,#4774,.F.);
#6276=ORIENTED_EDGE('',*,*,#4775,.F.);
#6277=ORIENTED_EDGE('',*,*,#4776,.F.);
#6278=ORIENTED_EDGE('',*,*,#4777,.F.);
#6279=ORIENTED_EDGE('',*,*,#4778,.F.);
#6280=ORIENTED_EDGE('',*,*,#4779,.F.);
#6281=ORIENTED_EDGE('',*,*,#4780,.F.);
#6282=ORIENTED_EDGE('',*,*,#4781,.F.);
#6283=ORIENTED_EDGE('',*,*,#4782,.F.);
#6284=ORIENTED_EDGE('',*,*,#4783,.F.);
#6285=ORIENTED_EDGE('',*,*,#4784,.F.);
#6286=ORIENTED_EDGE('',*,*,#4785,.F.);
#6287=ORIENTED_EDGE('',*,*,#4786,.F.);
#6288=ORIENTED_EDGE('',*,*,#4787,.F.);
#6289=ORIENTED_EDGE('',*,*,#4788,.F.);
#6290=ORIENTED_EDGE('',*,*,#4789,.F.);
#6291=ORIENTED_EDGE('',*,*,#4790,.F.);
#6292=ORIENTED_EDGE('',*,*,#4791,.F.);
#6293=ORIENTED_EDGE('',*,*,#4459,.T.);
#6294=ORIENTED_EDGE('',*,*,#4792,.T.);
#6295=ORIENTED_EDGE('',*,*,#4793,.T.);
#6296=ORIENTED_EDGE('',*,*,#4770,.T.);
#6297=ORIENTED_EDGE('',*,*,#4794,.T.);
#6298=ORIENTED_EDGE('',*,*,#4795,.T.);
#6299=ORIENTED_EDGE('',*,*,#4455,.T.);
#6300=ORIENTED_EDGE('',*,*,#4796,.F.);
#6301=ORIENTED_EDGE('',*,*,#4454,.T.);
#6302=ORIENTED_EDGE('',*,*,#4797,.T.);
#6303=ORIENTED_EDGE('',*,*,#4759,.T.);
#6304=ORIENTED_EDGE('',*,*,#4798,.T.);
#6305=ORIENTED_EDGE('',*,*,#4799,.T.);
#6306=ORIENTED_EDGE('',*,*,#4800,.T.);
#6307=ORIENTED_EDGE('',*,*,#4801,.T.);
#6308=ORIENTED_EDGE('',*,*,#4802,.T.);
#6309=ORIENTED_EDGE('',*,*,#4803,.T.);
#6310=ORIENTED_EDGE('',*,*,#4804,.T.);
#6311=ORIENTED_EDGE('',*,*,#4805,.T.);
#6312=ORIENTED_EDGE('',*,*,#4806,.T.);
#6313=ORIENTED_EDGE('',*,*,#4807,.T.);
#6314=ORIENTED_EDGE('',*,*,#4808,.T.);
#6315=ORIENTED_EDGE('',*,*,#4809,.T.);
#6316=ORIENTED_EDGE('',*,*,#4810,.T.);
#6317=ORIENTED_EDGE('',*,*,#4811,.T.);
#6318=ORIENTED_EDGE('',*,*,#4812,.T.);
#6319=ORIENTED_EDGE('',*,*,#4813,.T.);
#6320=ORIENTED_EDGE('',*,*,#4814,.T.);
#6321=ORIENTED_EDGE('',*,*,#4815,.T.);
#6322=ORIENTED_EDGE('',*,*,#4816,.T.);
#6323=ORIENTED_EDGE('',*,*,#4758,.T.);
#6324=ORIENTED_EDGE('',*,*,#4754,.T.);
#6325=ORIENTED_EDGE('',*,*,#4817,.T.);
#6326=ORIENTED_EDGE('',*,*,#4818,.T.);
#6327=ORIENTED_EDGE('',*,*,#4796,.T.);
#6328=ORIENTED_EDGE('',*,*,#4818,.F.);
#6329=ORIENTED_EDGE('',*,*,#4819,.T.);
#6330=ORIENTED_EDGE('',*,*,#4820,.T.);
#6331=ORIENTED_EDGE('',*,*,#4794,.F.);
#6332=ORIENTED_EDGE('',*,*,#4821,.T.);
#6333=ORIENTED_EDGE('',*,*,#4822,.T.);
#6334=ORIENTED_EDGE('',*,*,#4771,.F.);
#6335=ORIENTED_EDGE('',*,*,#4793,.F.);
#6336=ORIENTED_EDGE('',*,*,#4773,.T.);
#6337=ORIENTED_EDGE('',*,*,#4756,.F.);
#6338=ORIENTED_EDGE('',*,*,#4816,.F.);
#6339=ORIENTED_EDGE('',*,*,#4823,.T.);
#6340=ORIENTED_EDGE('',*,*,#4774,.T.);
#6341=ORIENTED_EDGE('',*,*,#4823,.F.);
#6342=ORIENTED_EDGE('',*,*,#4815,.F.);
#6343=ORIENTED_EDGE('',*,*,#4824,.T.);
#6344=ORIENTED_EDGE('',*,*,#4775,.T.);
#6345=ORIENTED_EDGE('',*,*,#4824,.F.);
#6346=ORIENTED_EDGE('',*,*,#4814,.F.);
#6347=ORIENTED_EDGE('',*,*,#4825,.T.);
#6348=ORIENTED_EDGE('',*,*,#4776,.T.);
#6349=ORIENTED_EDGE('',*,*,#4825,.F.);
#6350=ORIENTED_EDGE('',*,*,#4813,.F.);
#6351=ORIENTED_EDGE('',*,*,#4826,.T.);
#6352=ORIENTED_EDGE('',*,*,#4777,.T.);
#6353=ORIENTED_EDGE('',*,*,#4826,.F.);
#6354=ORIENTED_EDGE('',*,*,#4812,.F.);
#6355=ORIENTED_EDGE('',*,*,#4827,.T.);
#6356=ORIENTED_EDGE('',*,*,#4778,.T.);
#6357=ORIENTED_EDGE('',*,*,#4827,.F.);
#6358=ORIENTED_EDGE('',*,*,#4811,.F.);
#6359=ORIENTED_EDGE('',*,*,#4828,.T.);
#6360=ORIENTED_EDGE('',*,*,#4779,.T.);
#6361=ORIENTED_EDGE('',*,*,#4828,.F.);
#6362=ORIENTED_EDGE('',*,*,#4810,.F.);
#6363=ORIENTED_EDGE('',*,*,#4829,.T.);
#6364=ORIENTED_EDGE('',*,*,#4780,.T.);
#6365=ORIENTED_EDGE('',*,*,#4829,.F.);
#6366=ORIENTED_EDGE('',*,*,#4809,.F.);
#6367=ORIENTED_EDGE('',*,*,#4830,.T.);
#6368=ORIENTED_EDGE('',*,*,#4781,.T.);
#6369=ORIENTED_EDGE('',*,*,#4830,.F.);
#6370=ORIENTED_EDGE('',*,*,#4808,.F.);
#6371=ORIENTED_EDGE('',*,*,#4831,.T.);
#6372=ORIENTED_EDGE('',*,*,#4782,.T.);
#6373=ORIENTED_EDGE('',*,*,#4831,.F.);
#6374=ORIENTED_EDGE('',*,*,#4807,.F.);
#6375=ORIENTED_EDGE('',*,*,#4832,.T.);
#6376=ORIENTED_EDGE('',*,*,#4783,.T.);
#6377=ORIENTED_EDGE('',*,*,#4832,.F.);
#6378=ORIENTED_EDGE('',*,*,#4806,.F.);
#6379=ORIENTED_EDGE('',*,*,#4833,.T.);
#6380=ORIENTED_EDGE('',*,*,#4784,.T.);
#6381=ORIENTED_EDGE('',*,*,#4833,.F.);
#6382=ORIENTED_EDGE('',*,*,#4805,.F.);
#6383=ORIENTED_EDGE('',*,*,#4834,.T.);
#6384=ORIENTED_EDGE('',*,*,#4785,.T.);
#6385=ORIENTED_EDGE('',*,*,#4834,.F.);
#6386=ORIENTED_EDGE('',*,*,#4804,.F.);
#6387=ORIENTED_EDGE('',*,*,#4835,.T.);
#6388=ORIENTED_EDGE('',*,*,#4786,.T.);
#6389=ORIENTED_EDGE('',*,*,#4835,.F.);
#6390=ORIENTED_EDGE('',*,*,#4803,.F.);
#6391=ORIENTED_EDGE('',*,*,#4836,.T.);
#6392=ORIENTED_EDGE('',*,*,#4787,.T.);
#6393=ORIENTED_EDGE('',*,*,#4836,.F.);
#6394=ORIENTED_EDGE('',*,*,#4802,.F.);
#6395=ORIENTED_EDGE('',*,*,#4837,.T.);
#6396=ORIENTED_EDGE('',*,*,#4788,.T.);
#6397=ORIENTED_EDGE('',*,*,#4837,.F.);
#6398=ORIENTED_EDGE('',*,*,#4801,.F.);
#6399=ORIENTED_EDGE('',*,*,#4838,.T.);
#6400=ORIENTED_EDGE('',*,*,#4789,.T.);
#6401=ORIENTED_EDGE('',*,*,#4838,.F.);
#6402=ORIENTED_EDGE('',*,*,#4800,.F.);
#6403=ORIENTED_EDGE('',*,*,#4839,.T.);
#6404=ORIENTED_EDGE('',*,*,#4790,.T.);
#6405=ORIENTED_EDGE('',*,*,#4839,.F.);
#6406=ORIENTED_EDGE('',*,*,#4799,.F.);
#6407=ORIENTED_EDGE('',*,*,#4840,.T.);
#6408=ORIENTED_EDGE('',*,*,#4791,.T.);
#6409=ORIENTED_EDGE('',*,*,#4840,.F.);
#6410=ORIENTED_EDGE('',*,*,#4798,.F.);
#6411=ORIENTED_EDGE('',*,*,#4768,.T.);
#6412=ORIENTED_EDGE('',*,*,#4841,.F.);
#6413=ORIENTED_EDGE('',*,*,#4842,.T.);
#6414=ORIENTED_EDGE('',*,*,#4645,.F.);
#6415=ORIENTED_EDGE('',*,*,#4453,.T.);
#6416=ORIENTED_EDGE('',*,*,#4795,.F.);
#6417=ORIENTED_EDGE('',*,*,#4820,.F.);
#6418=ORIENTED_EDGE('',*,*,#4843,.T.);
#6419=ORIENTED_EDGE('',*,*,#4841,.T.);
#6420=ORIENTED_EDGE('',*,*,#4743,.F.);
#6421=ORIENTED_EDGE('',*,*,#4844,.T.);
#6422=ORIENTED_EDGE('',*,*,#4845,.F.);
#6423=ORIENTED_EDGE('',*,*,#4792,.F.);
#6424=ORIENTED_EDGE('',*,*,#4449,.T.);
#6425=ORIENTED_EDGE('',*,*,#4845,.T.);
#6426=ORIENTED_EDGE('',*,*,#4846,.T.);
#6427=ORIENTED_EDGE('',*,*,#4821,.F.);
#6428=ORIENTED_EDGE('',*,*,#4443,.T.);
#6429=ORIENTED_EDGE('',*,*,#4747,.F.);
#6430=ORIENTED_EDGE('',*,*,#4847,.F.);
#6431=ORIENTED_EDGE('',*,*,#4844,.F.);
#6432=ORIENTED_EDGE('',*,*,#4847,.T.);
#6433=ORIENTED_EDGE('',*,*,#4746,.F.);
#6434=ORIENTED_EDGE('',*,*,#4848,.F.);
#6435=ORIENTED_EDGE('',*,*,#4846,.F.);
#6436=ORIENTED_EDGE('',*,*,#4848,.T.);
#6437=ORIENTED_EDGE('',*,*,#4745,.F.);
#6438=ORIENTED_EDGE('',*,*,#4752,.F.);
#6439=ORIENTED_EDGE('',*,*,#4772,.F.);
#6440=ORIENTED_EDGE('',*,*,#4822,.F.);
#6441=ORIENTED_EDGE('',*,*,#4439,.T.);
#6442=ORIENTED_EDGE('',*,*,#4842,.F.);
#6443=ORIENTED_EDGE('',*,*,#4849,.F.);
#6444=ORIENTED_EDGE('',*,*,#4748,.F.);
#6445=ORIENTED_EDGE('',*,*,#4849,.T.);
#6446=ORIENTED_EDGE('',*,*,#4843,.F.);
#6447=ORIENTED_EDGE('',*,*,#4850,.F.);
#6448=ORIENTED_EDGE('',*,*,#4749,.F.);
#6449=ORIENTED_EDGE('',*,*,#4850,.T.);
#6450=ORIENTED_EDGE('',*,*,#4819,.F.);
#6451=ORIENTED_EDGE('',*,*,#4817,.F.);
#6452=ORIENTED_EDGE('',*,*,#4753,.F.);
#6453=ORIENTED_EDGE('',*,*,#4750,.F.);
#6454=ORIENTED_EDGE('',*,*,#4587,.T.);
#6455=ORIENTED_EDGE('',*,*,#4480,.T.);
#6456=ORIENTED_EDGE('',*,*,#4851,.T.);
#6457=ORIENTED_EDGE('',*,*,#4852,.T.);
#6458=ORIENTED_EDGE('',*,*,#4736,.T.);
#6459=ORIENTED_EDGE('',*,*,#4735,.T.);
#6460=ORIENTED_EDGE('',*,*,#4853,.T.);
#6461=ORIENTED_EDGE('',*,*,#4851,.F.);
#6462=ORIENTED_EDGE('',*,*,#4486,.T.);
#6463=ORIENTED_EDGE('',*,*,#4712,.F.);
#6464=ORIENTED_EDGE('',*,*,#4673,.F.);
#6465=ORIENTED_EDGE('',*,*,#4688,.F.);
#6466=ORIENTED_EDGE('',*,*,#4854,.F.);
#6467=ORIENTED_EDGE('',*,*,#4581,.F.);
#6468=ORIENTED_EDGE('',*,*,#4854,.T.);
#6469=ORIENTED_EDGE('',*,*,#4680,.F.);
#6470=ORIENTED_EDGE('',*,*,#4855,.F.);
#6471=ORIENTED_EDGE('',*,*,#4582,.F.);
#6472=ORIENTED_EDGE('',*,*,#4855,.T.);
#6473=ORIENTED_EDGE('',*,*,#4686,.F.);
#6474=ORIENTED_EDGE('',*,*,#4856,.F.);
#6475=ORIENTED_EDGE('',*,*,#4583,.F.);
#6476=ORIENTED_EDGE('',*,*,#4474,.F.);
#6477=ORIENTED_EDGE('',*,*,#4436,.T.);
#6478=ORIENTED_EDGE('',*,*,#4584,.F.);
#6479=ORIENTED_EDGE('',*,*,#4856,.T.);
#6480=ORIENTED_EDGE('',*,*,#4671,.F.);
#6481=ORIENTED_EDGE('',*,*,#4695,.F.);
#6482=ORIENTED_EDGE('',*,*,#4857,.F.);
#6483=ORIENTED_EDGE('',*,*,#4689,.F.);
#6484=ORIENTED_EDGE('',*,*,#4857,.T.);
#6485=ORIENTED_EDGE('',*,*,#4694,.F.);
#6486=ORIENTED_EDGE('',*,*,#4858,.F.);
#6487=ORIENTED_EDGE('',*,*,#4682,.F.);
#6488=ORIENTED_EDGE('',*,*,#4858,.T.);
#6489=ORIENTED_EDGE('',*,*,#4693,.F.);
#6490=ORIENTED_EDGE('',*,*,#4859,.F.);
#6491=ORIENTED_EDGE('',*,*,#4687,.F.);
#6492=ORIENTED_EDGE('',*,*,#4859,.T.);
#6493=ORIENTED_EDGE('',*,*,#4692,.F.);
#6494=ORIENTED_EDGE('',*,*,#4860,.F.);
#6495=ORIENTED_EDGE('',*,*,#4471,.F.);
#6496=ORIENTED_EDGE('',*,*,#4860,.T.);
#6497=ORIENTED_EDGE('',*,*,#4691,.F.);
#6498=ORIENTED_EDGE('',*,*,#4861,.F.);
#6499=ORIENTED_EDGE('',*,*,#4652,.F.);
#6500=ORIENTED_EDGE('',*,*,#4861,.T.);
#6501=ORIENTED_EDGE('',*,*,#4705,.F.);
#6502=ORIENTED_EDGE('',*,*,#4862,.F.);
#6503=ORIENTED_EDGE('',*,*,#4653,.F.);
#6504=ORIENTED_EDGE('',*,*,#4862,.T.);
#6505=ORIENTED_EDGE('',*,*,#4684,.F.);
#6506=ORIENTED_EDGE('',*,*,#4863,.F.);
#6507=ORIENTED_EDGE('',*,*,#4654,.F.);
#6508=ORIENTED_EDGE('',*,*,#4863,.T.);
#6509=ORIENTED_EDGE('',*,*,#4704,.F.);
#6510=ORIENTED_EDGE('',*,*,#4864,.F.);
#6511=ORIENTED_EDGE('',*,*,#4646,.F.);
#6512=ORIENTED_EDGE('',*,*,#4864,.T.);
#6513=ORIENTED_EDGE('',*,*,#4700,.F.);
#6514=ORIENTED_EDGE('',*,*,#4865,.F.);
#6515=ORIENTED_EDGE('',*,*,#4647,.F.);
#6516=ORIENTED_EDGE('',*,*,#4865,.T.);
#6517=ORIENTED_EDGE('',*,*,#4699,.F.);
#6518=ORIENTED_EDGE('',*,*,#4866,.F.);
#6519=ORIENTED_EDGE('',*,*,#4469,.F.);
#6520=ORIENTED_EDGE('',*,*,#4866,.T.);
#6521=ORIENTED_EDGE('',*,*,#4698,.F.);
#6522=ORIENTED_EDGE('',*,*,#4867,.F.);
#6523=ORIENTED_EDGE('',*,*,#4655,.F.);
#6524=ORIENTED_EDGE('',*,*,#4867,.T.);
#6525=ORIENTED_EDGE('',*,*,#4697,.F.);
#6526=ORIENTED_EDGE('',*,*,#4868,.F.);
#6527=ORIENTED_EDGE('',*,*,#4702,.F.);
#6528=ORIENTED_EDGE('',*,*,#4868,.T.);
#6529=ORIENTED_EDGE('',*,*,#4696,.F.);
#6530=ORIENTED_EDGE('',*,*,#4665,.F.);
#6531=ORIENTED_EDGE('',*,*,#4659,.F.);
#6532=ORIENTED_EDGE('',*,*,#4869,.T.);
#6533=ORIENTED_EDGE('',*,*,#4853,.F.);
#6534=ORIENTED_EDGE('',*,*,#4734,.T.);
#6535=ORIENTED_EDGE('',*,*,#4499,.T.);
#6536=ORIENTED_EDGE('',*,*,#4591,.F.);
#6537=ORIENTED_EDGE('',*,*,#4537,.T.);
#6538=ORIENTED_EDGE('',*,*,#4619,.F.);
#6539=ORIENTED_EDGE('',*,*,#4631,.T.);
#6540=ORIENTED_EDGE('',*,*,#4556,.F.);
#6541=ORIENTED_EDGE('',*,*,#4632,.T.);
#6542=ORIENTED_EDGE('',*,*,#4634,.F.);
#6543=ORIENTED_EDGE('',*,*,#4870,.F.);
#6544=ORIENTED_EDGE('',*,*,#4554,.F.);
#6545=ORIENTED_EDGE('',*,*,#4870,.T.);
#6546=ORIENTED_EDGE('',*,*,#4496,.T.);
#6547=ORIENTED_EDGE('',*,*,#4709,.T.);
#6548=ORIENTED_EDGE('',*,*,#4852,.F.);
#6549=ORIENTED_EDGE('',*,*,#4869,.F.);
#6550=ORIENTED_EDGE('',*,*,#4555,.F.);
#6551=ORIENTED_EDGE('',*,*,#4478,.T.);
#6552=ORIENTED_EDGE('',*,*,#4871,.F.);
#6553=ORIENTED_EDGE('',*,*,#4476,.F.);
#6554=ORIENTED_EDGE('',*,*,#4588,.F.);
#6555=ORIENTED_EDGE('',*,*,#4477,.T.);
#6556=ORIENTED_EDGE('',*,*,#4871,.T.);
#6557=ORIENTED_EDGE('',*,*,#4488,.T.);
#6558=ORIENTED_EDGE('',*,*,#4711,.T.);
#6559=ORIENTED_EDGE('',*,*,#4490,.F.);
#6560=ORIENTED_EDGE('',*,*,#4589,.F.);
#6561=ORIENTED_EDGE('',*,*,#4492,.T.);
#6562=ORIENTED_EDGE('',*,*,#4710,.T.);
#6563=ORIENTED_EDGE('',*,*,#4494,.F.);
#6564=ORIENTED_EDGE('',*,*,#4551,.F.);
#6565=ORIENTED_EDGE('',*,*,#4620,.T.);
#6566=ORIENTED_EDGE('',*,*,#4602,.F.);
#6567=ORIENTED_EDGE('',*,*,#4527,.T.);
#6568=ORIENTED_EDGE('',*,*,#4600,.F.);
#6569=ORIENTED_EDGE('',*,*,#4521,.T.);
#6570=ORIENTED_EDGE('',*,*,#4718,.T.);
#6571=ORIENTED_EDGE('',*,*,#4872,.F.);
#6572=ORIENTED_EDGE('',*,*,#4578,.F.);
#6573=ORIENTED_EDGE('',*,*,#4873,.T.);
#6574=ORIENTED_EDGE('',*,*,#4716,.T.);
#6575=ORIENTED_EDGE('',*,*,#4523,.T.);
#6576=ORIENTED_EDGE('',*,*,#4738,.F.);
#6577=ORIENTED_EDGE('',*,*,#4706,.T.);
#6578=ORIENTED_EDGE('',*,*,#4739,.F.);
#6579=ORIENTED_EDGE('',*,*,#4675,.F.);
#6580=ORIENTED_EDGE('',*,*,#4579,.F.);
#6581=ORIENTED_EDGE('',*,*,#4872,.T.);
#6582=ORIENTED_EDGE('',*,*,#4717,.T.);
#6583=ORIENTED_EDGE('',*,*,#4873,.F.);
#6584=ORIENTED_EDGE('',*,*,#4674,.F.);
#6585=ORIENTED_EDGE('',*,*,#4874,.T.);
#6586=ORIENTED_EDGE('',*,*,#4719,.T.);
#6587=ORIENTED_EDGE('',*,*,#4519,.T.);
#6588=ORIENTED_EDGE('',*,*,#4601,.F.);
#6589=ORIENTED_EDGE('',*,*,#4529,.T.);
#6590=ORIENTED_EDGE('',*,*,#4604,.F.);
#6591=ORIENTED_EDGE('',*,*,#4621,.T.);
#6592=ORIENTED_EDGE('',*,*,#4576,.F.);
#6593=ORIENTED_EDGE('',*,*,#4622,.T.);
#6594=ORIENTED_EDGE('',*,*,#4605,.F.);
#6595=ORIENTED_EDGE('',*,*,#4531,.T.);
#6596=ORIENTED_EDGE('',*,*,#4598,.F.);
#6597=ORIENTED_EDGE('',*,*,#4517,.T.);
#6598=ORIENTED_EDGE('',*,*,#4721,.T.);
#6599=ORIENTED_EDGE('',*,*,#4875,.F.);
#6600=ORIENTED_EDGE('',*,*,#4574,.F.);
#6601=ORIENTED_EDGE('',*,*,#4875,.T.);
#6602=ORIENTED_EDGE('',*,*,#4720,.T.);
#6603=ORIENTED_EDGE('',*,*,#4874,.F.);
#6604=ORIENTED_EDGE('',*,*,#4575,.F.);
#6605=ORIENTED_EDGE('',*,*,#4876,.T.);
#6606=ORIENTED_EDGE('',*,*,#4722,.T.);
#6607=ORIENTED_EDGE('',*,*,#4515,.T.);
#6608=ORIENTED_EDGE('',*,*,#4599,.F.);
#6609=ORIENTED_EDGE('',*,*,#4533,.T.);
#6610=ORIENTED_EDGE('',*,*,#4607,.F.);
#6611=ORIENTED_EDGE('',*,*,#4623,.T.);
#6612=ORIENTED_EDGE('',*,*,#4572,.F.);
#6613=ORIENTED_EDGE('',*,*,#4624,.T.);
#6614=ORIENTED_EDGE('',*,*,#4608,.F.);
#6615=ORIENTED_EDGE('',*,*,#4547,.T.);
#6616=ORIENTED_EDGE('',*,*,#4596,.F.);
#6617=ORIENTED_EDGE('',*,*,#4513,.T.);
#6618=ORIENTED_EDGE('',*,*,#4724,.T.);
#6619=ORIENTED_EDGE('',*,*,#4877,.F.);
#6620=ORIENTED_EDGE('',*,*,#4570,.F.);
#6621=ORIENTED_EDGE('',*,*,#4877,.T.);
#6622=ORIENTED_EDGE('',*,*,#4723,.T.);
#6623=ORIENTED_EDGE('',*,*,#4876,.F.);
#6624=ORIENTED_EDGE('',*,*,#4571,.F.);
#6625=ORIENTED_EDGE('',*,*,#4878,.T.);
#6626=ORIENTED_EDGE('',*,*,#4725,.T.);
#6627=ORIENTED_EDGE('',*,*,#4511,.T.);
#6628=ORIENTED_EDGE('',*,*,#4597,.F.);
#6629=ORIENTED_EDGE('',*,*,#4549,.T.);
#6630=ORIENTED_EDGE('',*,*,#4610,.F.);
#6631=ORIENTED_EDGE('',*,*,#4625,.T.);
#6632=ORIENTED_EDGE('',*,*,#4568,.F.);
#6633=ORIENTED_EDGE('',*,*,#4626,.T.);
#6634=ORIENTED_EDGE('',*,*,#4611,.F.);
#6635=ORIENTED_EDGE('',*,*,#4543,.T.);
#6636=ORIENTED_EDGE('',*,*,#4594,.F.);
#6637=ORIENTED_EDGE('',*,*,#4509,.T.);
#6638=ORIENTED_EDGE('',*,*,#4727,.T.);
#6639=ORIENTED_EDGE('',*,*,#4879,.F.);
#6640=ORIENTED_EDGE('',*,*,#4566,.F.);
#6641=ORIENTED_EDGE('',*,*,#4879,.T.);
#6642=ORIENTED_EDGE('',*,*,#4726,.T.);
#6643=ORIENTED_EDGE('',*,*,#4878,.F.);
#6644=ORIENTED_EDGE('',*,*,#4567,.F.);
#6645=ORIENTED_EDGE('',*,*,#4880,.T.);
#6646=ORIENTED_EDGE('',*,*,#4728,.T.);
#6647=ORIENTED_EDGE('',*,*,#4507,.T.);
#6648=ORIENTED_EDGE('',*,*,#4595,.F.);
#6649=ORIENTED_EDGE('',*,*,#4545,.T.);
#6650=ORIENTED_EDGE('',*,*,#4613,.F.);
#6651=ORIENTED_EDGE('',*,*,#4627,.T.);
#6652=ORIENTED_EDGE('',*,*,#4564,.F.);
#6653=ORIENTED_EDGE('',*,*,#4628,.T.);
#6654=ORIENTED_EDGE('',*,*,#4614,.F.);
#6655=ORIENTED_EDGE('',*,*,#4539,.T.);
#6656=ORIENTED_EDGE('',*,*,#4592,.F.);
#6657=ORIENTED_EDGE('',*,*,#4505,.T.);
#6658=ORIENTED_EDGE('',*,*,#4730,.T.);
#6659=ORIENTED_EDGE('',*,*,#4881,.F.);
#6660=ORIENTED_EDGE('',*,*,#4562,.F.);
#6661=ORIENTED_EDGE('',*,*,#4881,.T.);
#6662=ORIENTED_EDGE('',*,*,#4729,.T.);
#6663=ORIENTED_EDGE('',*,*,#4880,.F.);
#6664=ORIENTED_EDGE('',*,*,#4563,.F.);
#6665=ORIENTED_EDGE('',*,*,#4882,.T.);
#6666=ORIENTED_EDGE('',*,*,#4731,.T.);
#6667=ORIENTED_EDGE('',*,*,#4503,.T.);
#6668=ORIENTED_EDGE('',*,*,#4593,.F.);
#6669=ORIENTED_EDGE('',*,*,#4541,.T.);
#6670=ORIENTED_EDGE('',*,*,#4616,.F.);
#6671=ORIENTED_EDGE('',*,*,#4629,.T.);
#6672=ORIENTED_EDGE('',*,*,#4560,.F.);
#6673=ORIENTED_EDGE('',*,*,#4630,.T.);
#6674=ORIENTED_EDGE('',*,*,#4617,.F.);
#6675=ORIENTED_EDGE('',*,*,#4535,.T.);
#6676=ORIENTED_EDGE('',*,*,#4590,.F.);
#6677=ORIENTED_EDGE('',*,*,#4501,.T.);
#6678=ORIENTED_EDGE('',*,*,#4733,.T.);
#6679=ORIENTED_EDGE('',*,*,#4883,.F.);
#6680=ORIENTED_EDGE('',*,*,#4558,.F.);
#6681=ORIENTED_EDGE('',*,*,#4883,.T.);
#6682=ORIENTED_EDGE('',*,*,#4732,.T.);
#6683=ORIENTED_EDGE('',*,*,#4882,.F.);
#6684=ORIENTED_EDGE('',*,*,#4559,.F.);
#6685=ORIENTED_EDGE('',*,*,#4737,.F.);
#6686=ORIENTED_EDGE('',*,*,#4525,.T.);
#6687=ORIENTED_EDGE('',*,*,#4715,.T.);
#6688=ORIENTED_EDGE('',*,*,#4884,.F.);
#6689=ORIENTED_EDGE('',*,*,#4662,.F.);
#6690=ORIENTED_EDGE('',*,*,#4884,.T.);
#6691=ORIENTED_EDGE('',*,*,#4714,.T.);
#6692=ORIENTED_EDGE('',*,*,#4663,.F.);
#6693=ORIENTED_EDGE('',*,*,#4763,.F.);
#6694=ORIENTED_EDGE('',*,*,#4885,.T.);
#6695=ORIENTED_EDGE('',*,*,#4430,.T.);
#6696=ORIENTED_EDGE('',*,*,#4886,.T.);
#6697=ORIENTED_EDGE('',*,*,#4797,.F.);
#6698=ORIENTED_EDGE('',*,*,#4456,.F.);
#6699=ORIENTED_EDGE('',*,*,#4887,.F.);
#6700=ORIENTED_EDGE('',*,*,#4760,.F.);
#6701=ORIENTED_EDGE('',*,*,#4887,.T.);
#6702=ORIENTED_EDGE('',*,*,#4451,.F.);
#6703=ORIENTED_EDGE('',*,*,#4888,.F.);
#6704=ORIENTED_EDGE('',*,*,#4761,.F.);
#6705=ORIENTED_EDGE('',*,*,#4888,.T.);
#6706=ORIENTED_EDGE('',*,*,#4644,.F.);
#6707=ORIENTED_EDGE('',*,*,#4889,.F.);
#6708=ORIENTED_EDGE('',*,*,#4762,.F.);
#6709=ORIENTED_EDGE('',*,*,#4889,.T.);
#6710=ORIENTED_EDGE('',*,*,#4643,.F.);
#6711=ORIENTED_EDGE('',*,*,#4890,.F.);
#6712=ORIENTED_EDGE('',*,*,#4885,.F.);
#6713=ORIENTED_EDGE('',*,*,#4467,.F.);
#6714=ORIENTED_EDGE('',*,*,#4431,.F.);
#6715=ORIENTED_EDGE('',*,*,#4890,.T.);
#6716=ORIENTED_EDGE('',*,*,#4642,.F.);
#6717=ORIENTED_EDGE('',*,*,#4648,.F.);
#6718=ORIENTED_EDGE('',*,*,#4651,.F.);
#6719=ORIENTED_EDGE('',*,*,#4742,.F.);
#6720=ORIENTED_EDGE('',*,*,#4891,.F.);
#6721=ORIENTED_EDGE('',*,*,#4429,.F.);
#6722=ORIENTED_EDGE('',*,*,#4473,.F.);
#6723=ORIENTED_EDGE('',*,*,#4891,.T.);
#6724=ORIENTED_EDGE('',*,*,#4741,.F.);
#6725=ORIENTED_EDGE('',*,*,#4892,.F.);
#6726=ORIENTED_EDGE('',*,*,#4886,.F.);
#6727=ORIENTED_EDGE('',*,*,#4892,.T.);
#6728=ORIENTED_EDGE('',*,*,#4740,.F.);
#6729=ORIENTED_EDGE('',*,*,#4893,.F.);
#6730=ORIENTED_EDGE('',*,*,#4764,.F.);
#6731=ORIENTED_EDGE('',*,*,#4893,.T.);
#6732=ORIENTED_EDGE('',*,*,#4447,.F.);
#6733=ORIENTED_EDGE('',*,*,#4894,.F.);
#6734=ORIENTED_EDGE('',*,*,#4765,.F.);
#6735=ORIENTED_EDGE('',*,*,#4769,.F.);
#6736=ORIENTED_EDGE('',*,*,#4766,.F.);
#6737=ORIENTED_EDGE('',*,*,#4894,.T.);
#6738=ORIENTED_EDGE('',*,*,#4458,.F.);
#6739=ORIENTED_EDGE('',*,*,#4895,.F.);
#6740=ORIENTED_EDGE('',*,*,#4896,.T.);
#6741=ORIENTED_EDGE('',*,*,#4897,.T.);
#6742=ORIENTED_EDGE('',*,*,#4898,.F.);
#6743=ORIENTED_EDGE('',*,*,#4899,.T.);
#6744=ORIENTED_EDGE('',*,*,#4895,.T.);
#6745=ORIENTED_EDGE('',*,*,#4900,.T.);
#6746=ORIENTED_EDGE('',*,*,#4901,.F.);
#6747=ORIENTED_EDGE('',*,*,#4902,.F.);
#6748=ORIENTED_EDGE('',*,*,#4903,.T.);
#6749=ORIENTED_EDGE('',*,*,#4898,.T.);
#6750=ORIENTED_EDGE('',*,*,#4904,.F.);
#6751=ORIENTED_EDGE('',*,*,#4905,.F.);
#6752=ORIENTED_EDGE('',*,*,#4906,.T.);
#6753=ORIENTED_EDGE('',*,*,#4902,.T.);
#6754=ORIENTED_EDGE('',*,*,#4907,.F.);
#6755=ORIENTED_EDGE('',*,*,#4908,.F.);
#6756=ORIENTED_EDGE('',*,*,#4909,.T.);
#6757=ORIENTED_EDGE('',*,*,#4905,.T.);
#6758=ORIENTED_EDGE('',*,*,#4910,.F.);
#6759=ORIENTED_EDGE('',*,*,#4911,.F.);
#6760=ORIENTED_EDGE('',*,*,#4912,.T.);
#6761=ORIENTED_EDGE('',*,*,#4908,.T.);
#6762=ORIENTED_EDGE('',*,*,#4913,.F.);
#6763=ORIENTED_EDGE('',*,*,#4914,.F.);
#6764=ORIENTED_EDGE('',*,*,#4915,.T.);
#6765=ORIENTED_EDGE('',*,*,#4911,.T.);
#6766=ORIENTED_EDGE('',*,*,#4916,.F.);
#6767=ORIENTED_EDGE('',*,*,#4917,.F.);
#6768=ORIENTED_EDGE('',*,*,#4918,.T.);
#6769=ORIENTED_EDGE('',*,*,#4914,.T.);
#6770=ORIENTED_EDGE('',*,*,#4919,.F.);
#6771=ORIENTED_EDGE('',*,*,#4920,.F.);
#6772=ORIENTED_EDGE('',*,*,#4921,.T.);
#6773=ORIENTED_EDGE('',*,*,#4917,.T.);
#6774=ORIENTED_EDGE('',*,*,#4922,.F.);
#6775=ORIENTED_EDGE('',*,*,#4923,.F.);
#6776=ORIENTED_EDGE('',*,*,#4924,.T.);
#6777=ORIENTED_EDGE('',*,*,#4920,.T.);
#6778=ORIENTED_EDGE('',*,*,#4925,.F.);
#6779=ORIENTED_EDGE('',*,*,#4926,.F.);
#6780=ORIENTED_EDGE('',*,*,#4927,.T.);
#6781=ORIENTED_EDGE('',*,*,#4923,.T.);
#6782=ORIENTED_EDGE('',*,*,#4928,.F.);
#6783=ORIENTED_EDGE('',*,*,#4929,.F.);
#6784=ORIENTED_EDGE('',*,*,#4930,.T.);
#6785=ORIENTED_EDGE('',*,*,#4926,.T.);
#6786=ORIENTED_EDGE('',*,*,#4931,.F.);
#6787=ORIENTED_EDGE('',*,*,#4932,.F.);
#6788=ORIENTED_EDGE('',*,*,#4933,.T.);
#6789=ORIENTED_EDGE('',*,*,#4929,.T.);
#6790=ORIENTED_EDGE('',*,*,#4934,.F.);
#6791=ORIENTED_EDGE('',*,*,#4935,.F.);
#6792=ORIENTED_EDGE('',*,*,#4936,.T.);
#6793=ORIENTED_EDGE('',*,*,#4932,.T.);
#6794=ORIENTED_EDGE('',*,*,#4937,.F.);
#6795=ORIENTED_EDGE('',*,*,#4938,.F.);
#6796=ORIENTED_EDGE('',*,*,#4939,.T.);
#6797=ORIENTED_EDGE('',*,*,#4935,.T.);
#6798=ORIENTED_EDGE('',*,*,#4940,.F.);
#6799=ORIENTED_EDGE('',*,*,#4941,.F.);
#6800=ORIENTED_EDGE('',*,*,#4942,.T.);
#6801=ORIENTED_EDGE('',*,*,#4938,.T.);
#6802=ORIENTED_EDGE('',*,*,#4943,.F.);
#6803=ORIENTED_EDGE('',*,*,#4944,.F.);
#6804=ORIENTED_EDGE('',*,*,#4945,.T.);
#6805=ORIENTED_EDGE('',*,*,#4941,.T.);
#6806=ORIENTED_EDGE('',*,*,#4946,.F.);
#6807=ORIENTED_EDGE('',*,*,#4947,.F.);
#6808=ORIENTED_EDGE('',*,*,#4948,.T.);
#6809=ORIENTED_EDGE('',*,*,#4944,.T.);
#6810=ORIENTED_EDGE('',*,*,#4949,.F.);
#6811=ORIENTED_EDGE('',*,*,#4950,.F.);
#6812=ORIENTED_EDGE('',*,*,#4951,.T.);
#6813=ORIENTED_EDGE('',*,*,#4947,.T.);
#6814=ORIENTED_EDGE('',*,*,#4952,.F.);
#6815=ORIENTED_EDGE('',*,*,#4953,.F.);
#6816=ORIENTED_EDGE('',*,*,#4954,.T.);
#6817=ORIENTED_EDGE('',*,*,#4950,.T.);
#6818=ORIENTED_EDGE('',*,*,#4955,.F.);
#6819=ORIENTED_EDGE('',*,*,#4956,.F.);
#6820=ORIENTED_EDGE('',*,*,#4957,.T.);
#6821=ORIENTED_EDGE('',*,*,#4953,.T.);
#6822=ORIENTED_EDGE('',*,*,#4958,.F.);
#6823=ORIENTED_EDGE('',*,*,#4959,.F.);
#6824=ORIENTED_EDGE('',*,*,#4960,.T.);
#6825=ORIENTED_EDGE('',*,*,#4956,.T.);
#6826=ORIENTED_EDGE('',*,*,#4961,.F.);
#6827=ORIENTED_EDGE('',*,*,#4962,.F.);
#6828=ORIENTED_EDGE('',*,*,#4963,.T.);
#6829=ORIENTED_EDGE('',*,*,#4959,.T.);
#6830=ORIENTED_EDGE('',*,*,#4964,.F.);
#6831=ORIENTED_EDGE('',*,*,#4965,.F.);
#6832=ORIENTED_EDGE('',*,*,#4966,.T.);
#6833=ORIENTED_EDGE('',*,*,#4962,.T.);
#6834=ORIENTED_EDGE('',*,*,#4967,.F.);
#6835=ORIENTED_EDGE('',*,*,#4968,.F.);
#6836=ORIENTED_EDGE('',*,*,#4969,.T.);
#6837=ORIENTED_EDGE('',*,*,#4965,.T.);
#6838=ORIENTED_EDGE('',*,*,#4970,.F.);
#6839=ORIENTED_EDGE('',*,*,#4971,.F.);
#6840=ORIENTED_EDGE('',*,*,#4972,.T.);
#6841=ORIENTED_EDGE('',*,*,#4968,.T.);
#6842=ORIENTED_EDGE('',*,*,#4973,.F.);
#6843=ORIENTED_EDGE('',*,*,#4974,.F.);
#6844=ORIENTED_EDGE('',*,*,#4975,.T.);
#6845=ORIENTED_EDGE('',*,*,#4971,.T.);
#6846=ORIENTED_EDGE('',*,*,#4976,.F.);
#6847=ORIENTED_EDGE('',*,*,#4977,.F.);
#6848=ORIENTED_EDGE('',*,*,#4978,.T.);
#6849=ORIENTED_EDGE('',*,*,#4974,.T.);
#6850=ORIENTED_EDGE('',*,*,#4979,.F.);
#6851=ORIENTED_EDGE('',*,*,#4980,.F.);
#6852=ORIENTED_EDGE('',*,*,#4981,.T.);
#6853=ORIENTED_EDGE('',*,*,#4977,.T.);
#6854=ORIENTED_EDGE('',*,*,#4982,.F.);
#6855=ORIENTED_EDGE('',*,*,#4983,.F.);
#6856=ORIENTED_EDGE('',*,*,#4984,.T.);
#6857=ORIENTED_EDGE('',*,*,#4980,.T.);
#6858=ORIENTED_EDGE('',*,*,#4985,.F.);
#6859=ORIENTED_EDGE('',*,*,#4986,.F.);
#6860=ORIENTED_EDGE('',*,*,#4987,.T.);
#6861=ORIENTED_EDGE('',*,*,#4983,.T.);
#6862=ORIENTED_EDGE('',*,*,#4988,.F.);
#6863=ORIENTED_EDGE('',*,*,#4989,.F.);
#6864=ORIENTED_EDGE('',*,*,#4990,.T.);
#6865=ORIENTED_EDGE('',*,*,#4986,.T.);
#6866=ORIENTED_EDGE('',*,*,#4991,.F.);
#6867=ORIENTED_EDGE('',*,*,#4992,.F.);
#6868=ORIENTED_EDGE('',*,*,#4993,.T.);
#6869=ORIENTED_EDGE('',*,*,#4989,.T.);
#6870=ORIENTED_EDGE('',*,*,#4994,.F.);
#6871=ORIENTED_EDGE('',*,*,#4995,.F.);
#6872=ORIENTED_EDGE('',*,*,#4996,.T.);
#6873=ORIENTED_EDGE('',*,*,#4992,.T.);
#6874=ORIENTED_EDGE('',*,*,#4997,.F.);
#6875=ORIENTED_EDGE('',*,*,#4998,.F.);
#6876=ORIENTED_EDGE('',*,*,#4999,.T.);
#6877=ORIENTED_EDGE('',*,*,#4995,.T.);
#6878=ORIENTED_EDGE('',*,*,#5000,.F.);
#6879=ORIENTED_EDGE('',*,*,#5001,.F.);
#6880=ORIENTED_EDGE('',*,*,#5002,.T.);
#6881=ORIENTED_EDGE('',*,*,#4998,.T.);
#6882=ORIENTED_EDGE('',*,*,#5003,.F.);
#6883=ORIENTED_EDGE('',*,*,#5004,.F.);
#6884=ORIENTED_EDGE('',*,*,#5005,.T.);
#6885=ORIENTED_EDGE('',*,*,#5001,.T.);
#6886=ORIENTED_EDGE('',*,*,#5006,.F.);
#6887=ORIENTED_EDGE('',*,*,#5007,.F.);
#6888=ORIENTED_EDGE('',*,*,#5008,.T.);
#6889=ORIENTED_EDGE('',*,*,#5004,.T.);
#6890=ORIENTED_EDGE('',*,*,#5009,.F.);
#6891=ORIENTED_EDGE('',*,*,#5010,.F.);
#6892=ORIENTED_EDGE('',*,*,#5011,.T.);
#6893=ORIENTED_EDGE('',*,*,#5007,.T.);
#6894=ORIENTED_EDGE('',*,*,#5012,.F.);
#6895=ORIENTED_EDGE('',*,*,#5013,.F.);
#6896=ORIENTED_EDGE('',*,*,#5014,.T.);
#6897=ORIENTED_EDGE('',*,*,#5010,.T.);
#6898=ORIENTED_EDGE('',*,*,#5015,.F.);
#6899=ORIENTED_EDGE('',*,*,#5016,.F.);
#6900=ORIENTED_EDGE('',*,*,#5017,.F.);
#6901=ORIENTED_EDGE('',*,*,#5018,.T.);
#6902=ORIENTED_EDGE('',*,*,#5013,.T.);
#6903=ORIENTED_EDGE('',*,*,#5019,.F.);
#6904=ORIENTED_EDGE('',*,*,#5020,.T.);
#6905=ORIENTED_EDGE('',*,*,#5017,.T.);
#6906=ORIENTED_EDGE('',*,*,#5021,.T.);
#6907=ORIENTED_EDGE('',*,*,#5022,.F.);
#6908=ORIENTED_EDGE('',*,*,#5021,.F.);
#6909=ORIENTED_EDGE('',*,*,#5023,.T.);
#6910=ORIENTED_EDGE('',*,*,#5024,.T.);
#6911=ORIENTED_EDGE('',*,*,#5025,.T.);
#6912=ORIENTED_EDGE('',*,*,#5026,.T.);
#6913=ORIENTED_EDGE('',*,*,#5027,.T.);
#6914=ORIENTED_EDGE('',*,*,#5028,.T.);
#6915=ORIENTED_EDGE('',*,*,#5029,.T.);
#6916=ORIENTED_EDGE('',*,*,#5030,.T.);
#6917=ORIENTED_EDGE('',*,*,#5031,.T.);
#6918=ORIENTED_EDGE('',*,*,#5032,.T.);
#6919=ORIENTED_EDGE('',*,*,#5033,.T.);
#6920=ORIENTED_EDGE('',*,*,#5034,.T.);
#6921=ORIENTED_EDGE('',*,*,#5035,.T.);
#6922=ORIENTED_EDGE('',*,*,#5036,.T.);
#6923=ORIENTED_EDGE('',*,*,#5037,.T.);
#6924=ORIENTED_EDGE('',*,*,#5038,.T.);
#6925=ORIENTED_EDGE('',*,*,#5039,.T.);
#6926=ORIENTED_EDGE('',*,*,#5040,.T.);
#6927=ORIENTED_EDGE('',*,*,#5041,.T.);
#6928=ORIENTED_EDGE('',*,*,#5042,.T.);
#6929=ORIENTED_EDGE('',*,*,#5043,.T.);
#6930=ORIENTED_EDGE('',*,*,#5044,.T.);
#6931=ORIENTED_EDGE('',*,*,#5045,.T.);
#6932=ORIENTED_EDGE('',*,*,#5046,.T.);
#6933=ORIENTED_EDGE('',*,*,#5047,.T.);
#6934=ORIENTED_EDGE('',*,*,#5048,.T.);
#6935=ORIENTED_EDGE('',*,*,#5049,.T.);
#6936=ORIENTED_EDGE('',*,*,#5050,.T.);
#6937=ORIENTED_EDGE('',*,*,#5051,.T.);
#6938=ORIENTED_EDGE('',*,*,#5052,.T.);
#6939=ORIENTED_EDGE('',*,*,#5053,.T.);
#6940=ORIENTED_EDGE('',*,*,#5054,.T.);
#6941=ORIENTED_EDGE('',*,*,#5055,.T.);
#6942=ORIENTED_EDGE('',*,*,#5056,.T.);
#6943=ORIENTED_EDGE('',*,*,#5057,.T.);
#6944=ORIENTED_EDGE('',*,*,#5058,.T.);
#6945=ORIENTED_EDGE('',*,*,#5059,.T.);
#6946=ORIENTED_EDGE('',*,*,#5060,.T.);
#6947=ORIENTED_EDGE('',*,*,#5061,.T.);
#6948=ORIENTED_EDGE('',*,*,#5062,.T.);
#6949=ORIENTED_EDGE('',*,*,#5063,.T.);
#6950=ORIENTED_EDGE('',*,*,#5064,.F.);
#6951=ORIENTED_EDGE('',*,*,#5065,.T.);
#6952=ORIENTED_EDGE('',*,*,#5066,.F.);
#6953=ORIENTED_EDGE('',*,*,#5067,.F.);
#6954=ORIENTED_EDGE('',*,*,#5068,.F.);
#6955=ORIENTED_EDGE('',*,*,#5069,.F.);
#6956=ORIENTED_EDGE('',*,*,#5070,.F.);
#6957=ORIENTED_EDGE('',*,*,#5071,.F.);
#6958=ORIENTED_EDGE('',*,*,#5072,.F.);
#6959=ORIENTED_EDGE('',*,*,#5073,.F.);
#6960=ORIENTED_EDGE('',*,*,#5074,.F.);
#6961=ORIENTED_EDGE('',*,*,#5075,.F.);
#6962=ORIENTED_EDGE('',*,*,#5076,.F.);
#6963=ORIENTED_EDGE('',*,*,#5077,.F.);
#6964=ORIENTED_EDGE('',*,*,#5078,.F.);
#6965=ORIENTED_EDGE('',*,*,#5079,.F.);
#6966=ORIENTED_EDGE('',*,*,#5080,.F.);
#6967=ORIENTED_EDGE('',*,*,#5081,.F.);
#6968=ORIENTED_EDGE('',*,*,#5082,.F.);
#6969=ORIENTED_EDGE('',*,*,#5024,.F.);
#6970=ORIENTED_EDGE('',*,*,#5083,.F.);
#6971=ORIENTED_EDGE('',*,*,#5028,.F.);
#6972=ORIENTED_EDGE('',*,*,#5084,.F.);
#6973=ORIENTED_EDGE('',*,*,#5032,.F.);
#6974=ORIENTED_EDGE('',*,*,#5085,.F.);
#6975=ORIENTED_EDGE('',*,*,#5036,.F.);
#6976=ORIENTED_EDGE('',*,*,#5086,.F.);
#6977=ORIENTED_EDGE('',*,*,#5040,.F.);
#6978=ORIENTED_EDGE('',*,*,#5087,.F.);
#6979=ORIENTED_EDGE('',*,*,#5044,.F.);
#6980=ORIENTED_EDGE('',*,*,#5088,.F.);
#6981=ORIENTED_EDGE('',*,*,#5048,.F.);
#6982=ORIENTED_EDGE('',*,*,#5089,.F.);
#6983=ORIENTED_EDGE('',*,*,#5052,.F.);
#6984=ORIENTED_EDGE('',*,*,#5090,.F.);
#6985=ORIENTED_EDGE('',*,*,#5056,.F.);
#6986=ORIENTED_EDGE('',*,*,#5091,.F.);
#6987=ORIENTED_EDGE('',*,*,#5060,.F.);
#6988=ORIENTED_EDGE('',*,*,#5092,.F.);
#6989=ORIENTED_EDGE('',*,*,#5093,.F.);
#6990=ORIENTED_EDGE('',*,*,#5094,.F.);
#6991=ORIENTED_EDGE('',*,*,#5095,.F.);
#6992=ORIENTED_EDGE('',*,*,#5096,.F.);
#6993=ORIENTED_EDGE('',*,*,#5097,.F.);
#6994=ORIENTED_EDGE('',*,*,#5098,.F.);
#6995=ORIENTED_EDGE('',*,*,#5099,.F.);
#6996=ORIENTED_EDGE('',*,*,#5100,.F.);
#6997=ORIENTED_EDGE('',*,*,#5101,.F.);
#6998=ORIENTED_EDGE('',*,*,#5102,.F.);
#6999=ORIENTED_EDGE('',*,*,#5103,.F.);
#7000=ORIENTED_EDGE('',*,*,#5104,.F.);
#7001=ORIENTED_EDGE('',*,*,#5105,.F.);
#7002=ORIENTED_EDGE('',*,*,#5106,.F.);
#7003=ORIENTED_EDGE('',*,*,#5107,.F.);
#7004=ORIENTED_EDGE('',*,*,#5108,.F.);
#7005=ORIENTED_EDGE('',*,*,#5065,.F.);
#7006=ORIENTED_EDGE('',*,*,#5109,.F.);
#7007=ORIENTED_EDGE('',*,*,#5110,.T.);
#7008=ORIENTED_EDGE('',*,*,#5111,.F.);
#7009=ORIENTED_EDGE('',*,*,#5042,.F.);
#7010=ORIENTED_EDGE('',*,*,#5112,.F.);
#7011=ORIENTED_EDGE('',*,*,#5038,.F.);
#7012=ORIENTED_EDGE('',*,*,#5113,.F.);
#7013=ORIENTED_EDGE('',*,*,#5034,.F.);
#7014=ORIENTED_EDGE('',*,*,#5114,.F.);
#7015=ORIENTED_EDGE('',*,*,#5030,.F.);
#7016=ORIENTED_EDGE('',*,*,#5115,.F.);
#7017=ORIENTED_EDGE('',*,*,#5026,.F.);
#7018=ORIENTED_EDGE('',*,*,#5116,.F.);
#7019=ORIENTED_EDGE('',*,*,#5117,.F.);
#7020=ORIENTED_EDGE('',*,*,#5118,.F.);
#7021=ORIENTED_EDGE('',*,*,#5119,.F.);
#7022=ORIENTED_EDGE('',*,*,#5120,.F.);
#7023=ORIENTED_EDGE('',*,*,#5121,.F.);
#7024=ORIENTED_EDGE('',*,*,#5122,.F.);
#7025=ORIENTED_EDGE('',*,*,#5123,.F.);
#7026=ORIENTED_EDGE('',*,*,#5124,.F.);
#7027=ORIENTED_EDGE('',*,*,#5125,.F.);
#7028=ORIENTED_EDGE('',*,*,#5126,.F.);
#7029=ORIENTED_EDGE('',*,*,#5127,.F.);
#7030=ORIENTED_EDGE('',*,*,#5128,.F.);
#7031=ORIENTED_EDGE('',*,*,#5129,.F.);
#7032=ORIENTED_EDGE('',*,*,#5130,.F.);
#7033=ORIENTED_EDGE('',*,*,#5131,.F.);
#7034=ORIENTED_EDGE('',*,*,#5132,.F.);
#7035=ORIENTED_EDGE('',*,*,#5133,.F.);
#7036=ORIENTED_EDGE('',*,*,#5134,.F.);
#7037=ORIENTED_EDGE('',*,*,#5135,.F.);
#7038=ORIENTED_EDGE('',*,*,#5136,.F.);
#7039=ORIENTED_EDGE('',*,*,#5137,.F.);
#7040=ORIENTED_EDGE('',*,*,#5138,.F.);
#7041=ORIENTED_EDGE('',*,*,#5139,.F.);
#7042=ORIENTED_EDGE('',*,*,#5140,.F.);
#7043=ORIENTED_EDGE('',*,*,#5141,.F.);
#7044=ORIENTED_EDGE('',*,*,#5142,.F.);
#7045=ORIENTED_EDGE('',*,*,#5143,.F.);
#7046=ORIENTED_EDGE('',*,*,#5144,.F.);
#7047=ORIENTED_EDGE('',*,*,#5145,.F.);
#7048=ORIENTED_EDGE('',*,*,#5146,.F.);
#7049=ORIENTED_EDGE('',*,*,#5147,.F.);
#7050=ORIENTED_EDGE('',*,*,#5148,.F.);
#7051=ORIENTED_EDGE('',*,*,#5062,.F.);
#7052=ORIENTED_EDGE('',*,*,#5149,.F.);
#7053=ORIENTED_EDGE('',*,*,#5058,.F.);
#7054=ORIENTED_EDGE('',*,*,#5150,.F.);
#7055=ORIENTED_EDGE('',*,*,#5054,.F.);
#7056=ORIENTED_EDGE('',*,*,#5151,.F.);
#7057=ORIENTED_EDGE('',*,*,#5050,.F.);
#7058=ORIENTED_EDGE('',*,*,#5152,.F.);
#7059=ORIENTED_EDGE('',*,*,#5046,.F.);
#7060=ORIENTED_EDGE('',*,*,#5153,.F.);
#7061=ORIENTED_EDGE('',*,*,#5110,.F.);
#7062=ORIENTED_EDGE('',*,*,#5016,.T.);
#7063=ORIENTED_EDGE('',*,*,#5154,.F.);
#7064=ORIENTED_EDGE('',*,*,#5023,.F.);
#7065=ORIENTED_EDGE('',*,*,#5111,.T.);
#7066=ORIENTED_EDGE('',*,*,#5153,.T.);
#7067=ORIENTED_EDGE('',*,*,#5045,.F.);
#7068=ORIENTED_EDGE('',*,*,#5087,.T.);
#7069=ORIENTED_EDGE('',*,*,#5043,.F.);
#7070=ORIENTED_EDGE('',*,*,#5155,.F.);
#7071=ORIENTED_EDGE('',*,*,#5116,.T.);
#7072=ORIENTED_EDGE('',*,*,#5025,.F.);
#7073=ORIENTED_EDGE('',*,*,#5082,.T.);
#7074=ORIENTED_EDGE('',*,*,#5027,.F.);
#7075=ORIENTED_EDGE('',*,*,#5115,.T.);
#7076=ORIENTED_EDGE('',*,*,#5029,.F.);
#7077=ORIENTED_EDGE('',*,*,#5083,.T.);
#7078=ORIENTED_EDGE('',*,*,#5031,.F.);
#7079=ORIENTED_EDGE('',*,*,#5114,.T.);
#7080=ORIENTED_EDGE('',*,*,#5033,.F.);
#7081=ORIENTED_EDGE('',*,*,#5084,.T.);
#7082=ORIENTED_EDGE('',*,*,#5035,.F.);
#7083=ORIENTED_EDGE('',*,*,#5113,.T.);
#7084=ORIENTED_EDGE('',*,*,#5037,.F.);
#7085=ORIENTED_EDGE('',*,*,#5085,.T.);
#7086=ORIENTED_EDGE('',*,*,#5039,.F.);
#7087=ORIENTED_EDGE('',*,*,#5112,.T.);
#7088=ORIENTED_EDGE('',*,*,#5041,.F.);
#7089=ORIENTED_EDGE('',*,*,#5086,.T.);
#7090=ORIENTED_EDGE('',*,*,#5047,.F.);
#7091=ORIENTED_EDGE('',*,*,#5152,.T.);
#7092=ORIENTED_EDGE('',*,*,#5049,.F.);
#7093=ORIENTED_EDGE('',*,*,#5088,.T.);
#7094=ORIENTED_EDGE('',*,*,#5051,.F.);
#7095=ORIENTED_EDGE('',*,*,#5151,.T.);
#7096=ORIENTED_EDGE('',*,*,#5053,.F.);
#7097=ORIENTED_EDGE('',*,*,#5089,.T.);
#7098=ORIENTED_EDGE('',*,*,#5055,.F.);
#7099=ORIENTED_EDGE('',*,*,#5150,.T.);
#7100=ORIENTED_EDGE('',*,*,#5057,.F.);
#7101=ORIENTED_EDGE('',*,*,#5090,.T.);
#7102=ORIENTED_EDGE('',*,*,#5059,.F.);
#7103=ORIENTED_EDGE('',*,*,#5149,.T.);
#7104=ORIENTED_EDGE('',*,*,#5061,.F.);
#7105=ORIENTED_EDGE('',*,*,#5091,.T.);
#7106=ORIENTED_EDGE('',*,*,#5063,.F.);
#7107=ORIENTED_EDGE('',*,*,#5148,.T.);
#7108=ORIENTED_EDGE('',*,*,#5156,.F.);
#7109=ORIENTED_EDGE('',*,*,#5092,.T.);
#7110=ORIENTED_EDGE('',*,*,#5157,.F.);
#7111=ORIENTED_EDGE('',*,*,#5146,.T.);
#7112=ORIENTED_EDGE('',*,*,#5158,.F.);
#7113=ORIENTED_EDGE('',*,*,#5094,.T.);
#7114=ORIENTED_EDGE('',*,*,#5159,.F.);
#7115=ORIENTED_EDGE('',*,*,#5144,.T.);
#7116=ORIENTED_EDGE('',*,*,#5160,.F.);
#7117=ORIENTED_EDGE('',*,*,#5096,.T.);
#7118=ORIENTED_EDGE('',*,*,#5161,.F.);
#7119=ORIENTED_EDGE('',*,*,#5142,.T.);
#7120=ORIENTED_EDGE('',*,*,#5162,.F.);
#7121=ORIENTED_EDGE('',*,*,#5098,.T.);
#7122=ORIENTED_EDGE('',*,*,#5163,.F.);
#7123=ORIENTED_EDGE('',*,*,#5140,.T.);
#7124=ORIENTED_EDGE('',*,*,#5164,.F.);
#7125=ORIENTED_EDGE('',*,*,#5100,.T.);
#7126=ORIENTED_EDGE('',*,*,#5165,.F.);
#7127=ORIENTED_EDGE('',*,*,#5138,.T.);
#7128=ORIENTED_EDGE('',*,*,#5166,.F.);
#7129=ORIENTED_EDGE('',*,*,#5102,.T.);
#7130=ORIENTED_EDGE('',*,*,#5167,.F.);
#7131=ORIENTED_EDGE('',*,*,#5136,.T.);
#7132=ORIENTED_EDGE('',*,*,#5168,.F.);
#7133=ORIENTED_EDGE('',*,*,#5104,.T.);
#7134=ORIENTED_EDGE('',*,*,#5169,.F.);
#7135=ORIENTED_EDGE('',*,*,#5134,.T.);
#7136=ORIENTED_EDGE('',*,*,#5170,.F.);
#7137=ORIENTED_EDGE('',*,*,#5106,.T.);
#7138=ORIENTED_EDGE('',*,*,#5171,.F.);
#7139=ORIENTED_EDGE('',*,*,#5132,.T.);
#7140=ORIENTED_EDGE('',*,*,#5172,.F.);
#7141=ORIENTED_EDGE('',*,*,#5066,.T.);
#7142=ORIENTED_EDGE('',*,*,#5108,.T.);
#7143=ORIENTED_EDGE('',*,*,#5173,.F.);
#7144=ORIENTED_EDGE('',*,*,#5130,.T.);
#7145=ORIENTED_EDGE('',*,*,#5174,.F.);
#7146=ORIENTED_EDGE('',*,*,#5068,.T.);
#7147=ORIENTED_EDGE('',*,*,#5175,.F.);
#7148=ORIENTED_EDGE('',*,*,#5128,.T.);
#7149=ORIENTED_EDGE('',*,*,#5176,.F.);
#7150=ORIENTED_EDGE('',*,*,#5070,.T.);
#7151=ORIENTED_EDGE('',*,*,#5177,.F.);
#7152=ORIENTED_EDGE('',*,*,#5126,.T.);
#7153=ORIENTED_EDGE('',*,*,#5178,.F.);
#7154=ORIENTED_EDGE('',*,*,#5072,.T.);
#7155=ORIENTED_EDGE('',*,*,#5179,.F.);
#7156=ORIENTED_EDGE('',*,*,#5124,.T.);
#7157=ORIENTED_EDGE('',*,*,#5180,.F.);
#7158=ORIENTED_EDGE('',*,*,#5074,.T.);
#7159=ORIENTED_EDGE('',*,*,#5181,.F.);
#7160=ORIENTED_EDGE('',*,*,#5122,.T.);
#7161=ORIENTED_EDGE('',*,*,#5182,.F.);
#7162=ORIENTED_EDGE('',*,*,#5076,.T.);
#7163=ORIENTED_EDGE('',*,*,#5183,.F.);
#7164=ORIENTED_EDGE('',*,*,#5120,.T.);
#7165=ORIENTED_EDGE('',*,*,#5184,.F.);
#7166=ORIENTED_EDGE('',*,*,#5078,.T.);
#7167=ORIENTED_EDGE('',*,*,#5064,.T.);
#7168=ORIENTED_EDGE('',*,*,#5185,.T.);
#7169=ORIENTED_EDGE('',*,*,#5186,.T.);
#7170=ORIENTED_EDGE('',*,*,#4900,.F.);
#7171=ORIENTED_EDGE('',*,*,#4897,.F.);
#7172=ORIENTED_EDGE('',*,*,#5187,.T.);
#7173=ORIENTED_EDGE('',*,*,#5109,.T.);
#7174=ORIENTED_EDGE('',*,*,#5188,.F.);
#7175=ORIENTED_EDGE('',*,*,#5080,.T.);
#7176=ORIENTED_EDGE('',*,*,#5189,.F.);
#7177=ORIENTED_EDGE('',*,*,#5118,.T.);
#7178=ORIENTED_EDGE('',*,*,#5190,.F.);
#7179=ORIENTED_EDGE('',*,*,#5020,.F.);
#7180=ORIENTED_EDGE('',*,*,#5191,.F.);
#7181=ORIENTED_EDGE('',*,*,#5192,.F.);
#7182=ORIENTED_EDGE('',*,*,#5193,.F.);
#7183=ORIENTED_EDGE('',*,*,#5191,.T.);
#7184=ORIENTED_EDGE('',*,*,#5154,.T.);
#7185=ORIENTED_EDGE('',*,*,#5019,.T.);
#7186=ORIENTED_EDGE('',*,*,#5015,.T.);
#7187=ORIENTED_EDGE('',*,*,#5012,.T.);
#7188=ORIENTED_EDGE('',*,*,#5009,.T.);
#7189=ORIENTED_EDGE('',*,*,#5006,.T.);
#7190=ORIENTED_EDGE('',*,*,#5003,.T.);
#7191=ORIENTED_EDGE('',*,*,#5000,.T.);
#7192=ORIENTED_EDGE('',*,*,#4997,.T.);
#7193=ORIENTED_EDGE('',*,*,#4994,.T.);
#7194=ORIENTED_EDGE('',*,*,#4991,.T.);
#7195=ORIENTED_EDGE('',*,*,#4988,.T.);
#7196=ORIENTED_EDGE('',*,*,#4985,.T.);
#7197=ORIENTED_EDGE('',*,*,#4982,.T.);
#7198=ORIENTED_EDGE('',*,*,#4979,.T.);
#7199=ORIENTED_EDGE('',*,*,#4976,.T.);
#7200=ORIENTED_EDGE('',*,*,#4973,.T.);
#7201=ORIENTED_EDGE('',*,*,#4970,.T.);
#7202=ORIENTED_EDGE('',*,*,#4967,.T.);
#7203=ORIENTED_EDGE('',*,*,#4964,.T.);
#7204=ORIENTED_EDGE('',*,*,#4961,.T.);
#7205=ORIENTED_EDGE('',*,*,#4958,.T.);
#7206=ORIENTED_EDGE('',*,*,#4955,.T.);
#7207=ORIENTED_EDGE('',*,*,#4952,.T.);
#7208=ORIENTED_EDGE('',*,*,#4949,.T.);
#7209=ORIENTED_EDGE('',*,*,#4946,.T.);
#7210=ORIENTED_EDGE('',*,*,#4943,.T.);
#7211=ORIENTED_EDGE('',*,*,#4940,.T.);
#7212=ORIENTED_EDGE('',*,*,#4937,.T.);
#7213=ORIENTED_EDGE('',*,*,#4934,.T.);
#7214=ORIENTED_EDGE('',*,*,#4931,.T.);
#7215=ORIENTED_EDGE('',*,*,#4928,.T.);
#7216=ORIENTED_EDGE('',*,*,#4925,.T.);
#7217=ORIENTED_EDGE('',*,*,#4922,.T.);
#7218=ORIENTED_EDGE('',*,*,#4919,.T.);
#7219=ORIENTED_EDGE('',*,*,#4916,.T.);
#7220=ORIENTED_EDGE('',*,*,#4913,.T.);
#7221=ORIENTED_EDGE('',*,*,#4910,.T.);
#7222=ORIENTED_EDGE('',*,*,#4907,.T.);
#7223=ORIENTED_EDGE('',*,*,#4904,.T.);
#7224=ORIENTED_EDGE('',*,*,#4901,.T.);
#7225=ORIENTED_EDGE('',*,*,#5186,.F.);
#7226=ORIENTED_EDGE('',*,*,#5018,.F.);
#7227=ORIENTED_EDGE('',*,*,#5190,.T.);
#7228=ORIENTED_EDGE('',*,*,#5194,.T.);
#7229=ORIENTED_EDGE('',*,*,#5187,.F.);
#7230=ORIENTED_EDGE('',*,*,#4896,.F.);
#7231=ORIENTED_EDGE('',*,*,#4899,.F.);
#7232=ORIENTED_EDGE('',*,*,#4903,.F.);
#7233=ORIENTED_EDGE('',*,*,#4906,.F.);
#7234=ORIENTED_EDGE('',*,*,#4909,.F.);
#7235=ORIENTED_EDGE('',*,*,#4912,.F.);
#7236=ORIENTED_EDGE('',*,*,#4915,.F.);
#7237=ORIENTED_EDGE('',*,*,#4918,.F.);
#7238=ORIENTED_EDGE('',*,*,#4921,.F.);
#7239=ORIENTED_EDGE('',*,*,#4924,.F.);
#7240=ORIENTED_EDGE('',*,*,#4927,.F.);
#7241=ORIENTED_EDGE('',*,*,#4930,.F.);
#7242=ORIENTED_EDGE('',*,*,#4933,.F.);
#7243=ORIENTED_EDGE('',*,*,#4936,.F.);
#7244=ORIENTED_EDGE('',*,*,#4939,.F.);
#7245=ORIENTED_EDGE('',*,*,#4942,.F.);
#7246=ORIENTED_EDGE('',*,*,#4945,.F.);
#7247=ORIENTED_EDGE('',*,*,#4948,.F.);
#7248=ORIENTED_EDGE('',*,*,#4951,.F.);
#7249=ORIENTED_EDGE('',*,*,#4954,.F.);
#7250=ORIENTED_EDGE('',*,*,#4957,.F.);
#7251=ORIENTED_EDGE('',*,*,#4960,.F.);
#7252=ORIENTED_EDGE('',*,*,#4963,.F.);
#7253=ORIENTED_EDGE('',*,*,#4966,.F.);
#7254=ORIENTED_EDGE('',*,*,#4969,.F.);
#7255=ORIENTED_EDGE('',*,*,#4972,.F.);
#7256=ORIENTED_EDGE('',*,*,#4975,.F.);
#7257=ORIENTED_EDGE('',*,*,#4978,.F.);
#7258=ORIENTED_EDGE('',*,*,#4981,.F.);
#7259=ORIENTED_EDGE('',*,*,#4984,.F.);
#7260=ORIENTED_EDGE('',*,*,#4987,.F.);
#7261=ORIENTED_EDGE('',*,*,#4990,.F.);
#7262=ORIENTED_EDGE('',*,*,#4993,.F.);
#7263=ORIENTED_EDGE('',*,*,#4996,.F.);
#7264=ORIENTED_EDGE('',*,*,#4999,.F.);
#7265=ORIENTED_EDGE('',*,*,#5002,.F.);
#7266=ORIENTED_EDGE('',*,*,#5005,.F.);
#7267=ORIENTED_EDGE('',*,*,#5008,.F.);
#7268=ORIENTED_EDGE('',*,*,#5011,.F.);
#7269=ORIENTED_EDGE('',*,*,#5014,.F.);
#7270=ORIENTED_EDGE('',*,*,#5194,.F.);
#7271=ORIENTED_EDGE('',*,*,#5192,.T.);
#7272=ORIENTED_EDGE('',*,*,#5193,.T.);
#7273=ORIENTED_EDGE('',*,*,#5185,.F.);
#7274=ORIENTED_EDGE('',*,*,#5119,.T.);
#7275=ORIENTED_EDGE('',*,*,#5189,.T.);
#7276=ORIENTED_EDGE('',*,*,#5079,.T.);
#7277=ORIENTED_EDGE('',*,*,#5184,.T.);
#7278=ORIENTED_EDGE('',*,*,#5121,.T.);
#7279=ORIENTED_EDGE('',*,*,#5183,.T.);
#7280=ORIENTED_EDGE('',*,*,#5077,.T.);
#7281=ORIENTED_EDGE('',*,*,#5182,.T.);
#7282=ORIENTED_EDGE('',*,*,#5123,.T.);
#7283=ORIENTED_EDGE('',*,*,#5181,.T.);
#7284=ORIENTED_EDGE('',*,*,#5075,.T.);
#7285=ORIENTED_EDGE('',*,*,#5180,.T.);
#7286=ORIENTED_EDGE('',*,*,#5125,.T.);
#7287=ORIENTED_EDGE('',*,*,#5179,.T.);
#7288=ORIENTED_EDGE('',*,*,#5073,.T.);
#7289=ORIENTED_EDGE('',*,*,#5178,.T.);
#7290=ORIENTED_EDGE('',*,*,#5127,.T.);
#7291=ORIENTED_EDGE('',*,*,#5177,.T.);
#7292=ORIENTED_EDGE('',*,*,#5071,.T.);
#7293=ORIENTED_EDGE('',*,*,#5176,.T.);
#7294=ORIENTED_EDGE('',*,*,#5129,.T.);
#7295=ORIENTED_EDGE('',*,*,#5175,.T.);
#7296=ORIENTED_EDGE('',*,*,#5069,.T.);
#7297=ORIENTED_EDGE('',*,*,#5174,.T.);
#7298=ORIENTED_EDGE('',*,*,#5131,.T.);
#7299=ORIENTED_EDGE('',*,*,#5173,.T.);
#7300=ORIENTED_EDGE('',*,*,#5067,.T.);
#7301=ORIENTED_EDGE('',*,*,#5172,.T.);
#7302=ORIENTED_EDGE('',*,*,#5133,.T.);
#7303=ORIENTED_EDGE('',*,*,#5171,.T.);
#7304=ORIENTED_EDGE('',*,*,#5107,.T.);
#7305=ORIENTED_EDGE('',*,*,#5170,.T.);
#7306=ORIENTED_EDGE('',*,*,#5135,.T.);
#7307=ORIENTED_EDGE('',*,*,#5169,.T.);
#7308=ORIENTED_EDGE('',*,*,#5105,.T.);
#7309=ORIENTED_EDGE('',*,*,#5168,.T.);
#7310=ORIENTED_EDGE('',*,*,#5137,.T.);
#7311=ORIENTED_EDGE('',*,*,#5167,.T.);
#7312=ORIENTED_EDGE('',*,*,#5103,.T.);
#7313=ORIENTED_EDGE('',*,*,#5166,.T.);
#7314=ORIENTED_EDGE('',*,*,#5139,.T.);
#7315=ORIENTED_EDGE('',*,*,#5165,.T.);
#7316=ORIENTED_EDGE('',*,*,#5101,.T.);
#7317=ORIENTED_EDGE('',*,*,#5164,.T.);
#7318=ORIENTED_EDGE('',*,*,#5141,.T.);
#7319=ORIENTED_EDGE('',*,*,#5163,.T.);
#7320=ORIENTED_EDGE('',*,*,#5099,.T.);
#7321=ORIENTED_EDGE('',*,*,#5162,.T.);
#7322=ORIENTED_EDGE('',*,*,#5143,.T.);
#7323=ORIENTED_EDGE('',*,*,#5161,.T.);
#7324=ORIENTED_EDGE('',*,*,#5097,.T.);
#7325=ORIENTED_EDGE('',*,*,#5160,.T.);
#7326=ORIENTED_EDGE('',*,*,#5145,.T.);
#7327=ORIENTED_EDGE('',*,*,#5159,.T.);
#7328=ORIENTED_EDGE('',*,*,#5095,.T.);
#7329=ORIENTED_EDGE('',*,*,#5158,.T.);
#7330=ORIENTED_EDGE('',*,*,#5147,.T.);
#7331=ORIENTED_EDGE('',*,*,#5157,.T.);
#7332=ORIENTED_EDGE('',*,*,#5093,.T.);
#7333=ORIENTED_EDGE('',*,*,#5156,.T.);
#7334=ORIENTED_EDGE('',*,*,#5117,.T.);
#7335=ORIENTED_EDGE('',*,*,#5155,.T.);
#7336=ORIENTED_EDGE('',*,*,#5081,.T.);
#7337=ORIENTED_EDGE('',*,*,#5188,.T.);
#7338=ORIENTED_EDGE('',*,*,#5022,.T.);
#7339=ORIENTED_EDGE('',*,*,#5195,.T.);
#7340=ORIENTED_EDGE('',*,*,#5196,.T.);
#7341=ORIENTED_EDGE('',*,*,#5197,.F.);
#7342=ORIENTED_EDGE('',*,*,#5198,.T.);
#7343=ORIENTED_EDGE('',*,*,#5195,.F.);
#7344=ORIENTED_EDGE('',*,*,#5196,.F.);
#7345=ORIENTED_EDGE('',*,*,#5198,.F.);
#7346=ORIENTED_EDGE('',*,*,#5197,.T.);
#7347=ORIENTED_EDGE('',*,*,#5199,.F.);
#7348=ORIENTED_EDGE('',*,*,#5200,.F.);
#7349=ORIENTED_EDGE('',*,*,#5201,.F.);
#7350=ORIENTED_EDGE('',*,*,#5202,.T.);
#7351=ORIENTED_EDGE('',*,*,#5203,.F.);
#7352=ORIENTED_EDGE('',*,*,#5204,.F.);
#7353=ORIENTED_EDGE('',*,*,#5205,.F.);
#7354=ORIENTED_EDGE('',*,*,#5206,.T.);
#7355=ORIENTED_EDGE('',*,*,#5207,.T.);
#7356=ORIENTED_EDGE('',*,*,#5208,.T.);
#7357=ORIENTED_EDGE('',*,*,#5209,.F.);
#7358=ORIENTED_EDGE('',*,*,#5208,.F.);
#7359=ORIENTED_EDGE('',*,*,#5210,.T.);
#7360=ORIENTED_EDGE('',*,*,#5211,.T.);
#7361=ORIENTED_EDGE('',*,*,#5212,.T.);
#7362=ORIENTED_EDGE('',*,*,#5211,.F.);
#7363=ORIENTED_EDGE('',*,*,#5213,.T.);
#7364=ORIENTED_EDGE('',*,*,#5214,.T.);
#7365=ORIENTED_EDGE('',*,*,#5215,.T.);
#7366=ORIENTED_EDGE('',*,*,#5214,.F.);
#7367=ORIENTED_EDGE('',*,*,#5216,.F.);
#7368=ORIENTED_EDGE('',*,*,#5217,.T.);
#7369=ORIENTED_EDGE('',*,*,#5218,.F.);
#7370=ORIENTED_EDGE('',*,*,#5219,.T.);
#7371=ORIENTED_EDGE('',*,*,#5220,.F.);
#7372=ORIENTED_EDGE('',*,*,#5221,.T.);
#7373=ORIENTED_EDGE('',*,*,#5222,.F.);
#7374=ORIENTED_EDGE('',*,*,#5223,.T.);
#7375=ORIENTED_EDGE('',*,*,#5224,.F.);
#7376=ORIENTED_EDGE('',*,*,#5225,.T.);
#7377=ORIENTED_EDGE('',*,*,#5226,.T.);
#7378=ORIENTED_EDGE('',*,*,#5227,.F.);
#7379=ORIENTED_EDGE('',*,*,#5201,.T.);
#7380=ORIENTED_EDGE('',*,*,#5228,.T.);
#7381=ORIENTED_EDGE('',*,*,#5203,.T.);
#7382=ORIENTED_EDGE('',*,*,#5229,.F.);
#7383=ORIENTED_EDGE('',*,*,#5230,.T.);
#7384=ORIENTED_EDGE('',*,*,#5231,.T.);
#7385=ORIENTED_EDGE('',*,*,#5232,.F.);
#7386=ORIENTED_EDGE('',*,*,#5233,.T.);
#7387=ORIENTED_EDGE('',*,*,#5234,.F.);
#7388=ORIENTED_EDGE('',*,*,#5235,.T.);
#7389=ORIENTED_EDGE('',*,*,#5236,.T.);
#7390=ORIENTED_EDGE('',*,*,#5237,.T.);
#7391=ORIENTED_EDGE('',*,*,#5238,.T.);
#7392=ORIENTED_EDGE('',*,*,#5239,.T.);
#7393=ORIENTED_EDGE('',*,*,#5240,.T.);
#7394=ORIENTED_EDGE('',*,*,#5241,.T.);
#7395=ORIENTED_EDGE('',*,*,#5242,.T.);
#7396=ORIENTED_EDGE('',*,*,#5243,.T.);
#7397=ORIENTED_EDGE('',*,*,#5244,.T.);
#7398=ORIENTED_EDGE('',*,*,#5245,.T.);
#7399=ORIENTED_EDGE('',*,*,#5246,.F.);
#7400=ORIENTED_EDGE('',*,*,#5247,.T.);
#7401=ORIENTED_EDGE('',*,*,#5248,.F.);
#7402=ORIENTED_EDGE('',*,*,#5249,.T.);
#7403=ORIENTED_EDGE('',*,*,#5250,.F.);
#7404=ORIENTED_EDGE('',*,*,#5251,.F.);
#7405=ORIENTED_EDGE('',*,*,#5252,.T.);
#7406=ORIENTED_EDGE('',*,*,#5253,.T.);
#7407=ORIENTED_EDGE('',*,*,#5254,.T.);
#7408=ORIENTED_EDGE('',*,*,#5255,.T.);
#7409=ORIENTED_EDGE('',*,*,#5220,.T.);
#7410=ORIENTED_EDGE('',*,*,#5256,.T.);
#7411=ORIENTED_EDGE('',*,*,#5257,.T.);
#7412=ORIENTED_EDGE('',*,*,#5199,.T.);
#7413=ORIENTED_EDGE('',*,*,#5258,.T.);
#7414=ORIENTED_EDGE('',*,*,#5259,.T.);
#7415=ORIENTED_EDGE('',*,*,#5260,.T.);
#7416=ORIENTED_EDGE('',*,*,#5261,.T.);
#7417=ORIENTED_EDGE('',*,*,#5212,.F.);
#7418=ORIENTED_EDGE('',*,*,#5215,.F.);
#7419=ORIENTED_EDGE('',*,*,#5262,.T.);
#7420=ORIENTED_EDGE('',*,*,#5263,.T.);
#7421=ORIENTED_EDGE('',*,*,#5264,.T.);
#7422=ORIENTED_EDGE('',*,*,#5265,.T.);
#7423=ORIENTED_EDGE('',*,*,#5266,.T.);
#7424=ORIENTED_EDGE('',*,*,#5205,.T.);
#7425=ORIENTED_EDGE('',*,*,#5267,.T.);
#7426=ORIENTED_EDGE('',*,*,#5268,.T.);
#7427=ORIENTED_EDGE('',*,*,#5218,.T.);
#7428=ORIENTED_EDGE('',*,*,#5269,.T.);
#7429=ORIENTED_EDGE('',*,*,#5270,.T.);
#7430=ORIENTED_EDGE('',*,*,#5271,.T.);
#7431=ORIENTED_EDGE('',*,*,#5210,.F.);
#7432=ORIENTED_EDGE('',*,*,#5213,.F.);
#7433=ORIENTED_EDGE('',*,*,#5229,.T.);
#7434=ORIENTED_EDGE('',*,*,#5272,.T.);
#7435=ORIENTED_EDGE('',*,*,#5248,.T.);
#7436=ORIENTED_EDGE('',*,*,#5273,.T.);
#7437=ORIENTED_EDGE('',*,*,#5274,.F.);
#7438=ORIENTED_EDGE('',*,*,#5275,.F.);
#7439=ORIENTED_EDGE('',*,*,#5276,.T.);
#7440=ORIENTED_EDGE('',*,*,#5277,.T.);
#7441=ORIENTED_EDGE('',*,*,#5278,.T.);
#7442=ORIENTED_EDGE('',*,*,#5279,.T.);
#7443=ORIENTED_EDGE('',*,*,#5280,.T.);
#7444=ORIENTED_EDGE('',*,*,#5281,.T.);
#7445=ORIENTED_EDGE('',*,*,#5282,.T.);
#7446=ORIENTED_EDGE('',*,*,#5283,.F.);
#7447=ORIENTED_EDGE('',*,*,#5284,.F.);
#7448=ORIENTED_EDGE('',*,*,#5250,.T.);
#7449=ORIENTED_EDGE('',*,*,#5285,.F.);
#7450=ORIENTED_EDGE('',*,*,#5286,.T.);
#7451=ORIENTED_EDGE('',*,*,#5287,.T.);
#7452=ORIENTED_EDGE('',*,*,#5288,.T.);
#7453=ORIENTED_EDGE('',*,*,#5238,.F.);
#7454=ORIENTED_EDGE('',*,*,#5289,.T.);
#7455=ORIENTED_EDGE('',*,*,#5285,.T.);
#7456=ORIENTED_EDGE('',*,*,#5290,.T.);
#7457=ORIENTED_EDGE('',*,*,#5227,.T.);
#7458=ORIENTED_EDGE('',*,*,#5291,.T.);
#7459=ORIENTED_EDGE('',*,*,#5292,.F.);
#7460=ORIENTED_EDGE('',*,*,#5293,.F.);
#7461=ORIENTED_EDGE('',*,*,#5294,.T.);
#7462=ORIENTED_EDGE('',*,*,#5295,.T.);
#7463=ORIENTED_EDGE('',*,*,#5296,.T.);
#7464=ORIENTED_EDGE('',*,*,#5297,.T.);
#7465=ORIENTED_EDGE('',*,*,#5298,.F.);
#7466=ORIENTED_EDGE('',*,*,#5299,.T.);
#7467=ORIENTED_EDGE('',*,*,#5300,.T.);
#7468=ORIENTED_EDGE('',*,*,#5301,.T.);
#7469=ORIENTED_EDGE('',*,*,#5302,.F.);
#7470=ORIENTED_EDGE('',*,*,#5292,.T.);
#7471=ORIENTED_EDGE('',*,*,#5228,.F.);
#7472=ORIENTED_EDGE('',*,*,#5303,.T.);
#7473=ORIENTED_EDGE('',*,*,#5298,.T.);
#7474=ORIENTED_EDGE('',*,*,#5304,.T.);
#7475=ORIENTED_EDGE('',*,*,#5242,.F.);
#7476=ORIENTED_EDGE('',*,*,#5305,.T.);
#7477=ORIENTED_EDGE('',*,*,#5306,.T.);
#7478=ORIENTED_EDGE('',*,*,#5307,.F.);
#7479=ORIENTED_EDGE('',*,*,#5308,.F.);
#7480=ORIENTED_EDGE('',*,*,#5309,.T.);
#7481=ORIENTED_EDGE('',*,*,#5310,.F.);
#7482=ORIENTED_EDGE('',*,*,#5291,.F.);
#7483=ORIENTED_EDGE('',*,*,#5226,.F.);
#7484=ORIENTED_EDGE('',*,*,#5311,.T.);
#7485=ORIENTED_EDGE('',*,*,#5312,.T.);
#7486=ORIENTED_EDGE('',*,*,#5313,.T.);
#7487=ORIENTED_EDGE('',*,*,#5314,.T.);
#7488=ORIENTED_EDGE('',*,*,#5315,.T.);
#7489=ORIENTED_EDGE('',*,*,#5316,.T.);
#7490=ORIENTED_EDGE('',*,*,#5317,.T.);
#7491=ORIENTED_EDGE('',*,*,#5318,.T.);
#7492=ORIENTED_EDGE('',*,*,#5319,.T.);
#7493=ORIENTED_EDGE('',*,*,#5320,.T.);
#7494=ORIENTED_EDGE('',*,*,#5321,.T.);
#7495=ORIENTED_EDGE('',*,*,#5322,.T.);
#7496=ORIENTED_EDGE('',*,*,#5323,.T.);
#7497=ORIENTED_EDGE('',*,*,#5324,.T.);
#7498=ORIENTED_EDGE('',*,*,#5244,.F.);
#7499=ORIENTED_EDGE('',*,*,#5325,.T.);
#7500=ORIENTED_EDGE('',*,*,#5326,.T.);
#7501=ORIENTED_EDGE('',*,*,#5230,.F.);
#7502=ORIENTED_EDGE('',*,*,#5327,.T.);
#7503=ORIENTED_EDGE('',*,*,#5328,.T.);
#7504=ORIENTED_EDGE('',*,*,#5329,.F.);
#7505=ORIENTED_EDGE('',*,*,#5330,.T.);
#7506=ORIENTED_EDGE('',*,*,#5331,.T.);
#7507=ORIENTED_EDGE('',*,*,#5307,.T.);
#7508=ORIENTED_EDGE('',*,*,#5216,.T.);
#7509=ORIENTED_EDGE('',*,*,#5332,.T.);
#7510=ORIENTED_EDGE('',*,*,#5308,.T.);
#7511=ORIENTED_EDGE('',*,*,#5331,.F.);
#7512=ORIENTED_EDGE('',*,*,#5310,.T.);
#7513=ORIENTED_EDGE('',*,*,#5333,.T.);
#7514=ORIENTED_EDGE('',*,*,#5294,.F.);
#7515=ORIENTED_EDGE('',*,*,#5306,.F.);
#7516=ORIENTED_EDGE('',*,*,#5334,.T.);
#7517=ORIENTED_EDGE('',*,*,#5335,.T.);
#7518=ORIENTED_EDGE('',*,*,#5329,.T.);
#7519=ORIENTED_EDGE('',*,*,#5336,.T.);
#7520=ORIENTED_EDGE('',*,*,#5337,.T.);
#7521=ORIENTED_EDGE('',*,*,#5338,.T.);
#7522=ORIENTED_EDGE('',*,*,#5339,.T.);
#7523=ORIENTED_EDGE('',*,*,#5302,.T.);
#7524=ORIENTED_EDGE('',*,*,#5340,.T.);
#7525=ORIENTED_EDGE('',*,*,#5341,.F.);
#7526=ORIENTED_EDGE('',*,*,#5342,.F.);
#7527=ORIENTED_EDGE('',*,*,#5343,.T.);
#7528=ORIENTED_EDGE('',*,*,#5222,.T.);
#7529=ORIENTED_EDGE('',*,*,#5344,.F.);
#7530=ORIENTED_EDGE('',*,*,#5344,.T.);
#7531=ORIENTED_EDGE('',*,*,#5345,.T.);
#7532=ORIENTED_EDGE('',*,*,#5339,.F.);
#7533=ORIENTED_EDGE('',*,*,#5346,.F.);
#7534=ORIENTED_EDGE('',*,*,#5338,.F.);
#7535=ORIENTED_EDGE('',*,*,#5347,.T.);
#7536=ORIENTED_EDGE('',*,*,#5234,.T.);
#7537=ORIENTED_EDGE('',*,*,#5348,.F.);
#7538=ORIENTED_EDGE('',*,*,#5349,.F.);
#7539=ORIENTED_EDGE('',*,*,#5232,.T.);
#7540=ORIENTED_EDGE('',*,*,#5350,.F.);
#7541=ORIENTED_EDGE('',*,*,#5351,.F.);
#7542=ORIENTED_EDGE('',*,*,#5246,.T.);
#7543=ORIENTED_EDGE('',*,*,#5352,.F.);
#7544=ORIENTED_EDGE('',*,*,#5353,.F.);
#7545=ORIENTED_EDGE('',*,*,#5354,.F.);
#7546=ORIENTED_EDGE('',*,*,#5355,.F.);
#7547=ORIENTED_EDGE('',*,*,#5356,.F.);
#7548=ORIENTED_EDGE('',*,*,#5357,.F.);
#7549=ORIENTED_EDGE('',*,*,#5358,.F.);
#7550=ORIENTED_EDGE('',*,*,#5359,.F.);
#7551=ORIENTED_EDGE('',*,*,#5360,.F.);
#7552=ORIENTED_EDGE('',*,*,#5361,.F.);
#7553=ORIENTED_EDGE('',*,*,#5362,.F.);
#7554=ORIENTED_EDGE('',*,*,#5363,.F.);
#7555=ORIENTED_EDGE('',*,*,#5364,.F.);
#7556=ORIENTED_EDGE('',*,*,#5365,.F.);
#7557=ORIENTED_EDGE('',*,*,#5224,.T.);
#7558=ORIENTED_EDGE('',*,*,#5293,.T.);
#7559=ORIENTED_EDGE('',*,*,#5341,.T.);
#7560=ORIENTED_EDGE('',*,*,#5366,.T.);
#7561=ORIENTED_EDGE('',*,*,#5342,.T.);
#7562=ORIENTED_EDGE('',*,*,#5346,.T.);
#7563=ORIENTED_EDGE('',*,*,#5254,.F.);
#7564=ORIENTED_EDGE('',*,*,#5367,.T.);
#7565=ORIENTED_EDGE('',*,*,#5336,.F.);
#7566=ORIENTED_EDGE('',*,*,#5368,.F.);
#7567=ORIENTED_EDGE('',*,*,#5368,.T.);
#7568=ORIENTED_EDGE('',*,*,#5345,.F.);
#7569=ORIENTED_EDGE('',*,*,#5221,.F.);
#7570=ORIENTED_EDGE('',*,*,#5255,.F.);
#7571=ORIENTED_EDGE('',*,*,#5335,.F.);
#7572=ORIENTED_EDGE('',*,*,#5369,.T.);
#7573=ORIENTED_EDGE('',*,*,#5270,.F.);
#7574=ORIENTED_EDGE('',*,*,#5370,.F.);
#7575=ORIENTED_EDGE('',*,*,#5370,.T.);
#7576=ORIENTED_EDGE('',*,*,#5269,.F.);
#7577=ORIENTED_EDGE('',*,*,#5217,.F.);
#7578=ORIENTED_EDGE('',*,*,#5330,.F.);
#7579=ORIENTED_EDGE('',*,*,#5281,.F.);
#7580=ORIENTED_EDGE('',*,*,#5371,.T.);
#7581=ORIENTED_EDGE('',*,*,#5276,.F.);
#7582=ORIENTED_EDGE('',*,*,#5372,.T.);
#7583=ORIENTED_EDGE('',*,*,#5373,.T.);
#7584=ORIENTED_EDGE('',*,*,#5283,.T.);
#7585=ORIENTED_EDGE('',*,*,#5374,.F.);
#7586=ORIENTED_EDGE('',*,*,#5375,.T.);
#7587=ORIENTED_EDGE('',*,*,#5282,.F.);
#7588=ORIENTED_EDGE('',*,*,#5372,.F.);
#7589=ORIENTED_EDGE('',*,*,#5275,.T.);
#7590=ORIENTED_EDGE('',*,*,#5376,.T.);
#7591=ORIENTED_EDGE('',*,*,#5377,.T.);
#7592=ORIENTED_EDGE('',*,*,#5374,.T.);
#7593=ORIENTED_EDGE('',*,*,#5207,.F.);
#7594=ORIENTED_EDGE('',*,*,#5251,.T.);
#7595=ORIENTED_EDGE('',*,*,#5284,.T.);
#7596=ORIENTED_EDGE('',*,*,#5373,.F.);
#7597=ORIENTED_EDGE('',*,*,#5378,.F.);
#7598=ORIENTED_EDGE('',*,*,#5379,.F.);
#7599=ORIENTED_EDGE('',*,*,#5273,.F.);
#7600=ORIENTED_EDGE('',*,*,#5209,.T.);
#7601=ORIENTED_EDGE('',*,*,#5378,.T.);
#7602=ORIENTED_EDGE('',*,*,#5375,.F.);
#7603=ORIENTED_EDGE('',*,*,#5377,.F.);
#7604=ORIENTED_EDGE('',*,*,#5380,.T.);
#7605=ORIENTED_EDGE('',*,*,#5379,.T.);
#7606=ORIENTED_EDGE('',*,*,#5380,.F.);
#7607=ORIENTED_EDGE('',*,*,#5376,.F.);
#7608=ORIENTED_EDGE('',*,*,#5274,.T.);
#7609=ORIENTED_EDGE('',*,*,#5364,.T.);
#7610=ORIENTED_EDGE('',*,*,#5381,.T.);
#7611=ORIENTED_EDGE('',*,*,#5312,.F.);
#7612=ORIENTED_EDGE('',*,*,#5382,.T.);
#7613=ORIENTED_EDGE('',*,*,#5365,.T.);
#7614=ORIENTED_EDGE('',*,*,#5382,.F.);
#7615=ORIENTED_EDGE('',*,*,#5311,.F.);
#7616=ORIENTED_EDGE('',*,*,#5225,.F.);
#7617=ORIENTED_EDGE('',*,*,#5363,.T.);
#7618=ORIENTED_EDGE('',*,*,#5383,.F.);
#7619=ORIENTED_EDGE('',*,*,#5313,.F.);
#7620=ORIENTED_EDGE('',*,*,#5381,.F.);
#7621=ORIENTED_EDGE('',*,*,#5361,.T.);
#7622=ORIENTED_EDGE('',*,*,#5384,.F.);
#7623=ORIENTED_EDGE('',*,*,#5315,.F.);
#7624=ORIENTED_EDGE('',*,*,#5385,.F.);
#7625=ORIENTED_EDGE('',*,*,#5359,.T.);
#7626=ORIENTED_EDGE('',*,*,#5386,.F.);
#7627=ORIENTED_EDGE('',*,*,#5317,.F.);
#7628=ORIENTED_EDGE('',*,*,#5387,.F.);
#7629=ORIENTED_EDGE('',*,*,#5357,.T.);
#7630=ORIENTED_EDGE('',*,*,#5388,.F.);
#7631=ORIENTED_EDGE('',*,*,#5319,.F.);
#7632=ORIENTED_EDGE('',*,*,#5389,.F.);
#7633=ORIENTED_EDGE('',*,*,#5355,.T.);
#7634=ORIENTED_EDGE('',*,*,#5390,.F.);
#7635=ORIENTED_EDGE('',*,*,#5321,.F.);
#7636=ORIENTED_EDGE('',*,*,#5391,.F.);
#7637=ORIENTED_EDGE('',*,*,#5353,.T.);
#7638=ORIENTED_EDGE('',*,*,#5392,.F.);
#7639=ORIENTED_EDGE('',*,*,#5323,.F.);
#7640=ORIENTED_EDGE('',*,*,#5393,.F.);
#7641=ORIENTED_EDGE('',*,*,#5324,.F.);
#7642=ORIENTED_EDGE('',*,*,#5392,.T.);
#7643=ORIENTED_EDGE('',*,*,#5352,.T.);
#7644=ORIENTED_EDGE('',*,*,#5245,.F.);
#7645=ORIENTED_EDGE('',*,*,#5393,.T.);
#7646=ORIENTED_EDGE('',*,*,#5322,.F.);
#7647=ORIENTED_EDGE('',*,*,#5390,.T.);
#7648=ORIENTED_EDGE('',*,*,#5354,.T.);
#7649=ORIENTED_EDGE('',*,*,#5391,.T.);
#7650=ORIENTED_EDGE('',*,*,#5320,.F.);
#7651=ORIENTED_EDGE('',*,*,#5388,.T.);
#7652=ORIENTED_EDGE('',*,*,#5356,.T.);
#7653=ORIENTED_EDGE('',*,*,#5389,.T.);
#7654=ORIENTED_EDGE('',*,*,#5318,.F.);
#7655=ORIENTED_EDGE('',*,*,#5386,.T.);
#7656=ORIENTED_EDGE('',*,*,#5358,.T.);
#7657=ORIENTED_EDGE('',*,*,#5387,.T.);
#7658=ORIENTED_EDGE('',*,*,#5316,.F.);
#7659=ORIENTED_EDGE('',*,*,#5384,.T.);
#7660=ORIENTED_EDGE('',*,*,#5360,.T.);
#7661=ORIENTED_EDGE('',*,*,#5385,.T.);
#7662=ORIENTED_EDGE('',*,*,#5314,.F.);
#7663=ORIENTED_EDGE('',*,*,#5383,.T.);
#7664=ORIENTED_EDGE('',*,*,#5362,.T.);
#7665=ORIENTED_EDGE('',*,*,#5349,.T.);
#7666=ORIENTED_EDGE('',*,*,#5394,.F.);
#7667=ORIENTED_EDGE('',*,*,#5327,.F.);
#7668=ORIENTED_EDGE('',*,*,#5233,.F.);
#7669=ORIENTED_EDGE('',*,*,#5328,.F.);
#7670=ORIENTED_EDGE('',*,*,#5394,.T.);
#7671=ORIENTED_EDGE('',*,*,#5348,.T.);
#7672=ORIENTED_EDGE('',*,*,#5243,.F.);
#7673=ORIENTED_EDGE('',*,*,#5326,.F.);
#7674=ORIENTED_EDGE('',*,*,#5395,.T.);
#7675=ORIENTED_EDGE('',*,*,#5350,.T.);
#7676=ORIENTED_EDGE('',*,*,#5231,.F.);
#7677=ORIENTED_EDGE('',*,*,#5351,.T.);
#7678=ORIENTED_EDGE('',*,*,#5395,.F.);
#7679=ORIENTED_EDGE('',*,*,#5325,.F.);
#7680=ORIENTED_EDGE('',*,*,#5247,.F.);
#7681=ORIENTED_EDGE('',*,*,#5264,.F.);
#7682=ORIENTED_EDGE('',*,*,#5396,.T.);
#7683=ORIENTED_EDGE('',*,*,#5278,.F.);
#7684=ORIENTED_EDGE('',*,*,#5397,.F.);
#7685=ORIENTED_EDGE('',*,*,#5397,.T.);
#7686=ORIENTED_EDGE('',*,*,#5249,.F.);
#7687=ORIENTED_EDGE('',*,*,#5398,.F.);
#7688=ORIENTED_EDGE('',*,*,#5265,.F.);
#7689=ORIENTED_EDGE('',*,*,#5398,.T.);
#7690=ORIENTED_EDGE('',*,*,#5272,.F.);
#7691=ORIENTED_EDGE('',*,*,#5206,.F.);
#7692=ORIENTED_EDGE('',*,*,#5266,.F.);
#7693=ORIENTED_EDGE('',*,*,#5204,.T.);
#7694=ORIENTED_EDGE('',*,*,#5304,.F.);
#7695=ORIENTED_EDGE('',*,*,#5399,.F.);
#7696=ORIENTED_EDGE('',*,*,#5267,.F.);
#7697=ORIENTED_EDGE('',*,*,#5399,.T.);
#7698=ORIENTED_EDGE('',*,*,#5297,.F.);
#7699=ORIENTED_EDGE('',*,*,#5400,.F.);
#7700=ORIENTED_EDGE('',*,*,#5268,.F.);
#7701=ORIENTED_EDGE('',*,*,#5400,.T.);
#7702=ORIENTED_EDGE('',*,*,#5296,.F.);
#7703=ORIENTED_EDGE('',*,*,#5401,.F.);
#7704=ORIENTED_EDGE('',*,*,#5219,.F.);
#7705=ORIENTED_EDGE('',*,*,#5309,.F.);
#7706=ORIENTED_EDGE('',*,*,#5332,.F.);
#7707=ORIENTED_EDGE('',*,*,#5401,.T.);
#7708=ORIENTED_EDGE('',*,*,#5295,.F.);
#7709=ORIENTED_EDGE('',*,*,#5333,.F.);
#7710=ORIENTED_EDGE('',*,*,#5280,.F.);
#7711=ORIENTED_EDGE('',*,*,#5402,.T.);
#7712=ORIENTED_EDGE('',*,*,#5260,.F.);
#7713=ORIENTED_EDGE('',*,*,#5403,.F.);
#7714=ORIENTED_EDGE('',*,*,#5403,.T.);
#7715=ORIENTED_EDGE('',*,*,#5259,.F.);
#7716=ORIENTED_EDGE('',*,*,#5404,.F.);
#7717=ORIENTED_EDGE('',*,*,#5371,.F.);
#7718=ORIENTED_EDGE('',*,*,#5404,.T.);
#7719=ORIENTED_EDGE('',*,*,#5258,.F.);
#7720=ORIENTED_EDGE('',*,*,#5202,.F.);
#7721=ORIENTED_EDGE('',*,*,#5277,.F.);
#7722=ORIENTED_EDGE('',*,*,#5200,.T.);
#7723=ORIENTED_EDGE('',*,*,#5257,.F.);
#7724=ORIENTED_EDGE('',*,*,#5405,.F.);
#7725=ORIENTED_EDGE('',*,*,#5303,.F.);
#7726=ORIENTED_EDGE('',*,*,#5405,.T.);
#7727=ORIENTED_EDGE('',*,*,#5256,.F.);
#7728=ORIENTED_EDGE('',*,*,#5406,.F.);
#7729=ORIENTED_EDGE('',*,*,#5299,.F.);
#7730=ORIENTED_EDGE('',*,*,#5406,.T.);
#7731=ORIENTED_EDGE('',*,*,#5223,.F.);
#7732=ORIENTED_EDGE('',*,*,#5407,.F.);
#7733=ORIENTED_EDGE('',*,*,#5300,.F.);
#7734=ORIENTED_EDGE('',*,*,#5340,.F.);
#7735=ORIENTED_EDGE('',*,*,#5301,.F.);
#7736=ORIENTED_EDGE('',*,*,#5407,.T.);
#7737=ORIENTED_EDGE('',*,*,#5343,.F.);
#7738=ORIENTED_EDGE('',*,*,#5366,.F.);
#7739=ORIENTED_EDGE('',*,*,#5305,.F.);
#7740=ORIENTED_EDGE('',*,*,#5241,.F.);
#7741=ORIENTED_EDGE('',*,*,#5408,.F.);
#7742=ORIENTED_EDGE('',*,*,#5334,.F.);
#7743=ORIENTED_EDGE('',*,*,#5408,.T.);
#7744=ORIENTED_EDGE('',*,*,#5240,.F.);
#7745=ORIENTED_EDGE('',*,*,#5409,.F.);
#7746=ORIENTED_EDGE('',*,*,#5369,.F.);
#7747=ORIENTED_EDGE('',*,*,#5409,.T.);
#7748=ORIENTED_EDGE('',*,*,#5239,.F.);
#7749=ORIENTED_EDGE('',*,*,#5410,.F.);
#7750=ORIENTED_EDGE('',*,*,#5271,.F.);
#7751=ORIENTED_EDGE('',*,*,#5410,.T.);
#7752=ORIENTED_EDGE('',*,*,#5290,.F.);
#7753=ORIENTED_EDGE('',*,*,#5411,.F.);
#7754=ORIENTED_EDGE('',*,*,#5262,.F.);
#7755=ORIENTED_EDGE('',*,*,#5412,.F.);
#7756=ORIENTED_EDGE('',*,*,#5263,.F.);
#7757=ORIENTED_EDGE('',*,*,#5411,.T.);
#7758=ORIENTED_EDGE('',*,*,#5288,.F.);
#7759=ORIENTED_EDGE('',*,*,#5396,.F.);
#7760=ORIENTED_EDGE('',*,*,#5412,.T.);
#7761=ORIENTED_EDGE('',*,*,#5413,.F.);
#7762=ORIENTED_EDGE('',*,*,#5414,.F.);
#7763=ORIENTED_EDGE('',*,*,#5279,.F.);
#7764=ORIENTED_EDGE('',*,*,#5413,.T.);
#7765=ORIENTED_EDGE('',*,*,#5287,.F.);
#7766=ORIENTED_EDGE('',*,*,#5402,.F.);
#7767=ORIENTED_EDGE('',*,*,#5414,.T.);
#7768=ORIENTED_EDGE('',*,*,#5415,.F.);
#7769=ORIENTED_EDGE('',*,*,#5415,.T.);
#7770=ORIENTED_EDGE('',*,*,#5286,.F.);
#7771=ORIENTED_EDGE('',*,*,#5416,.F.);
#7772=ORIENTED_EDGE('',*,*,#5261,.F.);
#7773=ORIENTED_EDGE('',*,*,#5416,.T.);
#7774=ORIENTED_EDGE('',*,*,#5289,.F.);
#7775=ORIENTED_EDGE('',*,*,#5417,.F.);
#7776=ORIENTED_EDGE('',*,*,#5252,.F.);
#7777=ORIENTED_EDGE('',*,*,#5417,.T.);
#7778=ORIENTED_EDGE('',*,*,#5237,.F.);
#7779=ORIENTED_EDGE('',*,*,#5418,.F.);
#7780=ORIENTED_EDGE('',*,*,#5253,.F.);
#7781=ORIENTED_EDGE('',*,*,#5418,.T.);
#7782=ORIENTED_EDGE('',*,*,#5236,.F.);
#7783=ORIENTED_EDGE('',*,*,#5419,.F.);
#7784=ORIENTED_EDGE('',*,*,#5367,.F.);
#7785=ORIENTED_EDGE('',*,*,#5347,.F.);
#7786=ORIENTED_EDGE('',*,*,#5337,.F.);
#7787=ORIENTED_EDGE('',*,*,#5419,.T.);
#7788=ORIENTED_EDGE('',*,*,#5235,.F.);
#7789=ORIENTED_EDGE('',*,*,#5420,.F.);
#7790=ORIENTED_EDGE('',*,*,#5421,.F.);
#7791=ORIENTED_EDGE('',*,*,#5422,.F.);
#7792=ORIENTED_EDGE('',*,*,#5423,.F.);
#7793=ORIENTED_EDGE('',*,*,#5424,.F.);
#7794=ORIENTED_EDGE('',*,*,#5425,.F.);
#7795=ORIENTED_EDGE('',*,*,#5426,.F.);
#7796=ORIENTED_EDGE('',*,*,#5427,.F.);
#7797=ORIENTED_EDGE('',*,*,#5428,.F.);
#7798=ORIENTED_EDGE('',*,*,#5429,.F.);
#7799=ORIENTED_EDGE('',*,*,#5430,.F.);
#7800=ORIENTED_EDGE('',*,*,#5431,.F.);
#7801=ORIENTED_EDGE('',*,*,#5432,.F.);
#7802=ORIENTED_EDGE('',*,*,#5433,.F.);
#7803=ORIENTED_EDGE('',*,*,#5434,.F.);
#7804=ORIENTED_EDGE('',*,*,#5435,.F.);
#7805=ORIENTED_EDGE('',*,*,#5436,.F.);
#7806=ORIENTED_EDGE('',*,*,#5437,.F.);
#7807=ORIENTED_EDGE('',*,*,#5438,.T.);
#7808=ORIENTED_EDGE('',*,*,#5439,.F.);
#7809=ORIENTED_EDGE('',*,*,#5440,.F.);
#7810=ORIENTED_EDGE('',*,*,#5441,.F.);
#7811=ORIENTED_EDGE('',*,*,#5442,.T.);
#7812=ORIENTED_EDGE('',*,*,#5443,.T.);
#7813=ORIENTED_EDGE('',*,*,#5444,.F.);
#7814=ORIENTED_EDGE('',*,*,#5443,.F.);
#7815=ORIENTED_EDGE('',*,*,#5445,.T.);
#7816=ORIENTED_EDGE('',*,*,#5446,.T.);
#7817=ORIENTED_EDGE('',*,*,#5447,.F.);
#7818=ORIENTED_EDGE('',*,*,#5446,.F.);
#7819=ORIENTED_EDGE('',*,*,#5448,.T.);
#7820=ORIENTED_EDGE('',*,*,#5449,.T.);
#7821=ORIENTED_EDGE('',*,*,#5450,.F.);
#7822=ORIENTED_EDGE('',*,*,#5449,.F.);
#7823=ORIENTED_EDGE('',*,*,#5420,.T.);
#7824=ORIENTED_EDGE('',*,*,#5451,.T.);
#7825=ORIENTED_EDGE('',*,*,#5452,.T.);
#7826=ORIENTED_EDGE('',*,*,#5453,.F.);
#7827=ORIENTED_EDGE('',*,*,#5454,.T.);
#7828=ORIENTED_EDGE('',*,*,#5455,.T.);
#7829=ORIENTED_EDGE('',*,*,#5456,.F.);
#7830=ORIENTED_EDGE('',*,*,#5455,.F.);
#7831=ORIENTED_EDGE('',*,*,#5457,.F.);
#7832=ORIENTED_EDGE('',*,*,#5458,.T.);
#7833=ORIENTED_EDGE('',*,*,#5459,.F.);
#7834=ORIENTED_EDGE('',*,*,#5458,.F.);
#7835=ORIENTED_EDGE('',*,*,#5460,.T.);
#7836=ORIENTED_EDGE('',*,*,#5461,.T.);
#7837=ORIENTED_EDGE('',*,*,#5462,.F.);
#7838=ORIENTED_EDGE('',*,*,#5461,.F.);
#7839=ORIENTED_EDGE('',*,*,#5463,.F.);
#7840=ORIENTED_EDGE('',*,*,#5464,.T.);
#7841=ORIENTED_EDGE('',*,*,#5427,.T.);
#7842=ORIENTED_EDGE('',*,*,#5465,.F.);
#7843=ORIENTED_EDGE('',*,*,#5432,.T.);
#7844=ORIENTED_EDGE('',*,*,#5466,.T.);
#7845=ORIENTED_EDGE('',*,*,#5434,.T.);
#7846=ORIENTED_EDGE('',*,*,#5467,.F.);
#7847=ORIENTED_EDGE('',*,*,#5468,.T.);
#7848=ORIENTED_EDGE('',*,*,#5428,.T.);
#7849=ORIENTED_EDGE('',*,*,#5464,.F.);
#7850=ORIENTED_EDGE('',*,*,#5469,.F.);
#7851=ORIENTED_EDGE('',*,*,#5470,.T.);
#7852=ORIENTED_EDGE('',*,*,#5471,.T.);
#7853=ORIENTED_EDGE('',*,*,#5451,.F.);
#7854=ORIENTED_EDGE('',*,*,#5424,.T.);
#7855=ORIENTED_EDGE('',*,*,#5465,.T.);
#7856=ORIENTED_EDGE('',*,*,#5472,.T.);
#7857=ORIENTED_EDGE('',*,*,#5473,.F.);
#7858=ORIENTED_EDGE('',*,*,#5474,.F.);
#7859=ORIENTED_EDGE('',*,*,#5475,.T.);
#7860=ORIENTED_EDGE('',*,*,#5476,.T.);
#7861=ORIENTED_EDGE('',*,*,#5477,.F.);
#7862=ORIENTED_EDGE('',*,*,#5478,.F.);
#7863=ORIENTED_EDGE('',*,*,#5479,.F.);
#7864=ORIENTED_EDGE('',*,*,#5473,.T.);
#7865=ORIENTED_EDGE('',*,*,#5480,.T.);
#7866=ORIENTED_EDGE('',*,*,#5430,.T.);
#7867=ORIENTED_EDGE('',*,*,#5481,.T.);
#7868=ORIENTED_EDGE('',*,*,#5422,.T.);
#7869=ORIENTED_EDGE('',*,*,#5482,.T.);
#7870=ORIENTED_EDGE('',*,*,#5483,.T.);
#7871=ORIENTED_EDGE('',*,*,#5484,.T.);
#7872=ORIENTED_EDGE('',*,*,#5485,.T.);
#7873=ORIENTED_EDGE('',*,*,#5486,.T.);
#7874=ORIENTED_EDGE('',*,*,#5487,.T.);
#7875=ORIENTED_EDGE('',*,*,#5488,.T.);
#7876=ORIENTED_EDGE('',*,*,#5448,.F.);
#7877=ORIENTED_EDGE('',*,*,#5444,.T.);
#7878=ORIENTED_EDGE('',*,*,#5489,.F.);
#7879=ORIENTED_EDGE('',*,*,#5436,.T.);
#7880=ORIENTED_EDGE('',*,*,#5490,.T.);
#7881=ORIENTED_EDGE('',*,*,#5491,.T.);
#7882=ORIENTED_EDGE('',*,*,#5492,.T.);
#7883=ORIENTED_EDGE('',*,*,#5493,.T.);
#7884=ORIENTED_EDGE('',*,*,#5494,.F.);
#7885=ORIENTED_EDGE('',*,*,#5495,.T.);
#7886=ORIENTED_EDGE('',*,*,#5496,.T.);
#7887=ORIENTED_EDGE('',*,*,#5425,.T.);
#7888=ORIENTED_EDGE('',*,*,#5454,.F.);
#7889=ORIENTED_EDGE('',*,*,#5462,.T.);
#7890=ORIENTED_EDGE('',*,*,#5497,.T.);
#7891=ORIENTED_EDGE('',*,*,#5498,.T.);
#7892=ORIENTED_EDGE('',*,*,#5499,.F.);
#7893=ORIENTED_EDGE('',*,*,#5500,.T.);
#7894=ORIENTED_EDGE('',*,*,#5499,.T.);
#7895=ORIENTED_EDGE('',*,*,#5501,.T.);
#7896=ORIENTED_EDGE('',*,*,#5502,.F.);
#7897=ORIENTED_EDGE('',*,*,#5503,.T.);
#7898=ORIENTED_EDGE('',*,*,#5502,.T.);
#7899=ORIENTED_EDGE('',*,*,#5504,.T.);
#7900=ORIENTED_EDGE('',*,*,#5466,.F.);
#7901=ORIENTED_EDGE('',*,*,#5505,.T.);
#7902=ORIENTED_EDGE('',*,*,#5506,.F.);
#7903=ORIENTED_EDGE('',*,*,#5507,.T.);
#7904=ORIENTED_EDGE('',*,*,#5453,.T.);
#7905=ORIENTED_EDGE('',*,*,#5508,.T.);
#7906=ORIENTED_EDGE('',*,*,#5509,.T.);
#7907=ORIENTED_EDGE('',*,*,#5510,.T.);
#7908=ORIENTED_EDGE('',*,*,#5511,.T.);
#7909=ORIENTED_EDGE('',*,*,#5512,.T.);
#7910=ORIENTED_EDGE('',*,*,#5506,.T.);
#7911=ORIENTED_EDGE('',*,*,#5513,.T.);
#7912=ORIENTED_EDGE('',*,*,#5514,.F.);
#7913=ORIENTED_EDGE('',*,*,#5515,.T.);
#7914=ORIENTED_EDGE('',*,*,#5516,.T.);
#7915=ORIENTED_EDGE('',*,*,#5494,.T.);
#7916=ORIENTED_EDGE('',*,*,#5517,.T.);
#7917=ORIENTED_EDGE('',*,*,#5518,.T.);
#7918=ORIENTED_EDGE('',*,*,#5519,.T.);
#7919=ORIENTED_EDGE('',*,*,#5520,.T.);
#7920=ORIENTED_EDGE('',*,*,#5521,.T.);
#7921=ORIENTED_EDGE('',*,*,#5445,.F.);
#7922=ORIENTED_EDGE('',*,*,#5522,.T.);
#7923=ORIENTED_EDGE('',*,*,#5523,.T.);
#7924=ORIENTED_EDGE('',*,*,#5515,.F.);
#7925=ORIENTED_EDGE('',*,*,#5524,.T.);
#7926=ORIENTED_EDGE('',*,*,#5459,.T.);
#7927=ORIENTED_EDGE('',*,*,#5484,.F.);
#7928=ORIENTED_EDGE('',*,*,#5525,.T.);
#7929=ORIENTED_EDGE('',*,*,#5518,.F.);
#7930=ORIENTED_EDGE('',*,*,#5526,.T.);
#7931=ORIENTED_EDGE('',*,*,#5527,.T.);
#7932=ORIENTED_EDGE('',*,*,#5528,.T.);
#7933=ORIENTED_EDGE('',*,*,#5529,.T.);
#7934=ORIENTED_EDGE('',*,*,#5530,.T.);
#7935=ORIENTED_EDGE('',*,*,#5497,.F.);
#7936=ORIENTED_EDGE('',*,*,#5531,.T.);
#7937=ORIENTED_EDGE('',*,*,#5532,.F.);
#7938=ORIENTED_EDGE('',*,*,#5438,.F.);
#7939=ORIENTED_EDGE('',*,*,#5533,.F.);
#7940=ORIENTED_EDGE('',*,*,#5534,.F.);
#7941=ORIENTED_EDGE('',*,*,#5535,.F.);
#7942=ORIENTED_EDGE('',*,*,#5536,.F.);
#7943=ORIENTED_EDGE('',*,*,#5513,.F.);
#7944=ORIENTED_EDGE('',*,*,#5508,.F.);
#7945=ORIENTED_EDGE('',*,*,#5452,.F.);
#7946=ORIENTED_EDGE('',*,*,#5471,.F.);
#7947=ORIENTED_EDGE('',*,*,#5442,.F.);
#7948=ORIENTED_EDGE('',*,*,#5450,.T.);
#7949=ORIENTED_EDGE('',*,*,#5440,.T.);
#7950=ORIENTED_EDGE('',*,*,#5537,.T.);
#7951=ORIENTED_EDGE('',*,*,#5469,.T.);
#7952=ORIENTED_EDGE('',*,*,#5463,.T.);
#7953=ORIENTED_EDGE('',*,*,#5474,.T.);
#7954=ORIENTED_EDGE('',*,*,#5479,.T.);
#7955=ORIENTED_EDGE('',*,*,#5538,.T.);
#7956=ORIENTED_EDGE('',*,*,#5539,.T.);
#7957=ORIENTED_EDGE('',*,*,#5540,.T.);
#7958=ORIENTED_EDGE('',*,*,#5541,.T.);
#7959=ORIENTED_EDGE('',*,*,#5460,.F.);
#7960=ORIENTED_EDGE('',*,*,#5456,.T.);
#7961=ORIENTED_EDGE('',*,*,#5539,.F.);
#7962=ORIENTED_EDGE('',*,*,#5542,.T.);
#7963=ORIENTED_EDGE('',*,*,#5543,.F.);
#7964=ORIENTED_EDGE('',*,*,#5544,.F.);
#7965=ORIENTED_EDGE('',*,*,#5545,.T.);
#7966=ORIENTED_EDGE('',*,*,#5546,.T.);
#7967=ORIENTED_EDGE('',*,*,#5535,.T.);
#7968=ORIENTED_EDGE('',*,*,#5547,.T.);
#7969=ORIENTED_EDGE('',*,*,#5540,.F.);
#7970=ORIENTED_EDGE('',*,*,#5547,.F.);
#7971=ORIENTED_EDGE('',*,*,#5534,.T.);
#7972=ORIENTED_EDGE('',*,*,#5548,.T.);
#7973=ORIENTED_EDGE('',*,*,#5541,.F.);
#7974=ORIENTED_EDGE('',*,*,#5548,.F.);
#7975=ORIENTED_EDGE('',*,*,#5533,.T.);
#7976=ORIENTED_EDGE('',*,*,#5441,.T.);
#7977=ORIENTED_EDGE('',*,*,#5478,.T.);
#7978=ORIENTED_EDGE('',*,*,#5549,.F.);
#7979=ORIENTED_EDGE('',*,*,#5542,.F.);
#7980=ORIENTED_EDGE('',*,*,#5538,.F.);
#7981=ORIENTED_EDGE('',*,*,#5550,.F.);
#7982=ORIENTED_EDGE('',*,*,#5551,.T.);
#7983=ORIENTED_EDGE('',*,*,#5509,.F.);
#7984=ORIENTED_EDGE('',*,*,#5552,.F.);
#7985=ORIENTED_EDGE('',*,*,#5545,.F.);
#7986=ORIENTED_EDGE('',*,*,#5553,.F.);
#7987=ORIENTED_EDGE('',*,*,#5554,.T.);
#7988=ORIENTED_EDGE('',*,*,#5543,.T.);
#7989=ORIENTED_EDGE('',*,*,#5549,.T.);
#7990=ORIENTED_EDGE('',*,*,#5477,.T.);
#7991=ORIENTED_EDGE('',*,*,#5536,.T.);
#7992=ORIENTED_EDGE('',*,*,#5546,.F.);
#7993=ORIENTED_EDGE('',*,*,#5552,.T.);
#7994=ORIENTED_EDGE('',*,*,#5514,.T.);
#7995=ORIENTED_EDGE('',*,*,#5555,.F.);
#7996=ORIENTED_EDGE('',*,*,#5550,.T.);
#7997=ORIENTED_EDGE('',*,*,#5544,.T.);
#7998=ORIENTED_EDGE('',*,*,#5554,.F.);
#7999=ORIENTED_EDGE('',*,*,#5491,.F.);
#8000=ORIENTED_EDGE('',*,*,#5556,.T.);
#8001=ORIENTED_EDGE('',*,*,#5501,.F.);
#8002=ORIENTED_EDGE('',*,*,#5557,.F.);
#8003=ORIENTED_EDGE('',*,*,#5530,.F.);
#8004=ORIENTED_EDGE('',*,*,#5558,.T.);
#8005=ORIENTED_EDGE('',*,*,#5492,.F.);
#8006=ORIENTED_EDGE('',*,*,#5557,.T.);
#8007=ORIENTED_EDGE('',*,*,#5498,.F.);
#8008=ORIENTED_EDGE('',*,*,#5503,.F.);
#8009=ORIENTED_EDGE('',*,*,#5559,.T.);
#8010=ORIENTED_EDGE('',*,*,#5487,.F.);
#8011=ORIENTED_EDGE('',*,*,#5560,.F.);
#8012=ORIENTED_EDGE('',*,*,#5531,.F.);
#8013=ORIENTED_EDGE('',*,*,#5500,.F.);
#8014=ORIENTED_EDGE('',*,*,#5560,.T.);
#8015=ORIENTED_EDGE('',*,*,#5486,.F.);
#8016=ORIENTED_EDGE('',*,*,#5561,.T.);
#8017=ORIENTED_EDGE('',*,*,#5556,.F.);
#8018=ORIENTED_EDGE('',*,*,#5490,.F.);
#8019=ORIENTED_EDGE('',*,*,#5435,.T.);
#8020=ORIENTED_EDGE('',*,*,#5504,.F.);
#8021=ORIENTED_EDGE('',*,*,#5559,.F.);
#8022=ORIENTED_EDGE('',*,*,#5505,.F.);
#8023=ORIENTED_EDGE('',*,*,#5431,.T.);
#8024=ORIENTED_EDGE('',*,*,#5488,.F.);
#8025=ORIENTED_EDGE('',*,*,#5558,.F.);
#8026=ORIENTED_EDGE('',*,*,#5529,.F.);
#8027=ORIENTED_EDGE('',*,*,#5562,.F.);
#8028=ORIENTED_EDGE('',*,*,#5563,.F.);
#8029=ORIENTED_EDGE('',*,*,#5524,.F.);
#8030=ORIENTED_EDGE('',*,*,#5517,.F.);
#8031=ORIENTED_EDGE('',*,*,#5493,.F.);
#8032=ORIENTED_EDGE('',*,*,#5426,.T.);
#8033=ORIENTED_EDGE('',*,*,#5496,.F.);
#8034=ORIENTED_EDGE('',*,*,#5564,.F.);
#8035=ORIENTED_EDGE('',*,*,#5480,.F.);
#8036=ORIENTED_EDGE('',*,*,#5472,.F.);
#8037=ORIENTED_EDGE('',*,*,#5563,.T.);
#8038=ORIENTED_EDGE('',*,*,#5565,.F.);
#8039=ORIENTED_EDGE('',*,*,#5566,.F.);
#8040=ORIENTED_EDGE('',*,*,#5522,.F.);
#8041=ORIENTED_EDGE('',*,*,#5516,.F.);
#8042=ORIENTED_EDGE('',*,*,#5523,.F.);
#8043=ORIENTED_EDGE('',*,*,#5566,.T.);
#8044=ORIENTED_EDGE('',*,*,#5567,.F.);
#8045=ORIENTED_EDGE('',*,*,#5475,.F.);
#8046=ORIENTED_EDGE('',*,*,#5564,.T.);
#8047=ORIENTED_EDGE('',*,*,#5495,.F.);
#8048=ORIENTED_EDGE('',*,*,#5526,.F.);
#8049=ORIENTED_EDGE('',*,*,#5521,.F.);
#8050=ORIENTED_EDGE('',*,*,#5568,.F.);
#8051=ORIENTED_EDGE('',*,*,#5569,.F.);
#8052=ORIENTED_EDGE('',*,*,#5527,.F.);
#8053=ORIENTED_EDGE('',*,*,#5561,.F.);
#8054=ORIENTED_EDGE('',*,*,#5485,.F.);
#8055=ORIENTED_EDGE('',*,*,#5507,.F.);
#8056=ORIENTED_EDGE('',*,*,#5512,.F.);
#8057=ORIENTED_EDGE('',*,*,#5570,.F.);
#8058=ORIENTED_EDGE('',*,*,#5482,.F.);
#8059=ORIENTED_EDGE('',*,*,#5421,.T.);
#8060=ORIENTED_EDGE('',*,*,#5568,.T.);
#8061=ORIENTED_EDGE('',*,*,#5520,.F.);
#8062=ORIENTED_EDGE('',*,*,#5571,.F.);
#8063=ORIENTED_EDGE('',*,*,#5572,.F.);
#8064=ORIENTED_EDGE('',*,*,#5570,.T.);
#8065=ORIENTED_EDGE('',*,*,#5511,.F.);
#8066=ORIENTED_EDGE('',*,*,#5573,.F.);
#8067=ORIENTED_EDGE('',*,*,#5571,.T.);
#8068=ORIENTED_EDGE('',*,*,#5519,.F.);
#8069=ORIENTED_EDGE('',*,*,#5525,.F.);
#8070=ORIENTED_EDGE('',*,*,#5483,.F.);
#8071=ORIENTED_EDGE('',*,*,#5439,.T.);
#8072=ORIENTED_EDGE('',*,*,#5532,.T.);
#8073=ORIENTED_EDGE('',*,*,#5470,.F.);
#8074=ORIENTED_EDGE('',*,*,#5423,.T.);
#8075=ORIENTED_EDGE('',*,*,#5481,.F.);
#8076=ORIENTED_EDGE('',*,*,#5433,.T.);
#8077=ORIENTED_EDGE('',*,*,#5467,.T.);
#8078=ORIENTED_EDGE('',*,*,#5437,.T.);
#8079=ORIENTED_EDGE('',*,*,#5489,.T.);
#8080=ORIENTED_EDGE('',*,*,#5429,.T.);
#8081=ORIENTED_EDGE('',*,*,#5468,.F.);
#8082=ORIENTED_EDGE('',*,*,#5537,.F.);
#8083=ORIENTED_EDGE('',*,*,#5574,.T.);
#8084=ORIENTED_EDGE('',*,*,#5510,.F.);
#8085=ORIENTED_EDGE('',*,*,#5551,.F.);
#8086=ORIENTED_EDGE('',*,*,#5555,.T.);
#8087=ORIENTED_EDGE('',*,*,#5553,.T.);
#8088=ORIENTED_EDGE('',*,*,#5476,.F.);
#8089=ORIENTED_EDGE('',*,*,#5575,.F.);
#8090=ORIENTED_EDGE('',*,*,#5528,.F.);
#8091=ORIENTED_EDGE('',*,*,#5562,.T.);
#8092=ORIENTED_EDGE('',*,*,#5575,.T.);
#8093=ORIENTED_EDGE('',*,*,#5567,.T.);
#8094=ORIENTED_EDGE('',*,*,#5565,.T.);
#8095=ORIENTED_EDGE('',*,*,#5457,.T.);
#8096=ORIENTED_EDGE('',*,*,#5569,.T.);
#8097=ORIENTED_EDGE('',*,*,#5572,.T.);
#8098=ORIENTED_EDGE('',*,*,#5573,.T.);
#8099=ORIENTED_EDGE('',*,*,#5574,.F.);
#8100=ORIENTED_EDGE('',*,*,#5447,.T.);
#8101=ORIENTED_EDGE('',*,*,#5576,.F.);
#8102=ORIENTED_EDGE('',*,*,#5577,.T.);
#8103=ORIENTED_EDGE('',*,*,#5577,.F.);
#8104=ORIENTED_EDGE('',*,*,#5578,.T.);
#8105=ORIENTED_EDGE('',*,*,#5579,.F.);
#8106=ORIENTED_EDGE('',*,*,#5579,.T.);
#8107=ORIENTED_EDGE('',*,*,#5580,.F.);
#8108=ORIENTED_EDGE('',*,*,#5581,.T.);
#8109=ORIENTED_EDGE('',*,*,#5582,.F.);
#8110=ORIENTED_EDGE('',*,*,#5581,.F.);
#8111=ORIENTED_EDGE('',*,*,#5578,.F.);
#8112=ORIENTED_EDGE('',*,*,#5582,.T.);
#8113=ORIENTED_EDGE('',*,*,#5576,.T.);
#8114=ORIENTED_EDGE('',*,*,#5580,.T.);
#8115=ORIENTED_EDGE('',*,*,#5583,.T.);
#8116=ORIENTED_EDGE('',*,*,#5584,.F.);
#8117=ORIENTED_EDGE('',*,*,#5585,.T.);
#8118=ORIENTED_EDGE('',*,*,#5586,.T.);
#8119=ORIENTED_EDGE('',*,*,#5585,.F.);
#8120=ORIENTED_EDGE('',*,*,#5587,.F.);
#8121=ORIENTED_EDGE('',*,*,#5587,.T.);
#8122=ORIENTED_EDGE('',*,*,#5586,.F.);
#8123=ORIENTED_EDGE('',*,*,#5583,.F.);
#8124=ORIENTED_EDGE('',*,*,#5584,.T.);
#8125=ORIENTED_EDGE('',*,*,#5588,.T.);
#8126=ORIENTED_EDGE('',*,*,#5589,.T.);
#8127=ORIENTED_EDGE('',*,*,#5590,.F.);
#8128=ORIENTED_EDGE('',*,*,#5591,.F.);
#8129=ORIENTED_EDGE('',*,*,#5592,.F.);
#8130=ORIENTED_EDGE('',*,*,#5589,.F.);
#8131=ORIENTED_EDGE('',*,*,#5593,.F.);
#8132=ORIENTED_EDGE('',*,*,#5594,.T.);
#8133=ORIENTED_EDGE('',*,*,#5595,.T.);
#8134=ORIENTED_EDGE('',*,*,#5596,.T.);
#8135=ORIENTED_EDGE('',*,*,#5597,.T.);
#8136=ORIENTED_EDGE('',*,*,#5598,.T.);
#8137=ORIENTED_EDGE('',*,*,#5599,.T.);
#8138=ORIENTED_EDGE('',*,*,#5600,.F.);
#8139=ORIENTED_EDGE('',*,*,#5601,.T.);
#8140=ORIENTED_EDGE('',*,*,#5602,.T.);
#8141=ORIENTED_EDGE('',*,*,#5603,.T.);
#8142=ORIENTED_EDGE('',*,*,#5604,.T.);
#8143=ORIENTED_EDGE('',*,*,#5605,.F.);
#8144=ORIENTED_EDGE('',*,*,#5604,.F.);
#8145=ORIENTED_EDGE('',*,*,#5606,.T.);
#8146=ORIENTED_EDGE('',*,*,#5607,.T.);
#8147=ORIENTED_EDGE('',*,*,#5608,.T.);
#8148=ORIENTED_EDGE('',*,*,#5609,.T.);
#8149=ORIENTED_EDGE('',*,*,#5610,.T.);
#8150=ORIENTED_EDGE('',*,*,#5611,.T.);
#8151=ORIENTED_EDGE('',*,*,#5612,.F.);
#8152=ORIENTED_EDGE('',*,*,#5613,.T.);
#8153=ORIENTED_EDGE('',*,*,#5614,.T.);
#8154=ORIENTED_EDGE('',*,*,#5615,.T.);
#8155=ORIENTED_EDGE('',*,*,#5616,.F.);
#8156=ORIENTED_EDGE('',*,*,#5617,.F.);
#8157=ORIENTED_EDGE('',*,*,#5616,.T.);
#8158=ORIENTED_EDGE('',*,*,#5618,.T.);
#8159=ORIENTED_EDGE('',*,*,#5596,.F.);
#8160=ORIENTED_EDGE('',*,*,#5619,.T.);
#8161=ORIENTED_EDGE('',*,*,#5620,.T.);
#8162=ORIENTED_EDGE('',*,*,#5621,.T.);
#8163=ORIENTED_EDGE('',*,*,#5622,.T.);
#8164=ORIENTED_EDGE('',*,*,#5623,.T.);
#8165=ORIENTED_EDGE('',*,*,#5593,.T.);
#8166=ORIENTED_EDGE('',*,*,#5624,.T.);
#8167=ORIENTED_EDGE('',*,*,#5588,.F.);
#8168=ORIENTED_EDGE('',*,*,#5615,.F.);
#8169=ORIENTED_EDGE('',*,*,#5625,.T.);
#8170=ORIENTED_EDGE('',*,*,#5626,.T.);
#8171=ORIENTED_EDGE('',*,*,#5627,.T.);
#8172=ORIENTED_EDGE('',*,*,#5597,.F.);
#8173=ORIENTED_EDGE('',*,*,#5618,.F.);
#8174=ORIENTED_EDGE('',*,*,#5605,.T.);
#8175=ORIENTED_EDGE('',*,*,#5600,.T.);
#8176=ORIENTED_EDGE('',*,*,#5628,.T.);
#8177=ORIENTED_EDGE('',*,*,#5608,.F.);
#8178=ORIENTED_EDGE('',*,*,#5629,.T.);
#8179=ORIENTED_EDGE('',*,*,#5622,.F.);
#8180=ORIENTED_EDGE('',*,*,#5630,.T.);
#8181=ORIENTED_EDGE('',*,*,#5631,.T.);
#8182=ORIENTED_EDGE('',*,*,#5632,.T.);
#8183=ORIENTED_EDGE('',*,*,#5633,.F.);
#8184=ORIENTED_EDGE('',*,*,#5633,.T.);
#8185=ORIENTED_EDGE('',*,*,#5634,.T.);
#8186=ORIENTED_EDGE('',*,*,#5635,.T.);
#8187=ORIENTED_EDGE('',*,*,#5594,.F.);
#8188=ORIENTED_EDGE('',*,*,#5623,.F.);
#8189=ORIENTED_EDGE('',*,*,#5632,.F.);
#8190=ORIENTED_EDGE('',*,*,#5636,.T.);
#8191=ORIENTED_EDGE('',*,*,#5590,.T.);
#8192=ORIENTED_EDGE('',*,*,#5592,.T.);
#8193=ORIENTED_EDGE('',*,*,#5637,.T.);
#8194=ORIENTED_EDGE('',*,*,#5634,.F.);
#8195=ORIENTED_EDGE('',*,*,#5617,.T.);
#8196=ORIENTED_EDGE('',*,*,#5638,.T.);
#8197=ORIENTED_EDGE('',*,*,#5606,.F.);
#8198=ORIENTED_EDGE('',*,*,#5603,.F.);
#8199=ORIENTED_EDGE('',*,*,#5639,.T.);
#8200=ORIENTED_EDGE('',*,*,#5612,.T.);
#8201=ORIENTED_EDGE('',*,*,#5595,.F.);
#8202=ORIENTED_EDGE('',*,*,#5640,.T.);
#8203=ORIENTED_EDGE('',*,*,#5641,.T.);
#8204=ORIENTED_EDGE('',*,*,#5642,.T.);
#8205=ORIENTED_EDGE('',*,*,#5643,.T.);
#8206=ORIENTED_EDGE('',*,*,#5644,.T.);
#8207=ORIENTED_EDGE('',*,*,#5645,.T.);
#8208=ORIENTED_EDGE('',*,*,#5646,.T.);
#8209=ORIENTED_EDGE('',*,*,#5598,.F.);
#8210=ORIENTED_EDGE('',*,*,#5627,.F.);
#8211=ORIENTED_EDGE('',*,*,#5647,.F.);
#8212=ORIENTED_EDGE('',*,*,#5628,.F.);
#8213=ORIENTED_EDGE('',*,*,#5599,.F.);
#8214=ORIENTED_EDGE('',*,*,#5601,.F.);
#8215=ORIENTED_EDGE('',*,*,#5629,.F.);
#8216=ORIENTED_EDGE('',*,*,#5648,.F.);
#8217=ORIENTED_EDGE('',*,*,#5624,.F.);
#8218=ORIENTED_EDGE('',*,*,#5602,.F.);
#8219=ORIENTED_EDGE('',*,*,#5647,.T.);
#8220=ORIENTED_EDGE('',*,*,#5626,.F.);
#8221=ORIENTED_EDGE('',*,*,#5649,.F.);
#8222=ORIENTED_EDGE('',*,*,#5609,.F.);
#8223=ORIENTED_EDGE('',*,*,#5648,.T.);
#8224=ORIENTED_EDGE('',*,*,#5611,.F.);
#8225=ORIENTED_EDGE('',*,*,#5650,.F.);
#8226=ORIENTED_EDGE('',*,*,#5620,.F.);
#8227=ORIENTED_EDGE('',*,*,#5614,.F.);
#8228=ORIENTED_EDGE('',*,*,#5651,.T.);
#8229=ORIENTED_EDGE('',*,*,#5643,.F.);
#8230=ORIENTED_EDGE('',*,*,#5652,.T.);
#8231=ORIENTED_EDGE('',*,*,#5630,.F.);
#8232=ORIENTED_EDGE('',*,*,#5621,.F.);
#8233=ORIENTED_EDGE('',*,*,#5650,.T.);
#8234=ORIENTED_EDGE('',*,*,#5610,.F.);
#8235=ORIENTED_EDGE('',*,*,#5649,.T.);
#8236=ORIENTED_EDGE('',*,*,#5625,.F.);
#8237=ORIENTED_EDGE('',*,*,#5652,.F.);
#8238=ORIENTED_EDGE('',*,*,#5642,.F.);
#8239=ORIENTED_EDGE('',*,*,#5653,.F.);
#8240=ORIENTED_EDGE('',*,*,#5636,.F.);
#8241=ORIENTED_EDGE('',*,*,#5631,.F.);
#8242=ORIENTED_EDGE('',*,*,#5653,.T.);
#8243=ORIENTED_EDGE('',*,*,#5641,.F.);
#8244=ORIENTED_EDGE('',*,*,#5654,.F.);
#8245=ORIENTED_EDGE('',*,*,#5591,.T.);
#8246=ORIENTED_EDGE('',*,*,#5635,.F.);
#8247=ORIENTED_EDGE('',*,*,#5637,.F.);
#8248=ORIENTED_EDGE('',*,*,#5654,.T.);
#8249=ORIENTED_EDGE('',*,*,#5640,.F.);
#8250=ORIENTED_EDGE('',*,*,#5613,.F.);
#8251=ORIENTED_EDGE('',*,*,#5639,.F.);
#8252=ORIENTED_EDGE('',*,*,#5655,.F.);
#8253=ORIENTED_EDGE('',*,*,#5644,.F.);
#8254=ORIENTED_EDGE('',*,*,#5651,.F.);
#8255=ORIENTED_EDGE('',*,*,#5655,.T.);
#8256=ORIENTED_EDGE('',*,*,#5607,.F.);
#8257=ORIENTED_EDGE('',*,*,#5656,.F.);
#8258=ORIENTED_EDGE('',*,*,#5645,.F.);
#8259=ORIENTED_EDGE('',*,*,#5619,.F.);
#8260=ORIENTED_EDGE('',*,*,#5646,.F.);
#8261=ORIENTED_EDGE('',*,*,#5656,.T.);
#8262=ORIENTED_EDGE('',*,*,#5638,.F.);
#8263=ORIENTED_EDGE('',*,*,#5657,.F.);
#8264=ORIENTED_EDGE('',*,*,#5658,.T.);
#8265=ORIENTED_EDGE('',*,*,#5659,.F.);
#8266=ORIENTED_EDGE('',*,*,#5658,.F.);
#8267=ORIENTED_EDGE('',*,*,#5660,.F.);
#8268=ORIENTED_EDGE('',*,*,#5661,.T.);
#8269=ORIENTED_EDGE('',*,*,#5662,.F.);
#8270=ORIENTED_EDGE('',*,*,#5663,.F.);
#8271=ORIENTED_EDGE('',*,*,#5664,.F.);
#8272=ORIENTED_EDGE('',*,*,#5665,.T.);
#8273=ORIENTED_EDGE('',*,*,#5666,.F.);
#8274=ORIENTED_EDGE('',*,*,#5665,.F.);
#8275=ORIENTED_EDGE('',*,*,#5667,.F.);
#8276=ORIENTED_EDGE('',*,*,#5668,.F.);
#8277=ORIENTED_EDGE('',*,*,#5669,.F.);
#8278=ORIENTED_EDGE('',*,*,#5670,.T.);
#8279=ORIENTED_EDGE('',*,*,#5671,.F.);
#8280=ORIENTED_EDGE('',*,*,#5672,.T.);
#8281=ORIENTED_EDGE('',*,*,#5673,.F.);
#8282=ORIENTED_EDGE('',*,*,#5672,.F.);
#8283=ORIENTED_EDGE('',*,*,#5674,.F.);
#8284=ORIENTED_EDGE('',*,*,#5675,.T.);
#8285=ORIENTED_EDGE('',*,*,#5676,.F.);
#8286=ORIENTED_EDGE('',*,*,#5675,.F.);
#8287=ORIENTED_EDGE('',*,*,#5676,.T.);
#8288=ORIENTED_EDGE('',*,*,#5677,.T.);
#8289=ORIENTED_EDGE('',*,*,#5664,.T.);
#8290=ORIENTED_EDGE('',*,*,#5677,.F.);
#8291=ORIENTED_EDGE('',*,*,#5673,.T.);
#8292=ORIENTED_EDGE('',*,*,#5678,.T.);
#8293=ORIENTED_EDGE('',*,*,#5657,.T.);
#8294=ORIENTED_EDGE('',*,*,#5678,.F.);
#8295=ORIENTED_EDGE('',*,*,#5669,.T.);
#8296=ORIENTED_EDGE('',*,*,#5679,.T.);
#8297=ORIENTED_EDGE('',*,*,#5660,.T.);
#8298=ORIENTED_EDGE('',*,*,#5680,.F.);
#8299=ORIENTED_EDGE('',*,*,#5681,.T.);
#8300=ORIENTED_EDGE('',*,*,#5682,.T.);
#8301=ORIENTED_EDGE('',*,*,#5667,.T.);
#8302=ORIENTED_EDGE('',*,*,#5683,.T.);
#8303=ORIENTED_EDGE('',*,*,#5684,.T.);
#8304=ORIENTED_EDGE('',*,*,#5685,.T.);
#8305=ORIENTED_EDGE('',*,*,#5686,.T.);
#8306=ORIENTED_EDGE('',*,*,#5687,.T.);
#8307=ORIENTED_EDGE('',*,*,#5674,.T.);
#8308=ORIENTED_EDGE('',*,*,#5671,.T.);
#8309=ORIENTED_EDGE('',*,*,#5688,.T.);
#8310=ORIENTED_EDGE('',*,*,#5689,.T.);
#8311=ORIENTED_EDGE('',*,*,#5662,.T.);
#8312=ORIENTED_EDGE('',*,*,#5690,.T.);
#8313=ORIENTED_EDGE('',*,*,#5691,.T.);
#8314=ORIENTED_EDGE('',*,*,#5692,.T.);
#8315=ORIENTED_EDGE('',*,*,#5693,.T.);
#8316=ORIENTED_EDGE('',*,*,#5694,.T.);
#8317=ORIENTED_EDGE('',*,*,#5659,.T.);
#8318=ORIENTED_EDGE('',*,*,#5666,.T.);
#8319=ORIENTED_EDGE('',*,*,#5695,.F.);
#8320=ORIENTED_EDGE('',*,*,#5696,.T.);
#8321=ORIENTED_EDGE('',*,*,#5680,.T.);
#8322=ORIENTED_EDGE('',*,*,#5697,.T.);
#8323=ORIENTED_EDGE('',*,*,#5698,.F.);
#8324=ORIENTED_EDGE('',*,*,#5699,.T.);
#8325=ORIENTED_EDGE('',*,*,#5695,.T.);
#8326=ORIENTED_EDGE('',*,*,#5700,.T.);
#8327=ORIENTED_EDGE('',*,*,#5701,.F.);
#8328=ORIENTED_EDGE('',*,*,#5702,.T.);
#8329=ORIENTED_EDGE('',*,*,#5698,.T.);
#8330=ORIENTED_EDGE('',*,*,#5703,.T.);
#8331=ORIENTED_EDGE('',*,*,#5704,.F.);
#8332=ORIENTED_EDGE('',*,*,#5705,.T.);
#8333=ORIENTED_EDGE('',*,*,#5701,.T.);
#8334=ORIENTED_EDGE('',*,*,#5706,.T.);
#8335=ORIENTED_EDGE('',*,*,#5707,.F.);
#8336=ORIENTED_EDGE('',*,*,#5708,.T.);
#8337=ORIENTED_EDGE('',*,*,#5704,.T.);
#8338=ORIENTED_EDGE('',*,*,#5709,.T.);
#8339=ORIENTED_EDGE('',*,*,#5710,.F.);
#8340=ORIENTED_EDGE('',*,*,#5711,.T.);
#8341=ORIENTED_EDGE('',*,*,#5707,.T.);
#8342=ORIENTED_EDGE('',*,*,#5712,.T.);
#8343=ORIENTED_EDGE('',*,*,#5679,.F.);
#8344=ORIENTED_EDGE('',*,*,#5713,.T.);
#8345=ORIENTED_EDGE('',*,*,#5710,.T.);
#8346=ORIENTED_EDGE('',*,*,#5714,.T.);
#8347=ORIENTED_EDGE('',*,*,#5715,.F.);
#8348=ORIENTED_EDGE('',*,*,#5702,.F.);
#8349=ORIENTED_EDGE('',*,*,#5716,.F.);
#8350=ORIENTED_EDGE('',*,*,#5685,.F.);
#8351=ORIENTED_EDGE('',*,*,#5716,.T.);
#8352=ORIENTED_EDGE('',*,*,#5705,.F.);
#8353=ORIENTED_EDGE('',*,*,#5717,.F.);
#8354=ORIENTED_EDGE('',*,*,#5686,.F.);
#8355=ORIENTED_EDGE('',*,*,#5715,.T.);
#8356=ORIENTED_EDGE('',*,*,#5684,.F.);
#8357=ORIENTED_EDGE('',*,*,#5718,.F.);
#8358=ORIENTED_EDGE('',*,*,#5699,.F.);
#8359=ORIENTED_EDGE('',*,*,#5717,.T.);
#8360=ORIENTED_EDGE('',*,*,#5708,.F.);
#8361=ORIENTED_EDGE('',*,*,#5719,.F.);
#8362=ORIENTED_EDGE('',*,*,#5687,.F.);
#8363=ORIENTED_EDGE('',*,*,#5718,.T.);
#8364=ORIENTED_EDGE('',*,*,#5683,.F.);
#8365=ORIENTED_EDGE('',*,*,#5670,.F.);
#8366=ORIENTED_EDGE('',*,*,#5696,.F.);
#8367=ORIENTED_EDGE('',*,*,#5719,.T.);
#8368=ORIENTED_EDGE('',*,*,#5711,.F.);
#8369=ORIENTED_EDGE('',*,*,#5720,.F.);
#8370=ORIENTED_EDGE('',*,*,#5681,.F.);
#8371=ORIENTED_EDGE('',*,*,#5720,.T.);
#8372=ORIENTED_EDGE('',*,*,#5713,.F.);
#8373=ORIENTED_EDGE('',*,*,#5668,.T.);
#8374=ORIENTED_EDGE('',*,*,#5682,.F.);
#8375=ORIENTED_EDGE('',*,*,#5721,.F.);
#8376=ORIENTED_EDGE('',*,*,#5692,.F.);
#8377=ORIENTED_EDGE('',*,*,#5722,.F.);
#8378=ORIENTED_EDGE('',*,*,#5709,.F.);
#8379=ORIENTED_EDGE('',*,*,#5722,.T.);
#8380=ORIENTED_EDGE('',*,*,#5691,.F.);
#8381=ORIENTED_EDGE('',*,*,#5723,.F.);
#8382=ORIENTED_EDGE('',*,*,#5712,.F.);
#8383=ORIENTED_EDGE('',*,*,#5721,.T.);
#8384=ORIENTED_EDGE('',*,*,#5706,.F.);
#8385=ORIENTED_EDGE('',*,*,#5724,.F.);
#8386=ORIENTED_EDGE('',*,*,#5693,.F.);
#8387=ORIENTED_EDGE('',*,*,#5723,.T.);
#8388=ORIENTED_EDGE('',*,*,#5690,.F.);
#8389=ORIENTED_EDGE('',*,*,#5661,.F.);
#8390=ORIENTED_EDGE('',*,*,#5714,.F.);
#8391=ORIENTED_EDGE('',*,*,#5724,.T.);
#8392=ORIENTED_EDGE('',*,*,#5703,.F.);
#8393=ORIENTED_EDGE('',*,*,#5725,.F.);
#8394=ORIENTED_EDGE('',*,*,#5694,.F.);
#8395=ORIENTED_EDGE('',*,*,#5725,.T.);
#8396=ORIENTED_EDGE('',*,*,#5700,.F.);
#8397=ORIENTED_EDGE('',*,*,#5726,.F.);
#8398=ORIENTED_EDGE('',*,*,#5688,.F.);
#8399=ORIENTED_EDGE('',*,*,#5663,.T.);
#8400=ORIENTED_EDGE('',*,*,#5689,.F.);
#8401=ORIENTED_EDGE('',*,*,#5726,.T.);
#8402=ORIENTED_EDGE('',*,*,#5697,.F.);
#8403=SPHERICAL_SURFACE('',#9072,4.);
#8404=SPHERICAL_SURFACE('',#9077,4.);
#8405=SPHERICAL_SURFACE('',#9113,4.);
#8406=SPHERICAL_SURFACE('',#9118,4.);
#8407=SPHERICAL_SURFACE('',#9690,0.5);
#8408=SPHERICAL_SURFACE('',#9694,0.5);
#8409=SPHERICAL_SURFACE('',#9813,1.2);
#8410=SPHERICAL_SURFACE('',#9816,1.2);
#8411=SPHERICAL_SURFACE('',#9825,4.);
#8412=SPHERICAL_SURFACE('',#9830,4.);
#8413=ADVANCED_FACE('',(#2063),#8403,.T.);
#8414=ADVANCED_FACE('',(#2064),#1857,.T.);
#8415=ADVANCED_FACE('',(#2065),#8404,.T.);
#8416=ADVANCED_FACE('',(#2066,#722),#759,.T.);
#8417=ADVANCED_FACE('',(#2067,#723),#760,.T.);
#8418=ADVANCED_FACE('',(#2068),#606,.T.);
#8419=ADVANCED_FACE('',(#2069),#607,.T.);
#8420=ADVANCED_FACE('',(#2070),#608,.T.);
#8421=ADVANCED_FACE('',(#2071),#609,.T.);
#8422=ADVANCED_FACE('',(#2072),#1858,.T.);
#8423=ADVANCED_FACE('',(#2073),#526,.F.);
#8424=ADVANCED_FACE('',(#2074),#527,.F.);
#8425=ADVANCED_FACE('',(#2075),#528,.F.);
#8426=ADVANCED_FACE('',(#2076),#1859,.T.);
#8427=ADVANCED_FACE('',(#2077),#529,.F.);
#8428=ADVANCED_FACE('',(#2078),#530,.F.);
#8429=ADVANCED_FACE('',(#2079),#531,.F.);
#8430=ADVANCED_FACE('',(#2080),#761,.F.);
#8431=ADVANCED_FACE('',(#2081),#762,.T.);
#8432=ADVANCED_FACE('',(#2082),#8405,.T.);
#8433=ADVANCED_FACE('',(#2083),#1860,.T.);
#8434=ADVANCED_FACE('',(#2084),#8406,.T.);
#8435=ADVANCED_FACE('',(#2085,#724),#763,.T.);
#8436=ADVANCED_FACE('',(#2086,#725),#764,.T.);
#8437=ADVANCED_FACE('',(#2087),#1861,.T.);
#8438=ADVANCED_FACE('',(#2088),#610,.T.);
#8439=ADVANCED_FACE('',(#2089),#611,.T.);
#8440=ADVANCED_FACE('',(#2090),#612,.F.);
#8441=ADVANCED_FACE('',(#2091),#613,.F.);
#8442=ADVANCED_FACE('',(#2092),#137,.T.);
#8443=ADVANCED_FACE('',(#2093),#138,.T.);
#8444=ADVANCED_FACE('',(#2094),#1862,.F.);
#8445=ADVANCED_FACE('',(#2095),#1863,.F.);
#8446=ADVANCED_FACE('',(#2096),#1864,.T.);
#8447=ADVANCED_FACE('',(#2097),#1865,.T.);
#8448=ADVANCED_FACE('',(#2098),#1866,.F.);
#8449=ADVANCED_FACE('',(#2099),#1867,.F.);
#8450=ADVANCED_FACE('',(#2100),#1868,.F.);
#8451=ADVANCED_FACE('',(#2101),#1869,.F.);
#8452=ADVANCED_FACE('',(#2102),#1870,.F.);
#8453=ADVANCED_FACE('',(#2103),#1871,.F.);
#8454=ADVANCED_FACE('',(#2104),#1872,.F.);
#8455=ADVANCED_FACE('',(#2105),#1873,.F.);
#8456=ADVANCED_FACE('',(#2106),#1874,.F.);
#8457=ADVANCED_FACE('',(#2107),#1875,.F.);
#8458=ADVANCED_FACE('',(#2108),#124,.T.);
#8459=ADVANCED_FACE('',(#2109),#125,.T.);
#8460=ADVANCED_FACE('',(#2110),#126,.T.);
#8461=ADVANCED_FACE('',(#2111),#127,.T.);
#8462=ADVANCED_FACE('',(#2112),#128,.T.);
#8463=ADVANCED_FACE('',(#2113),#129,.T.);
#8464=ADVANCED_FACE('',(#2114,#726),#765,.F.);
#8465=ADVANCED_FACE('',(#2115),#532,.F.);
#8466=ADVANCED_FACE('',(#2116),#533,.F.);
#8467=ADVANCED_FACE('',(#2117),#534,.F.);
#8468=ADVANCED_FACE('',(#2118),#535,.F.);
#8469=ADVANCED_FACE('',(#2119),#536,.F.);
#8470=ADVANCED_FACE('',(#2120),#537,.F.);
#8471=ADVANCED_FACE('',(#2121),#538,.F.);
#8472=ADVANCED_FACE('',(#2122),#539,.F.);
#8473=ADVANCED_FACE('',(#2123),#540,.F.);
#8474=ADVANCED_FACE('',(#2124),#541,.F.);
#8475=ADVANCED_FACE('',(#2125),#542,.F.);
#8476=ADVANCED_FACE('',(#2126),#543,.F.);
#8477=ADVANCED_FACE('',(#2127),#1876,.F.);
#8478=ADVANCED_FACE('',(#2128),#1877,.F.);
#8479=ADVANCED_FACE('',(#2129),#1878,.F.);
#8480=ADVANCED_FACE('',(#2130),#1879,.F.);
#8481=ADVANCED_FACE('',(#2131),#1880,.F.);
#8482=ADVANCED_FACE('',(#2132),#1881,.F.);
#8483=ADVANCED_FACE('',(#2133),#1882,.F.);
#8484=ADVANCED_FACE('',(#2134),#766,.F.);
#8485=ADVANCED_FACE('',(#2135),#130,.T.);
#8486=ADVANCED_FACE('',(#2136),#544,.F.);
#8487=ADVANCED_FACE('',(#2137),#545,.F.);
#8488=ADVANCED_FACE('',(#2138),#767,.F.);
#8489=ADVANCED_FACE('',(#2139),#768,.F.);
#8490=ADVANCED_FACE('',(#2140),#769,.F.);
#8491=ADVANCED_FACE('',(#2141),#770,.F.);
#8492=ADVANCED_FACE('',(#2142),#771,.F.);
#8493=ADVANCED_FACE('',(#2143),#1883,.F.);
#8494=ADVANCED_FACE('',(#2144),#131,.F.);
#8495=ADVANCED_FACE('',(#2145),#772,.F.);
#8496=ADVANCED_FACE('',(#2146),#773,.F.);
#8497=ADVANCED_FACE('',(#2147,#727),#774,.T.);
#8498=ADVANCED_FACE('',(#2148,#728),#775,.F.);
#8499=ADVANCED_FACE('',(#2149),#1884,.F.);
#8500=ADVANCED_FACE('',(#2150),#546,.T.);
#8501=ADVANCED_FACE('',(#2151),#547,.T.);
#8502=ADVANCED_FACE('',(#2152),#132,.T.);
#8503=ADVANCED_FACE('',(#2153,#729),#776,.T.);
#8504=ADVANCED_FACE('',(#2154),#548,.F.);
#8505=ADVANCED_FACE('',(#2155),#1885,.F.);
#8506=ADVANCED_FACE('',(#2156),#777,.T.);
#8507=ADVANCED_FACE('',(#2157),#778,.T.);
#8508=ADVANCED_FACE('',(#2158),#1886,.T.);
#8509=ADVANCED_FACE('',(#2159),#779,.T.);
#8510=ADVANCED_FACE('',(#2160),#780,.T.);
#8511=ADVANCED_FACE('',(#2161),#1887,.F.);
#8512=ADVANCED_FACE('',(#2162),#781,.T.);
#8513=ADVANCED_FACE('',(#2163),#782,.T.);
#8514=ADVANCED_FACE('',(#2164),#783,.T.);
#8515=ADVANCED_FACE('',(#2165),#784,.F.);
#8516=ADVANCED_FACE('',(#2166),#139,.T.);
#8517=ADVANCED_FACE('',(#2167),#140,.T.);
#8518=ADVANCED_FACE('',(#2168),#785,.F.);
#8519=ADVANCED_FACE('',(#2169),#786,.F.);
#8520=ADVANCED_FACE('',(#2170),#787,.F.);
#8521=ADVANCED_FACE('',(#2171),#788,.F.);
#8522=ADVANCED_FACE('',(#2172),#789,.F.);
#8523=ADVANCED_FACE('',(#2173),#790,.F.);
#8524=ADVANCED_FACE('',(#2174),#791,.F.);
#8525=ADVANCED_FACE('',(#2175),#792,.F.);
#8526=ADVANCED_FACE('',(#2176),#793,.F.);
#8527=ADVANCED_FACE('',(#2177),#794,.F.);
#8528=ADVANCED_FACE('',(#2178),#795,.F.);
#8529=ADVANCED_FACE('',(#2179),#796,.F.);
#8530=ADVANCED_FACE('',(#2180),#797,.F.);
#8531=ADVANCED_FACE('',(#2181),#798,.F.);
#8532=ADVANCED_FACE('',(#2182),#799,.F.);
#8533=ADVANCED_FACE('',(#2183),#800,.F.);
#8534=ADVANCED_FACE('',(#2184),#801,.F.);
#8535=ADVANCED_FACE('',(#2185),#802,.F.);
#8536=ADVANCED_FACE('',(#2186),#803,.F.);
#8537=ADVANCED_FACE('',(#2187),#1888,.F.);
#8538=ADVANCED_FACE('',(#2188),#614,.F.);
#8539=ADVANCED_FACE('',(#2189),#1889,.F.);
#8540=ADVANCED_FACE('',(#2190),#615,.F.);
#8541=ADVANCED_FACE('',(#2191),#549,.T.);
#8542=ADVANCED_FACE('',(#2192),#550,.T.);
#8543=ADVANCED_FACE('',(#2193),#551,.T.);
#8544=ADVANCED_FACE('',(#2194),#552,.T.);
#8545=ADVANCED_FACE('',(#2195),#553,.T.);
#8546=ADVANCED_FACE('',(#2196),#554,.T.);
#8547=ADVANCED_FACE('',(#2197),#804,.T.);
#8548=ADVANCED_FACE('',(#2198),#1890,.F.);
#8549=ADVANCED_FACE('',(#2199),#805,.F.);
#8550=ADVANCED_FACE('',(#2200),#806,.T.);
#8551=ADVANCED_FACE('',(#2201),#1891,.T.);
#8552=ADVANCED_FACE('',(#2202),#616,.T.);
#8553=ADVANCED_FACE('',(#2203),#1892,.T.);
#8554=ADVANCED_FACE('',(#2204),#617,.T.);
#8555=ADVANCED_FACE('',(#2205),#1893,.T.);
#8556=ADVANCED_FACE('',(#2206),#618,.T.);
#8557=ADVANCED_FACE('',(#2207),#1894,.T.);
#8558=ADVANCED_FACE('',(#2208),#619,.T.);
#8559=ADVANCED_FACE('',(#2209),#1895,.T.);
#8560=ADVANCED_FACE('',(#2210),#555,.T.);
#8561=ADVANCED_FACE('',(#2211),#1896,.T.);
#8562=ADVANCED_FACE('',(#2212),#556,.T.);
#8563=ADVANCED_FACE('',(#2213),#1897,.T.);
#8564=ADVANCED_FACE('',(#2214),#620,.T.);
#8565=ADVANCED_FACE('',(#2215),#1898,.T.);
#8566=ADVANCED_FACE('',(#2216),#621,.T.);
#8567=ADVANCED_FACE('',(#2217),#1899,.T.);
#8568=ADVANCED_FACE('',(#2218),#557,.F.);
#8569=ADVANCED_FACE('',(#2219),#558,.F.);
#8570=ADVANCED_FACE('',(#2220),#559,.F.);
#8571=ADVANCED_FACE('',(#2221),#560,.F.);
#8572=ADVANCED_FACE('',(#2222),#807,.T.);
#8573=ADVANCED_FACE('',(#2223),#561,.F.);
#8574=ADVANCED_FACE('',(#2224),#562,.F.);
#8575=ADVANCED_FACE('',(#2225),#563,.F.);
#8576=ADVANCED_FACE('',(#2226),#564,.F.);
#8577=ADVANCED_FACE('',(#2227),#565,.F.);
#8578=ADVANCED_FACE('',(#2228),#566,.F.);
#8579=ADVANCED_FACE('',(#2229),#567,.F.);
#8580=ADVANCED_FACE('',(#2230),#568,.F.);
#8581=ADVANCED_FACE('',(#2231),#569,.F.);
#8582=ADVANCED_FACE('',(#2232),#570,.F.);
#8583=ADVANCED_FACE('',(#2233),#571,.F.);
#8584=ADVANCED_FACE('',(#2234),#572,.F.);
#8585=ADVANCED_FACE('',(#2235),#573,.F.);
#8586=ADVANCED_FACE('',(#2236),#574,.F.);
#8587=ADVANCED_FACE('',(#2237),#575,.F.);
#8588=ADVANCED_FACE('',(#2238),#576,.F.);
#8589=ADVANCED_FACE('',(#2239),#577,.F.);
#8590=ADVANCED_FACE('',(#2240),#578,.F.);
#8591=ADVANCED_FACE('',(#2241),#579,.F.);
#8592=ADVANCED_FACE('',(#2242),#580,.F.);
#8593=ADVANCED_FACE('',(#2243),#581,.F.);
#8594=ADVANCED_FACE('',(#2244),#582,.F.);
#8595=ADVANCED_FACE('',(#2245),#1900,.T.);
#8596=ADVANCED_FACE('',(#2246),#583,.T.);
#8597=ADVANCED_FACE('',(#2247),#584,.T.);
#8598=ADVANCED_FACE('',(#2248),#622,.T.);
#8599=ADVANCED_FACE('',(#2249),#623,.T.);
#8600=ADVANCED_FACE('',(#2250),#624,.T.);
#8601=ADVANCED_FACE('',(#2251),#625,.T.);
#8602=ADVANCED_FACE('',(#2252),#626,.T.);
#8603=ADVANCED_FACE('',(#2253),#627,.T.);
#8604=ADVANCED_FACE('',(#2254),#585,.T.);
#8605=ADVANCED_FACE('',(#2255),#586,.T.);
#8606=ADVANCED_FACE('',(#2256),#1901,.T.);
#8607=ADVANCED_FACE('',(#2257),#1902,.T.);
#8608=ADVANCED_FACE('',(#2258),#1903,.T.);
#8609=ADVANCED_FACE('',(#2259),#1904,.T.);
#8610=ADVANCED_FACE('',(#2260),#1905,.T.);
#8611=ADVANCED_FACE('',(#2261),#1906,.T.);
#8612=ADVANCED_FACE('',(#2262),#1907,.T.);
#8613=ADVANCED_FACE('',(#2263),#1908,.T.);
#8614=ADVANCED_FACE('',(#2264),#1909,.T.);
#8615=ADVANCED_FACE('',(#2265),#1910,.T.);
#8616=ADVANCED_FACE('',(#2266),#1911,.T.);
#8617=ADVANCED_FACE('',(#2267),#1912,.T.);
#8618=ADVANCED_FACE('',(#2268),#1913,.T.);
#8619=ADVANCED_FACE('',(#2269),#1914,.T.);
#8620=ADVANCED_FACE('',(#2270),#1915,.T.);
#8621=ADVANCED_FACE('',(#2271),#1916,.T.);
#8622=ADVANCED_FACE('',(#2272),#1917,.T.);
#8623=ADVANCED_FACE('',(#2273),#1918,.T.);
#8624=ADVANCED_FACE('',(#2274),#1919,.T.);
#8625=ADVANCED_FACE('',(#2275),#1920,.T.);
#8626=ADVANCED_FACE('',(#2276),#1921,.T.);
#8627=ADVANCED_FACE('',(#2277),#1922,.T.);
#8628=ADVANCED_FACE('',(#2278),#1923,.T.);
#8629=ADVANCED_FACE('',(#2279),#1924,.T.);
#8630=ADVANCED_FACE('',(#2280),#1925,.T.);
#8631=ADVANCED_FACE('',(#2281),#1926,.T.);
#8632=ADVANCED_FACE('',(#2282),#1927,.T.);
#8633=ADVANCED_FACE('',(#2283),#1928,.T.);
#8634=ADVANCED_FACE('',(#2284),#1929,.T.);
#8635=ADVANCED_FACE('',(#2285),#1930,.T.);
#8636=ADVANCED_FACE('',(#2286),#1931,.T.);
#8637=ADVANCED_FACE('',(#2287),#1932,.T.);
#8638=ADVANCED_FACE('',(#2288),#1933,.T.);
#8639=ADVANCED_FACE('',(#2289),#1934,.T.);
#8640=ADVANCED_FACE('',(#2290),#1935,.T.);
#8641=ADVANCED_FACE('',(#2291),#1936,.T.);
#8642=ADVANCED_FACE('',(#2292),#1937,.T.);
#8643=ADVANCED_FACE('',(#2293),#1938,.T.);
#8644=ADVANCED_FACE('',(#2294),#1939,.T.);
#8645=ADVANCED_FACE('',(#2295),#1940,.T.);
#8646=ADVANCED_FACE('',(#2296),#1941,.T.);
#8647=ADVANCED_FACE('',(#2297),#141,.T.);
#8648=ADVANCED_FACE('',(#2298),#1942,.F.);
#8649=ADVANCED_FACE('',(#2299),#1943,.F.);
#8650=ADVANCED_FACE('',(#2300),#1944,.F.);
#8651=ADVANCED_FACE('',(#2301),#1945,.F.);
#8652=ADVANCED_FACE('',(#2302),#1946,.F.);
#8653=ADVANCED_FACE('',(#2303),#1947,.F.);
#8654=ADVANCED_FACE('',(#2304),#1948,.F.);
#8655=ADVANCED_FACE('',(#2305),#1949,.F.);
#8656=ADVANCED_FACE('',(#2306),#1950,.F.);
#8657=ADVANCED_FACE('',(#2307),#1951,.F.);
#8658=ADVANCED_FACE('',(#2308),#628,.T.);
#8659=ADVANCED_FACE('',(#2309),#629,.T.);
#8660=ADVANCED_FACE('',(#2310),#1952,.T.);
#8661=ADVANCED_FACE('',(#2311),#1953,.T.);
#8662=ADVANCED_FACE('',(#2312),#1954,.T.);
#8663=ADVANCED_FACE('',(#2313),#1955,.T.);
#8664=ADVANCED_FACE('',(#2314),#1956,.T.);
#8665=ADVANCED_FACE('',(#2315),#1957,.T.);
#8666=ADVANCED_FACE('',(#2316),#1958,.T.);
#8667=ADVANCED_FACE('',(#2317),#1959,.T.);
#8668=ADVANCED_FACE('',(#2318),#1960,.T.);
#8669=ADVANCED_FACE('',(#2319),#1961,.T.);
#8670=ADVANCED_FACE('',(#2320),#1962,.T.);
#8671=ADVANCED_FACE('',(#2321),#1963,.T.);
#8672=ADVANCED_FACE('',(#2322),#1964,.T.);
#8673=ADVANCED_FACE('',(#2323),#1965,.T.);
#8674=ADVANCED_FACE('',(#2324),#1966,.T.);
#8675=ADVANCED_FACE('',(#2325),#1967,.T.);
#8676=ADVANCED_FACE('',(#2326),#1968,.T.);
#8677=ADVANCED_FACE('',(#2327),#1969,.T.);
#8678=ADVANCED_FACE('',(#2328),#1970,.T.);
#8679=ADVANCED_FACE('',(#2329),#1971,.T.);
#8680=ADVANCED_FACE('',(#2330),#1972,.T.);
#8681=ADVANCED_FACE('',(#2331),#1973,.T.);
#8682=ADVANCED_FACE('',(#2332),#1974,.T.);
#8683=ADVANCED_FACE('',(#2333),#1975,.T.);
#8684=ADVANCED_FACE('',(#2334),#1976,.T.);
#8685=ADVANCED_FACE('',(#2335),#1977,.T.);
#8686=ADVANCED_FACE('',(#2336,#730),#808,.T.);
#8687=ADVANCED_FACE('',(#2337),#809,.T.);
#8688=ADVANCED_FACE('',(#2338),#1978,.T.);
#8689=ADVANCED_FACE('',(#2339),#810,.T.);
#8690=ADVANCED_FACE('',(#2340),#587,.F.);
#8691=ADVANCED_FACE('',(#2341),#588,.F.);
#8692=ADVANCED_FACE('',(#2342),#589,.F.);
#8693=ADVANCED_FACE('',(#2343),#1979,.F.);
#8694=ADVANCED_FACE('',(#2344),#1980,.F.);
#8695=ADVANCED_FACE('',(#2345),#1981,.F.);
#8696=ADVANCED_FACE('',(#2346),#1982,.F.);
#8697=ADVANCED_FACE('',(#2347),#1983,.F.);
#8698=ADVANCED_FACE('',(#2348),#1984,.F.);
#8699=ADVANCED_FACE('',(#2349),#1985,.F.);
#8700=ADVANCED_FACE('',(#2350),#1986,.F.);
#8701=ADVANCED_FACE('',(#2351),#1987,.F.);
#8702=ADVANCED_FACE('',(#2352),#1988,.F.);
#8703=ADVANCED_FACE('',(#2353),#1989,.F.);
#8704=ADVANCED_FACE('',(#2354),#1990,.F.);
#8705=ADVANCED_FACE('',(#2355),#1991,.F.);
#8706=ADVANCED_FACE('',(#2356),#1992,.F.);
#8707=ADVANCED_FACE('',(#2357),#1993,.F.);
#8708=ADVANCED_FACE('',(#2358),#1994,.F.);
#8709=ADVANCED_FACE('',(#2359),#811,.T.);
#8710=ADVANCED_FACE('',(#2360),#1995,.T.);
#8711=ADVANCED_FACE('',(#2361),#1996,.T.);
#8712=ADVANCED_FACE('',(#2362),#1997,.T.);
#8713=ADVANCED_FACE('',(#2363),#630,.T.);
#8714=ADVANCED_FACE('',(#2364),#631,.T.);
#8715=ADVANCED_FACE('',(#2365),#1998,.F.);
#8716=ADVANCED_FACE('',(#2366),#1999,.F.);
#8717=ADVANCED_FACE('',(#2367),#2000,.F.);
#8718=ADVANCED_FACE('',(#2368),#632,.F.);
#8719=ADVANCED_FACE('',(#2369),#633,.F.);
#8720=ADVANCED_FACE('',(#2370),#2001,.F.);
#8721=ADVANCED_FACE('',(#2371),#2002,.T.);
#8722=ADVANCED_FACE('',(#2372),#2003,.F.);
#8723=ADVANCED_FACE('',(#2373),#2004,.F.);
#8724=ADVANCED_FACE('',(#2374),#2005,.F.);
#8725=ADVANCED_FACE('',(#2375),#2006,.F.);
#8726=ADVANCED_FACE('',(#2376,#731,#732),#812,.F.);
#8727=ADVANCED_FACE('',(#2377,#733,#734),#813,.T.);
#8728=ADVANCED_FACE('',(#2378),#814,.F.);
#8729=ADVANCED_FACE('',(#2379),#2007,.T.);
#8730=ADVANCED_FACE('',(#2380),#2008,.T.);
#8731=ADVANCED_FACE('',(#2381),#2009,.F.);
#8732=ADVANCED_FACE('',(#2382),#815,.F.);
#8733=ADVANCED_FACE('',(#2383),#2010,.T.);
#8734=ADVANCED_FACE('',(#2384),#2011,.F.);
#8735=ADVANCED_FACE('',(#2385),#816,.F.);
#8736=ADVANCED_FACE('',(#2386),#142,.T.);
#8737=ADVANCED_FACE('',(#2387),#143,.T.);
#8738=ADVANCED_FACE('',(#2388),#817,.T.);
#8739=ADVANCED_FACE('',(#2389),#144,.T.);
#8740=ADVANCED_FACE('',(#2390),#145,.T.);
#8741=ADVANCED_FACE('',(#2391),#818,.T.);
#8742=ADVANCED_FACE('',(#2392),#146,.T.);
#8743=ADVANCED_FACE('',(#2393),#147,.T.);
#8744=ADVANCED_FACE('',(#2394),#819,.T.);
#8745=ADVANCED_FACE('',(#2395),#634,.F.);
#8746=ADVANCED_FACE('',(#2396),#635,.F.);
#8747=ADVANCED_FACE('',(#2397),#636,.F.);
#8748=ADVANCED_FACE('',(#2398),#637,.F.);
#8749=ADVANCED_FACE('',(#2399),#2012,.F.);
#8750=ADVANCED_FACE('',(#2400),#820,.F.);
#8751=ADVANCED_FACE('',(#2401,#735),#821,.T.);
#8752=ADVANCED_FACE('',(#2402,#736),#822,.F.);
#8753=ADVANCED_FACE('',(#2403),#2013,.T.);
#8754=ADVANCED_FACE('',(#2404),#823,.F.);
#8755=ADVANCED_FACE('',(#2405),#824,.F.);
#8756=ADVANCED_FACE('',(#2406),#825,.F.);
#8757=ADVANCED_FACE('',(#2407),#826,.F.);
#8758=ADVANCED_FACE('',(#2408),#827,.F.);
#8759=ADVANCED_FACE('',(#2409),#828,.F.);
#8760=ADVANCED_FACE('',(#2410),#829,.F.);
#8761=ADVANCED_FACE('',(#2411),#830,.F.);
#8762=ADVANCED_FACE('',(#2412),#831,.F.);
#8763=ADVANCED_FACE('',(#2413),#832,.F.);
#8764=ADVANCED_FACE('',(#2414),#833,.F.);
#8765=ADVANCED_FACE('',(#2415),#834,.F.);
#8766=ADVANCED_FACE('',(#2416),#835,.F.);
#8767=ADVANCED_FACE('',(#2417),#836,.F.);
#8768=ADVANCED_FACE('',(#2418),#837,.F.);
#8769=ADVANCED_FACE('',(#2419),#838,.F.);
#8770=ADVANCED_FACE('',(#2420),#839,.F.);
#8771=ADVANCED_FACE('',(#2421),#840,.F.);
#8772=ADVANCED_FACE('',(#2422),#841,.F.);
#8773=ADVANCED_FACE('',(#2423),#638,.T.);
#8774=ADVANCED_FACE('',(#2424),#639,.T.);
#8775=ADVANCED_FACE('',(#2425),#2014,.T.);
#8776=ADVANCED_FACE('',(#2426),#640,.T.);
#8777=ADVANCED_FACE('',(#2427),#641,.T.);
#8778=ADVANCED_FACE('',(#2428),#590,.T.);
#8779=ADVANCED_FACE('',(#2429),#591,.T.);
#8780=ADVANCED_FACE('',(#2430),#642,.T.);
#8781=ADVANCED_FACE('',(#2431),#643,.T.);
#8782=ADVANCED_FACE('',(#2432),#2015,.T.);
#8783=ADVANCED_FACE('',(#2433),#644,.T.);
#8784=ADVANCED_FACE('',(#2434),#645,.T.);
#8785=ADVANCED_FACE('',(#2435),#592,.T.);
#8786=ADVANCED_FACE('',(#2436),#593,.T.);
#8787=ADVANCED_FACE('',(#2437),#594,.T.);
#8788=ADVANCED_FACE('',(#2438),#595,.T.);
#8789=ADVANCED_FACE('',(#2439),#646,.T.);
#8790=ADVANCED_FACE('',(#2440),#647,.T.);
#8791=ADVANCED_FACE('',(#2441),#648,.T.);
#8792=ADVANCED_FACE('',(#2442),#8407,.T.);
#8793=ADVANCED_FACE('',(#2443),#2016,.T.);
#8794=ADVANCED_FACE('',(#2444),#8408,.T.);
#8795=ADVANCED_FACE('',(#2445),#649,.T.);
#8796=ADVANCED_FACE('',(#2446),#650,.T.);
#8797=ADVANCED_FACE('',(#2447),#651,.T.);
#8798=ADVANCED_FACE('',(#2448),#596,.T.);
#8799=ADVANCED_FACE('',(#2449),#597,.T.);
#8800=ADVANCED_FACE('',(#2450),#652,.T.);
#8801=ADVANCED_FACE('',(#2451),#653,.T.);
#8802=ADVANCED_FACE('',(#2452),#654,.T.);
#8803=ADVANCED_FACE('',(#2453),#655,.T.);
#8804=ADVANCED_FACE('',(#2454),#2017,.F.);
#8805=ADVANCED_FACE('',(#2455),#2018,.F.);
#8806=ADVANCED_FACE('',(#2456),#2019,.F.);
#8807=ADVANCED_FACE('',(#2457),#2020,.F.);
#8808=ADVANCED_FACE('',(#2458),#2021,.F.);
#8809=ADVANCED_FACE('',(#2459),#2022,.F.);
#8810=ADVANCED_FACE('',(#2460),#2023,.F.);
#8811=ADVANCED_FACE('',(#2461),#2024,.F.);
#8812=ADVANCED_FACE('',(#2462),#2025,.F.);
#8813=ADVANCED_FACE('',(#2463),#2026,.T.);
#8814=ADVANCED_FACE('',(#2464),#842,.F.);
#8815=ADVANCED_FACE('',(#2465),#843,.F.);
#8816=ADVANCED_FACE('',(#2466),#844,.F.);
#8817=ADVANCED_FACE('',(#2467),#845,.F.);
#8818=ADVANCED_FACE('',(#2468,#737,#738),#846,.F.);
#8819=ADVANCED_FACE('',(#2469,#739,#740),#847,.T.);
#8820=ADVANCED_FACE('',(#2470),#848,.F.);
#8821=ADVANCED_FACE('',(#2471),#2027,.F.);
#8822=ADVANCED_FACE('',(#2472),#849,.F.);
#8823=ADVANCED_FACE('',(#2473),#850,.F.);
#8824=ADVANCED_FACE('',(#2474),#851,.F.);
#8825=ADVANCED_FACE('',(#2475),#852,.T.);
#8826=ADVANCED_FACE('',(#2476,#741),#853,.T.);
#8827=ADVANCED_FACE('',(#2477,#742),#854,.F.);
#8828=ADVANCED_FACE('',(#2478),#855,.T.);
#8829=ADVANCED_FACE('',(#2479),#856,.F.);
#8830=ADVANCED_FACE('',(#2480,#743,#744),#857,.T.);
#8831=ADVANCED_FACE('',(#2481,#745,#746),#858,.F.);
#8832=ADVANCED_FACE('',(#2482),#859,.T.);
#8833=ADVANCED_FACE('',(#2483),#2028,.T.);
#8834=ADVANCED_FACE('',(#2484),#860,.T.);
#8835=ADVANCED_FACE('',(#2485),#861,.F.);
#8836=ADVANCED_FACE('',(#2486),#862,.F.);
#8837=ADVANCED_FACE('',(#2487),#863,.T.);
#8838=ADVANCED_FACE('',(#2488),#864,.F.);
#8839=ADVANCED_FACE('',(#2489),#865,.T.);
#8840=ADVANCED_FACE('',(#2490),#656,.T.);
#8841=ADVANCED_FACE('',(#2491),#2029,.T.);
#8842=ADVANCED_FACE('',(#2492),#657,.T.);
#8843=ADVANCED_FACE('',(#2493),#2030,.T.);
#8844=ADVANCED_FACE('',(#2494),#2031,.T.);
#8845=ADVANCED_FACE('',(#2495),#2032,.T.);
#8846=ADVANCED_FACE('',(#2496),#2033,.T.);
#8847=ADVANCED_FACE('',(#2497),#2034,.T.);
#8848=ADVANCED_FACE('',(#2498),#658,.T.);
#8849=ADVANCED_FACE('',(#2499),#2035,.T.);
#8850=ADVANCED_FACE('',(#2500),#2036,.T.);
#8851=ADVANCED_FACE('',(#2501),#2037,.T.);
#8852=ADVANCED_FACE('',(#2502),#659,.T.);
#8853=ADVANCED_FACE('',(#2503),#2038,.T.);
#8854=ADVANCED_FACE('',(#2504),#2039,.T.);
#8855=ADVANCED_FACE('',(#2505),#866,.F.);
#8856=ADVANCED_FACE('',(#2506,#747),#867,.F.);
#8857=ADVANCED_FACE('',(#2507,#748),#868,.F.);
#8858=ADVANCED_FACE('',(#2508),#8409,.T.);
#8859=ADVANCED_FACE('',(#2509),#8410,.T.);
#8860=ADVANCED_FACE('',(#2510),#2040,.T.);
#8861=ADVANCED_FACE('',(#2511,#749),#869,.F.);
#8862=ADVANCED_FACE('',(#2512,#750),#870,.F.);
#8863=ADVANCED_FACE('',(#2513),#8411,.T.);
#8864=ADVANCED_FACE('',(#2514),#2041,.T.);
#8865=ADVANCED_FACE('',(#2515),#8412,.T.);
#8866=ADVANCED_FACE('',(#2516,#751),#871,.T.);
#8867=ADVANCED_FACE('',(#2517,#752),#872,.T.);
#8868=ADVANCED_FACE('',(#2518),#2042,.F.);
#8869=ADVANCED_FACE('',(#2519),#2043,.T.);
#8870=ADVANCED_FACE('',(#2520),#2044,.F.);
#8871=ADVANCED_FACE('',(#2521),#873,.F.);
#8872=ADVANCED_FACE('',(#2522),#133,.F.);
#8873=ADVANCED_FACE('',(#2523),#2045,.F.);
#8874=ADVANCED_FACE('',(#2524,#753),#874,.F.);
#8875=ADVANCED_FACE('',(#2525,#754),#875,.T.);
#8876=ADVANCED_FACE('',(#2526),#134,.F.);
#8877=ADVANCED_FACE('',(#2527),#135,.F.);
#8878=ADVANCED_FACE('',(#2528),#2046,.F.);
#8879=ADVANCED_FACE('',(#2529),#876,.T.);
#8880=ADVANCED_FACE('',(#2530),#877,.F.);
#8881=ADVANCED_FACE('',(#2531),#136,.T.);
#8882=ADVANCED_FACE('',(#2532),#598,.T.);
#8883=ADVANCED_FACE('',(#2533),#599,.T.);
#8884=ADVANCED_FACE('',(#2534),#2047,.T.);
#8885=ADVANCED_FACE('',(#2535),#2048,.T.);
#8886=ADVANCED_FACE('',(#2536),#2049,.T.);
#8887=ADVANCED_FACE('',(#2537),#600,.F.);
#8888=ADVANCED_FACE('',(#2538),#601,.F.);
#8889=ADVANCED_FACE('',(#2539),#602,.F.);
#8890=ADVANCED_FACE('',(#2540),#603,.F.);
#8891=ADVANCED_FACE('',(#2541),#604,.F.);
#8892=ADVANCED_FACE('',(#2542),#605,.F.);
#8893=ADVANCED_FACE('',(#2543),#660,.T.);
#8894=ADVANCED_FACE('',(#2544),#661,.T.);
#8895=ADVANCED_FACE('',(#2545),#662,.T.);
#8896=ADVANCED_FACE('',(#2546),#663,.T.);
#8897=ADVANCED_FACE('',(#2547),#664,.T.);
#8898=ADVANCED_FACE('',(#2548),#665,.T.);
#8899=ADVANCED_FACE('',(#2549),#2050,.F.);
#8900=ADVANCED_FACE('',(#2550),#2051,.F.);
#8901=ADVANCED_FACE('',(#2551),#2052,.T.);
#8902=ADVANCED_FACE('',(#2552,#755,#756),#878,.F.);
#8903=ADVANCED_FACE('',(#2553,#757,#758),#879,.T.);
#8904=ADVANCED_FACE('',(#2554),#880,.F.);
#8905=ADVANCED_FACE('',(#2555),#2053,.F.);
#8906=ADVANCED_FACE('',(#2556),#881,.F.);
#8907=ADVANCED_FACE('',(#2557),#2054,.T.);
#8908=ADVANCED_FACE('',(#2558),#882,.F.);
#8909=ADVANCED_FACE('',(#2559),#2055,.T.);
#8910=ADVANCED_FACE('',(#2560),#2056,.F.);
#8911=ADVANCED_FACE('',(#2561),#2057,.T.);
#8912=ADVANCED_FACE('',(#2562),#666,.T.);
#8913=ADVANCED_FACE('',(#2563),#667,.T.);
#8914=ADVANCED_FACE('',(#2564),#2058,.T.);
#8915=ADVANCED_FACE('',(#2565),#2059,.T.);
#8916=ADVANCED_FACE('',(#2566),#668,.T.);
#8917=ADVANCED_FACE('',(#2567),#669,.T.);
#8918=ADVANCED_FACE('',(#2568),#2060,.T.);
#8919=ADVANCED_FACE('',(#2569),#670,.T.);
#8920=ADVANCED_FACE('',(#2570),#671,.T.);
#8921=ADVANCED_FACE('',(#2571),#672,.T.);
#8922=ADVANCED_FACE('',(#2572),#2061,.T.);
#8923=ADVANCED_FACE('',(#2573),#673,.T.);
#8924=ADVANCED_FACE('',(#2574),#2062,.T.);
#8925=CLOSED_SHELL('',(#8413,#8414,#8415,#8416,#8417));
#8926=CLOSED_SHELL('',(#8418,#8419,#8420,#8421,#8422,#8423,#8424,#8425,
#8426,#8427,#8428,#8429,#8430,#8431));
#8927=CLOSED_SHELL('',(#8432,#8433,#8434,#8435,#8436));
#8928=CLOSED_SHELL('',(#8437,#8438,#8439,#8440,#8441,#8442,#8443,#8444,
#8445,#8446,#8447,#8448,#8449,#8450,#8451,#8452,#8453,#8454,#8455,#8456,
#8457,#8458,#8459,#8460,#8461,#8462,#8463,#8464,#8465,#8466,#8467,#8468,
#8469,#8470,#8471,#8472,#8473,#8474,#8475,#8476,#8477,#8478,#8479,#8480,
#8481,#8482,#8483,#8484,#8485,#8486,#8487,#8488,#8489,#8490,#8491,#8492,
#8493,#8494,#8495,#8496,#8497,#8498,#8499,#8500,#8501,#8502,#8503,#8504,
#8505,#8506,#8507,#8508,#8509,#8510,#8511,#8512,#8513,#8514,#8515,#8516,
#8517,#8518,#8519,#8520,#8521,#8522,#8523,#8524,#8525,#8526,#8527,#8528,
#8529,#8530,#8531,#8532,#8533,#8534,#8535,#8536,#8537,#8538,#8539,#8540,
#8541,#8542,#8543,#8544,#8545,#8546,#8547,#8548,#8549,#8550,#8551,#8552,
#8553,#8554,#8555,#8556,#8557,#8558,#8559,#8560,#8561,#8562,#8563,#8564,
#8565,#8566,#8567,#8568,#8569,#8570,#8571,#8572,#8573,#8574,#8575,#8576,
#8577,#8578,#8579,#8580,#8581,#8582,#8583,#8584,#8585,#8586,#8587,#8588,
#8589,#8590,#8591,#8592,#8593,#8594,#8595,#8596,#8597,#8598,#8599,#8600,
#8601,#8602,#8603,#8604,#8605));
#8929=CLOSED_SHELL('',(#8606,#8607,#8608,#8609,#8610,#8611,#8612,#8613,
#8614,#8615,#8616,#8617,#8618,#8619,#8620,#8621,#8622,#8623,#8624,#8625,
#8626,#8627,#8628,#8629,#8630,#8631,#8632,#8633,#8634,#8635,#8636,#8637,
#8638,#8639,#8640,#8641,#8642,#8643,#8644,#8645,#8646,#8647,#8648,#8649,
#8650,#8651,#8652,#8653,#8654,#8655,#8656,#8657,#8658,#8659,#8660,#8661,
#8662,#8663,#8664,#8665,#8666,#8667,#8668,#8669,#8670,#8671,#8672,#8673,
#8674,#8675,#8676,#8677,#8678,#8679,#8680,#8681,#8682,#8683,#8684,#8685,
#8686,#8687,#8688,#8689,#8690,#8691,#8692,#8693,#8694,#8695,#8696,#8697,
#8698,#8699,#8700,#8701,#8702,#8703,#8704,#8705,#8706,#8707,#8708,#8709));
#8930=CLOSED_SHELL('',(#8710,#8711,#8712));
#8931=CLOSED_SHELL('',(#8713,#8714,#8715,#8716,#8717,#8718,#8719,#8720,
#8721,#8722,#8723,#8724,#8725,#8726,#8727,#8728,#8729,#8730,#8731,#8732,
#8733,#8734,#8735,#8736,#8737,#8738,#8739,#8740,#8741,#8742,#8743,#8744,
#8745,#8746,#8747,#8748,#8749,#8750,#8751,#8752,#8753,#8754,#8755,#8756,
#8757,#8758,#8759,#8760,#8761,#8762,#8763,#8764,#8765,#8766,#8767,#8768,
#8769,#8770,#8771,#8772,#8773,#8774,#8775,#8776,#8777,#8778,#8779,#8780,
#8781,#8782,#8783,#8784,#8785,#8786,#8787,#8788,#8789,#8790,#8791,#8792,
#8793,#8794,#8795,#8796,#8797,#8798,#8799));
#8932=CLOSED_SHELL('',(#8800,#8801,#8802,#8803,#8804,#8805,#8806,#8807,
#8808,#8809,#8810,#8811,#8812,#8813,#8814,#8815,#8816,#8817,#8818,#8819,
#8820,#8821,#8822,#8823,#8824,#8825,#8826,#8827,#8828,#8829,#8830,#8831,
#8832,#8833,#8834,#8835,#8836,#8837,#8838,#8839,#8840,#8841,#8842,#8843,
#8844,#8845,#8846,#8847,#8848,#8849,#8850,#8851,#8852,#8853,#8854,#8855,
#8856,#8857));
#8933=CLOSED_SHELL('',(#8858,#8859,#8860,#8861,#8862));
#8934=CLOSED_SHELL('',(#8863,#8864,#8865,#8866,#8867));
#8935=CLOSED_SHELL('',(#8868,#8869,#8870,#8871,#8872,#8873,#8874,#8875,
#8876,#8877,#8878,#8879,#8880,#8881,#8882,#8883,#8884,#8885,#8886,#8887,
#8888,#8889,#8890,#8891,#8892));
#8936=CLOSED_SHELL('',(#8893,#8894,#8895,#8896,#8897,#8898,#8899,#8900,
#8901,#8902,#8903,#8904,#8905,#8906,#8907,#8908,#8909,#8910,#8911,#8912,
#8913,#8914,#8915,#8916,#8917,#8918,#8919,#8920,#8921,#8922,#8923,#8924));
#8937=DERIVED_UNIT_ELEMENT(#8961,1.);
#8938=DERIVED_UNIT_ELEMENT(#47719,-3.);
#8939=DERIVED_UNIT_ELEMENT(#8961,1.);
#8940=DERIVED_UNIT_ELEMENT(#47719,-3.);
#8941=DERIVED_UNIT_ELEMENT(#8961,1.);
#8942=DERIVED_UNIT_ELEMENT(#47719,-3.);
#8943=DERIVED_UNIT_ELEMENT(#8961,1.);
#8944=DERIVED_UNIT_ELEMENT(#47719,-3.);
#8945=DERIVED_UNIT_ELEMENT(#8961,1.);
#8946=DERIVED_UNIT_ELEMENT(#47719,-3.);
#8947=DERIVED_UNIT_ELEMENT(#8961,1.);
#8948=DERIVED_UNIT_ELEMENT(#47719,-3.);
#8949=DERIVED_UNIT_ELEMENT(#8961,1.);
#8950=DERIVED_UNIT_ELEMENT(#47719,-3.);
#8951=DERIVED_UNIT_ELEMENT(#8961,1.);
#8952=DERIVED_UNIT_ELEMENT(#47719,-3.);
#8953=DERIVED_UNIT_ELEMENT(#8961,1.);
#8954=DERIVED_UNIT_ELEMENT(#47719,-3.);
#8955=DERIVED_UNIT_ELEMENT(#8961,1.);
#8956=DERIVED_UNIT_ELEMENT(#47719,-3.);
#8957=DERIVED_UNIT_ELEMENT(#8961,1.);
#8958=DERIVED_UNIT_ELEMENT(#47719,-3.);
#8959=DERIVED_UNIT_ELEMENT(#8961,1.);
#8960=DERIVED_UNIT_ELEMENT(#47719,-3.);
#8961=(
MASS_UNIT()
NAMED_UNIT(*)
SI_UNIT(.KILO.,.GRAM.)
);
#8962=DERIVED_UNIT((#8937,#8938));
#8963=DERIVED_UNIT((#8939,#8940));
#8964=DERIVED_UNIT((#8941,#8942));
#8965=DERIVED_UNIT((#8943,#8944));
#8966=DERIVED_UNIT((#8945,#8946));
#8967=DERIVED_UNIT((#8947,#8948));
#8968=DERIVED_UNIT((#8949,#8950));
#8969=DERIVED_UNIT((#8951,#8952));
#8970=DERIVED_UNIT((#8953,#8954));
#8971=DERIVED_UNIT((#8955,#8956));
#8972=DERIVED_UNIT((#8957,#8958));
#8973=DERIVED_UNIT((#8959,#8960));
#8974=MEASURE_REPRESENTATION_ITEM('density measure',
POSITIVE_RATIO_MEASURE(7850.),#8962);
#8975=MEASURE_REPRESENTATION_ITEM('density measure',
POSITIVE_RATIO_MEASURE(7850.),#8963);
#8976=MEASURE_REPRESENTATION_ITEM('density measure',
POSITIVE_RATIO_MEASURE(7850.),#8964);
#8977=MEASURE_REPRESENTATION_ITEM('density measure',
POSITIVE_RATIO_MEASURE(7850.),#8965);
#8978=MEASURE_REPRESENTATION_ITEM('density measure',
POSITIVE_RATIO_MEASURE(7850.),#8966);
#8979=MEASURE_REPRESENTATION_ITEM('density measure',
POSITIVE_RATIO_MEASURE(7850.),#8967);
#8980=MEASURE_REPRESENTATION_ITEM('density measure',
POSITIVE_RATIO_MEASURE(7850.),#8968);
#8981=MEASURE_REPRESENTATION_ITEM('density measure',
POSITIVE_RATIO_MEASURE(7850.),#8969);
#8982=MEASURE_REPRESENTATION_ITEM('density measure',
POSITIVE_RATIO_MEASURE(7850.),#8970);
#8983=MEASURE_REPRESENTATION_ITEM('density measure',
POSITIVE_RATIO_MEASURE(7850.),#8971);
#8984=MEASURE_REPRESENTATION_ITEM('density measure',
POSITIVE_RATIO_MEASURE(7850.),#8972);
#8985=MEASURE_REPRESENTATION_ITEM('density measure',
POSITIVE_RATIO_MEASURE(7850.),#8973);
#8986=PROPERTY_DEFINITION_REPRESENTATION(#9046,#9010);
#8987=PROPERTY_DEFINITION_REPRESENTATION(#9047,#9011);
#8988=PROPERTY_DEFINITION_REPRESENTATION(#9048,#9012);
#8989=PROPERTY_DEFINITION_REPRESENTATION(#9049,#9013);
#8990=PROPERTY_DEFINITION_REPRESENTATION(#9050,#9014);
#8991=PROPERTY_DEFINITION_REPRESENTATION(#9051,#9015);
#8992=PROPERTY_DEFINITION_REPRESENTATION(#9052,#9016);
#8993=PROPERTY_DEFINITION_REPRESENTATION(#9053,#9017);
#8994=PROPERTY_DEFINITION_REPRESENTATION(#9054,#9018);
#8995=PROPERTY_DEFINITION_REPRESENTATION(#9055,#9019);
#8996=PROPERTY_DEFINITION_REPRESENTATION(#9056,#9020);
#8997=PROPERTY_DEFINITION_REPRESENTATION(#9057,#9021);
#8998=PROPERTY_DEFINITION_REPRESENTATION(#9058,#9022);
#8999=PROPERTY_DEFINITION_REPRESENTATION(#9059,#9023);
#9000=PROPERTY_DEFINITION_REPRESENTATION(#9060,#9024);
#9001=PROPERTY_DEFINITION_REPRESENTATION(#9061,#9025);
#9002=PROPERTY_DEFINITION_REPRESENTATION(#9062,#9026);
#9003=PROPERTY_DEFINITION_REPRESENTATION(#9063,#9027);
#9004=PROPERTY_DEFINITION_REPRESENTATION(#9064,#9028);
#9005=PROPERTY_DEFINITION_REPRESENTATION(#9065,#9029);
#9006=PROPERTY_DEFINITION_REPRESENTATION(#9066,#9030);
#9007=PROPERTY_DEFINITION_REPRESENTATION(#9067,#9031);
#9008=PROPERTY_DEFINITION_REPRESENTATION(#9068,#9032);
#9009=PROPERTY_DEFINITION_REPRESENTATION(#9069,#9033);
#9010=REPRESENTATION('material name',(#9034),#47705);
#9011=REPRESENTATION('density',(#8974),#47705);
#9012=REPRESENTATION('material name',(#9035),#47706);
#9013=REPRESENTATION('density',(#8975),#47706);
#9014=REPRESENTATION('material name',(#9036),#47707);
#9015=REPRESENTATION('density',(#8976),#47707);
#9016=REPRESENTATION('material name',(#9037),#47708);
#9017=REPRESENTATION('density',(#8977),#47708);
#9018=REPRESENTATION('material name',(#9038),#47709);
#9019=REPRESENTATION('density',(#8978),#47709);
#9020=REPRESENTATION('material name',(#9039),#47710);
#9021=REPRESENTATION('density',(#8979),#47710);
#9022=REPRESENTATION('material name',(#9040),#47711);
#9023=REPRESENTATION('density',(#8980),#47711);
#9024=REPRESENTATION('material name',(#9041),#47712);
#9025=REPRESENTATION('density',(#8981),#47712);
#9026=REPRESENTATION('material name',(#9042),#47713);
#9027=REPRESENTATION('density',(#8982),#47713);
#9028=REPRESENTATION('material name',(#9043),#47714);
#9029=REPRESENTATION('density',(#8983),#47714);
#9030=REPRESENTATION('material name',(#9044),#47715);
#9031=REPRESENTATION('density',(#8984),#47715);
#9032=REPRESENTATION('material name',(#9045),#47716);
#9033=REPRESENTATION('density',(#8985),#47716);
#9034=DESCRIPTIVE_REPRESENTATION_ITEM('Steel','Steel');
#9035=DESCRIPTIVE_REPRESENTATION_ITEM('Steel','Steel');
#9036=DESCRIPTIVE_REPRESENTATION_ITEM('Steel','Steel');
#9037=DESCRIPTIVE_REPRESENTATION_ITEM('Steel','Steel');
#9038=DESCRIPTIVE_REPRESENTATION_ITEM('Steel','Steel');
#9039=DESCRIPTIVE_REPRESENTATION_ITEM('Steel','Steel');
#9040=DESCRIPTIVE_REPRESENTATION_ITEM('Steel','Steel');
#9041=DESCRIPTIVE_REPRESENTATION_ITEM('Steel','Steel');
#9042=DESCRIPTIVE_REPRESENTATION_ITEM('Steel','Steel');
#9043=DESCRIPTIVE_REPRESENTATION_ITEM('Steel','Steel');
#9044=DESCRIPTIVE_REPRESENTATION_ITEM('Steel','Steel');
#9045=DESCRIPTIVE_REPRESENTATION_ITEM('Steel','Steel');
#9046=PROPERTY_DEFINITION('material property','material name',#47775);
#9047=PROPERTY_DEFINITION('material property','density of part',#47775);
#9048=PROPERTY_DEFINITION('material property','material name',#47776);
#9049=PROPERTY_DEFINITION('material property','density of part',#47776);
#9050=PROPERTY_DEFINITION('material property','material name',#47777);
#9051=PROPERTY_DEFINITION('material property','density of part',#47777);
#9052=PROPERTY_DEFINITION('material property','material name',#47778);
#9053=PROPERTY_DEFINITION('material property','density of part',#47778);
#9054=PROPERTY_DEFINITION('material property','material name',#47779);
#9055=PROPERTY_DEFINITION('material property','density of part',#47779);
#9056=PROPERTY_DEFINITION('material property','material name',#47780);
#9057=PROPERTY_DEFINITION('material property','density of part',#47780);
#9058=PROPERTY_DEFINITION('material property','material name',#47781);
#9059=PROPERTY_DEFINITION('material property','density of part',#47781);
#9060=PROPERTY_DEFINITION('material property','material name',#47782);
#9061=PROPERTY_DEFINITION('material property','density of part',#47782);
#9062=PROPERTY_DEFINITION('material property','material name',#47783);
#9063=PROPERTY_DEFINITION('material property','density of part',#47783);
#9064=PROPERTY_DEFINITION('material property','material name',#47784);
#9065=PROPERTY_DEFINITION('material property','density of part',#47784);
#9066=PROPERTY_DEFINITION('material property','material name',#47785);
#9067=PROPERTY_DEFINITION('material property','density of part',#47785);
#9068=PROPERTY_DEFINITION('material property','material name',#47786);
#9069=PROPERTY_DEFINITION('material property','density of part',#47786);
#9070=AXIS2_PLACEMENT_3D('',#12215,#9956,#9957);
#9071=AXIS2_PLACEMENT_3D('',#12216,#9958,#9959);
#9072=AXIS2_PLACEMENT_3D('',#12217,#9960,#9961);
#9073=AXIS2_PLACEMENT_3D('',#12219,#9962,#9963);
#9074=AXIS2_PLACEMENT_3D('',#12220,#9964,#9965);
#9075=AXIS2_PLACEMENT_3D('',#12222,#9966,#9967);
#9076=AXIS2_PLACEMENT_3D('',#12225,#9969,#9970);
#9077=AXIS2_PLACEMENT_3D('',#12226,#9971,#9972);
#9078=AXIS2_PLACEMENT_3D('',#12228,#9973,#9974);
#9079=AXIS2_PLACEMENT_3D('',#12229,#9975,#9976);
#9080=AXIS2_PLACEMENT_3D('',#12230,#9977,#9978);
#9081=AXIS2_PLACEMENT_3D('',#12231,#9979,#9980);
#9082=AXIS2_PLACEMENT_3D('',#12232,#9981,#9982);
#9083=AXIS2_PLACEMENT_3D('',#12235,#9983,#9984);
#9084=AXIS2_PLACEMENT_3D('',#12236,#9985,#9986);
#9085=AXIS2_PLACEMENT_3D('',#12238,#9987,#9988);
#9086=AXIS2_PLACEMENT_3D('',#12240,#9989,#9990);
#9087=AXIS2_PLACEMENT_3D('',#12241,#9991,#9992);
#9088=AXIS2_PLACEMENT_3D('',#12242,#9993,#9994);
#9089=AXIS2_PLACEMENT_3D('',#12244,#9995,#9996);
#9090=AXIS2_PLACEMENT_3D('',#12246,#9997,#9998);
#9091=AXIS2_PLACEMENT_3D('',#12248,#9999,#10000);
#9092=AXIS2_PLACEMENT_3D('',#12249,#10001,#10002);
#9093=AXIS2_PLACEMENT_3D('',#12250,#10003,#10004);
#9094=AXIS2_PLACEMENT_3D('',#12252,#10005,#10006);
#9095=AXIS2_PLACEMENT_3D('',#12253,#10007,#10008);
#9096=AXIS2_PLACEMENT_3D('',#12254,#10009,#10010);
#9097=AXIS2_PLACEMENT_3D('',#12256,#10011,#10012);
#9098=AXIS2_PLACEMENT_3D('',#12257,#10013,#10014);
#9099=AXIS2_PLACEMENT_3D('',#12258,#10015,#10016);
#9100=AXIS2_PLACEMENT_3D('',#12262,#10018,#10019);
#9101=AXIS2_PLACEMENT_3D('',#12264,#10020,#10021);
#9102=AXIS2_PLACEMENT_3D('',#12265,#10022,#10023);
#9103=AXIS2_PLACEMENT_3D('',#12436,#10024,#10025);
#9104=AXIS2_PLACEMENT_3D('',#13663,#10026,#10027);
#9105=AXIS2_PLACEMENT_3D('',#14142,#10028,#10029);
#9106=AXIS2_PLACEMENT_3D('',#14183,#10030,#10031);
#9107=AXIS2_PLACEMENT_3D('',#14185,#10033,#10034);
#9108=AXIS2_PLACEMENT_3D('',#14354,#10035,#10036);
#9109=AXIS2_PLACEMENT_3D('',#15531,#10037,#10038);
#9110=AXIS2_PLACEMENT_3D('',#15672,#10039,#10040);
#9111=AXIS2_PLACEMENT_3D('',#15673,#10041,#10042);
#9112=AXIS2_PLACEMENT_3D('',#15674,#10043,#10044);
#9113=AXIS2_PLACEMENT_3D('',#15675,#10045,#10046);
#9114=AXIS2_PLACEMENT_3D('',#15677,#10047,#10048);
#9115=AXIS2_PLACEMENT_3D('',#15678,#10049,#10050);
#9116=AXIS2_PLACEMENT_3D('',#15680,#10051,#10052);
#9117=AXIS2_PLACEMENT_3D('',#15683,#10054,#10055);
#9118=AXIS2_PLACEMENT_3D('',#15684,#10056,#10057);
#9119=AXIS2_PLACEMENT_3D('',#15686,#10058,#10059);
#9120=AXIS2_PLACEMENT_3D('',#15687,#10060,#10061);
#9121=AXIS2_PLACEMENT_3D('',#15688,#10062,#10063);
#9122=AXIS2_PLACEMENT_3D('',#15689,#10064,#10065);
#9123=AXIS2_PLACEMENT_3D('',#15690,#10066,#10067);
#9124=AXIS2_PLACEMENT_3D('',#15693,#10068,#10069);
#9125=AXIS2_PLACEMENT_3D('',#15697,#10071,#10072);
#9126=AXIS2_PLACEMENT_3D('',#15701,#10074,#10075);
#9127=AXIS2_PLACEMENT_3D('',#15705,#10077,#10078);
#9128=AXIS2_PLACEMENT_3D('',#15720,#10080,#10081);
#9129=AXIS2_PLACEMENT_3D('',#15723,#10082,#10083);
#9130=AXIS2_PLACEMENT_3D('',#15725,#10084,#10085);
#9131=AXIS2_PLACEMENT_3D('',#15727,#10086,#10087);
#9132=AXIS2_PLACEMENT_3D('',#15738,#10088,#10089);
#9133=AXIS2_PLACEMENT_3D('',#15741,#10090,#10091);
#9134=AXIS2_PLACEMENT_3D('',#15743,#10092,#10093);
#9135=AXIS2_PLACEMENT_3D('',#15745,#10094,#10095);
#9136=AXIS2_PLACEMENT_3D('',#15756,#10096,#10097);
#9137=AXIS2_PLACEMENT_3D('',#15759,#10098,#10099);
#9138=AXIS2_PLACEMENT_3D('',#15793,#10100,#10101);
#9139=AXIS2_PLACEMENT_3D('',#15794,#10102,#10103);
#9140=AXIS2_PLACEMENT_3D('',#15795,#10104,#10105);
#9141=AXIS2_PLACEMENT_3D('',#15798,#10106,#10107);
#9142=AXIS2_PLACEMENT_3D('',#15832,#10108,#10109);
#9143=AXIS2_PLACEMENT_3D('',#15833,#10110,#10111);
#9144=AXIS2_PLACEMENT_3D('',#15834,#10112,#10113);
#9145=AXIS2_PLACEMENT_3D('',#15837,#10114,#10115);
#9146=AXIS2_PLACEMENT_3D('',#15846,#10116,#10117);
#9147=AXIS2_PLACEMENT_3D('',#15849,#10118,#10119);
#9148=AXIS2_PLACEMENT_3D('',#15858,#10120,#10121);
#9149=AXIS2_PLACEMENT_3D('',#15860,#10122,#10123);
#9150=AXIS2_PLACEMENT_3D('',#15863,#10125,#10126);
#9151=AXIS2_PLACEMENT_3D('',#15864,#10127,#10128);
#9152=AXIS2_PLACEMENT_3D('',#15866,#10129,#10130);
#9153=AXIS2_PLACEMENT_3D('',#15869,#10132,#10133);
#9154=AXIS2_PLACEMENT_3D('',#15870,#10134,#10135);
#9155=AXIS2_PLACEMENT_3D('',#15872,#10136,#10137);
#9156=AXIS2_PLACEMENT_3D('',#15885,#10139,#10140);
#9157=AXIS2_PLACEMENT_3D('',#15887,#10142,#10143);
#9158=AXIS2_PLACEMENT_3D('',#15890,#10144,#10145);
#9159=AXIS2_PLACEMENT_3D('',#15904,#10147,#10148);
#9160=AXIS2_PLACEMENT_3D('',#15906,#10150,#10151);
#9161=AXIS2_PLACEMENT_3D('',#15939,#10154,#10155);
#9162=AXIS2_PLACEMENT_3D('',#16176,#10158,#10159);
#9163=AXIS2_PLACEMENT_3D('',#16211,#10162,#10163);
#9164=AXIS2_PLACEMENT_3D('',#16278,#10166,#10167);
#9165=AXIS2_PLACEMENT_3D('',#16333,#10169,#10170);
#9166=AXIS2_PLACEMENT_3D('',#16335,#10172,#10173);
#9167=AXIS2_PLACEMENT_3D('',#16362,#10176,#10177);
#9168=AXIS2_PLACEMENT_3D('',#16389,#10180,#10181);
#9169=AXIS2_PLACEMENT_3D('',#16416,#10184,#10185);
#9170=AXIS2_PLACEMENT_3D('',#16443,#10188,#10189);
#9171=AXIS2_PLACEMENT_3D('',#16470,#10192,#10193);
#9172=AXIS2_PLACEMENT_3D('',#16497,#10196,#10197);
#9173=AXIS2_PLACEMENT_3D('',#17079,#10200,#10201);
#9174=AXIS2_PLACEMENT_3D('',#17080,#10202,#10203);
#9175=AXIS2_PLACEMENT_3D('',#17093,#10206,#10207);
#9176=AXIS2_PLACEMENT_3D('',#17111,#10209,#10210);
#9177=AXIS2_PLACEMENT_3D('',#17129,#10212,#10213);
#9178=AXIS2_PLACEMENT_3D('',#17147,#10215,#10216);
#9179=AXIS2_PLACEMENT_3D('',#17165,#10218,#10219);
#9180=AXIS2_PLACEMENT_3D('',#17183,#10221,#10222);
#9181=AXIS2_PLACEMENT_3D('',#17212,#10226,#10227);
#9182=AXIS2_PLACEMENT_3D('',#17215,#10229,#10230);
#9183=AXIS2_PLACEMENT_3D('',#17289,#10233,#10234);
#9184=AXIS2_PLACEMENT_3D('',#17290,#10235,#10236);
#9185=AXIS2_PLACEMENT_3D('',#17839,#10243,#10244);
#9186=AXIS2_PLACEMENT_3D('',#17850,#10245,#10246);
#9187=AXIS2_PLACEMENT_3D('',#17861,#10247,#10248);
#9188=AXIS2_PLACEMENT_3D('',#17872,#10249,#10250);
#9189=AXIS2_PLACEMENT_3D('',#17883,#10251,#10252);
#9190=AXIS2_PLACEMENT_3D('',#17894,#10253,#10254);
#9191=AXIS2_PLACEMENT_3D('',#17905,#10255,#10256);
#9192=AXIS2_PLACEMENT_3D('',#17912,#10257,#10258);
#9193=AXIS2_PLACEMENT_3D('',#17913,#10259,#10260);
#9194=AXIS2_PLACEMENT_3D('',#18334,#10262,#10263);
#9195=AXIS2_PLACEMENT_3D('',#18338,#10265,#10266);
#9196=AXIS2_PLACEMENT_3D('',#18340,#10267,#10268);
#9197=AXIS2_PLACEMENT_3D('',#18341,#10269,#10270);
#9198=AXIS2_PLACEMENT_3D('',#18343,#10272,#10273);
#9199=AXIS2_PLACEMENT_3D('',#18378,#10275,#10276);
#9200=AXIS2_PLACEMENT_3D('',#18382,#10279,#10280);
#9201=AXIS2_PLACEMENT_3D('',#18424,#10283,#10284);
#9202=AXIS2_PLACEMENT_3D('',#18430,#10288,#10289);
#9203=AXIS2_PLACEMENT_3D('',#18439,#10294,#10295);
#9204=AXIS2_PLACEMENT_3D('',#18463,#10297,#10298);
#9205=AXIS2_PLACEMENT_3D('',#18467,#10300,#10301);
#9206=AXIS2_PLACEMENT_3D('',#18471,#10303,#10304);
#9207=AXIS2_PLACEMENT_3D('',#18475,#10306,#10307);
#9208=AXIS2_PLACEMENT_3D('',#18478,#10309,#10310);
#9209=AXIS2_PLACEMENT_3D('',#18500,#10311,#10312);
#9210=AXIS2_PLACEMENT_3D('',#18503,#10314,#10315);
#9211=AXIS2_PLACEMENT_3D('',#18504,#10316,#10317);
#9212=AXIS2_PLACEMENT_3D('',#18509,#10319,#10320);
#9213=AXIS2_PLACEMENT_3D('',#18512,#10322,#10323);
#9214=AXIS2_PLACEMENT_3D('',#18578,#10325,#10326);
#9215=AXIS2_PLACEMENT_3D('',#18581,#10329,#10330);
#9216=AXIS2_PLACEMENT_3D('',#18584,#10333,#10334);
#9217=AXIS2_PLACEMENT_3D('',#18674,#10336,#10337);
#9218=AXIS2_PLACEMENT_3D('',#18678,#10339,#10340);
#9219=AXIS2_PLACEMENT_3D('',#18680,#10342,#10343);
#9220=AXIS2_PLACEMENT_3D('',#18684,#10345,#10346);
#9221=AXIS2_PLACEMENT_3D('',#18688,#10348,#10349);
#9222=AXIS2_PLACEMENT_3D('',#18773,#10351,#10352);
#9223=AXIS2_PLACEMENT_3D('',#18774,#10353,#10354);
#9224=AXIS2_PLACEMENT_3D('',#18775,#10355,#10356);
#9225=AXIS2_PLACEMENT_3D('',#19156,#10358,#10359);
#9226=AXIS2_PLACEMENT_3D('',#19158,#10360,#10361);
#9227=AXIS2_PLACEMENT_3D('',#19159,#10362,#10363);
#9228=AXIS2_PLACEMENT_3D('',#19160,#10364,#10365);
#9229=AXIS2_PLACEMENT_3D('',#19164,#10368,#10369);
#9230=AXIS2_PLACEMENT_3D('',#19179,#10370,#10371);
#9231=AXIS2_PLACEMENT_3D('',#19194,#10372,#10373);
#9232=AXIS2_PLACEMENT_3D('',#19209,#10374,#10375);
#9233=AXIS2_PLACEMENT_3D('',#19224,#10376,#10377);
#9234=AXIS2_PLACEMENT_3D('',#19239,#10378,#10379);
#9235=AXIS2_PLACEMENT_3D('',#19254,#10380,#10381);
#9236=AXIS2_PLACEMENT_3D('',#19303,#10384,#10385);
#9237=AXIS2_PLACEMENT_3D('',#19332,#10386,#10387);
#9238=AXIS2_PLACEMENT_3D('',#19333,#10388,#10389);
#9239=AXIS2_PLACEMENT_3D('',#19335,#10390,#10391);
#9240=AXIS2_PLACEMENT_3D('',#19337,#10392,#10393);
#9241=AXIS2_PLACEMENT_3D('',#19338,#10394,#10395);
#9242=AXIS2_PLACEMENT_3D('',#19340,#10397,#10398);
#9243=AXIS2_PLACEMENT_3D('',#19444,#10400,#10401);
#9244=AXIS2_PLACEMENT_3D('',#19464,#10405,#10406);
#9245=AXIS2_PLACEMENT_3D('',#19470,#10410,#10411);
#9246=AXIS2_PLACEMENT_3D('',#19473,#10412,#10413);
#9247=AXIS2_PLACEMENT_3D('',#19527,#10414,#10415);
#9248=AXIS2_PLACEMENT_3D('',#19531,#10417,#10418);
#9249=AXIS2_PLACEMENT_3D('',#19588,#10419,#10420);
#9250=AXIS2_PLACEMENT_3D('',#19590,#10422,#10423);
#9251=AXIS2_PLACEMENT_3D('',#19608,#10425,#10426);
#9252=AXIS2_PLACEMENT_3D('',#19652,#10446,#10447);
#9253=AXIS2_PLACEMENT_3D('',#19656,#10450,#10451);
#9254=AXIS2_PLACEMENT_3D('',#19662,#10455,#10456);
#9255=AXIS2_PLACEMENT_3D('',#19721,#10476,#10477);
#9256=AXIS2_PLACEMENT_3D('',#19722,#10478,#10479);
#9257=AXIS2_PLACEMENT_3D('',#19734,#10480,#10481);
#9258=AXIS2_PLACEMENT_3D('',#19735,#10482,#10483);
#9259=AXIS2_PLACEMENT_3D('',#19737,#10484,#10485);
#9260=AXIS2_PLACEMENT_3D('',#19748,#10486,#10487);
#9261=AXIS2_PLACEMENT_3D('',#19750,#10489,#10490);
#9262=AXIS2_PLACEMENT_3D('',#19752,#10492,#10493);
#9263=AXIS2_PLACEMENT_3D('',#19754,#10495,#10496);
#9264=AXIS2_PLACEMENT_3D('',#19756,#10498,#10499);
#9265=AXIS2_PLACEMENT_3D('',#19758,#10501,#10502);
#9266=AXIS2_PLACEMENT_3D('',#19760,#10504,#10505);
#9267=AXIS2_PLACEMENT_3D('',#19762,#10507,#10508);
#9268=AXIS2_PLACEMENT_3D('',#19764,#10510,#10511);
#9269=AXIS2_PLACEMENT_3D('',#19766,#10513,#10514);
#9270=AXIS2_PLACEMENT_3D('',#19768,#10516,#10517);
#9271=AXIS2_PLACEMENT_3D('',#19770,#10519,#10520);
#9272=AXIS2_PLACEMENT_3D('',#19772,#10522,#10523);
#9273=AXIS2_PLACEMENT_3D('',#19774,#10525,#10526);
#9274=AXIS2_PLACEMENT_3D('',#19776,#10528,#10529);
#9275=AXIS2_PLACEMENT_3D('',#19778,#10531,#10532);
#9276=AXIS2_PLACEMENT_3D('',#19780,#10534,#10535);
#9277=AXIS2_PLACEMENT_3D('',#19782,#10537,#10538);
#9278=AXIS2_PLACEMENT_3D('',#19784,#10540,#10541);
#9279=AXIS2_PLACEMENT_3D('',#19785,#10542,#10543);
#9280=AXIS2_PLACEMENT_3D('',#19787,#10544,#10545);
#9281=AXIS2_PLACEMENT_3D('',#19788,#10546,#10547);
#9282=AXIS2_PLACEMENT_3D('',#19789,#10548,#10549);
#9283=AXIS2_PLACEMENT_3D('',#19821,#10550,#10551);
#9284=AXIS2_PLACEMENT_3D('',#19823,#10552,#10553);
#9285=AXIS2_PLACEMENT_3D('',#19824,#10554,#10555);
#9286=AXIS2_PLACEMENT_3D('',#19825,#10556,#10557);
#9287=AXIS2_PLACEMENT_3D('',#19869,#10558,#10559);
#9288=AXIS2_PLACEMENT_3D('',#19894,#10560,#10561);
#9289=AXIS2_PLACEMENT_3D('',#19925,#10562,#10563);
#9290=AXIS2_PLACEMENT_3D('',#19950,#10564,#10565);
#9291=AXIS2_PLACEMENT_3D('',#19969,#10566,#10567);
#9292=AXIS2_PLACEMENT_3D('',#19970,#10568,#10569);
#9293=AXIS2_PLACEMENT_3D('',#19972,#10570,#10571);
#9294=AXIS2_PLACEMENT_3D('',#19978,#10572,#10573);
#9295=AXIS2_PLACEMENT_3D('',#19985,#10574,#10575);
#9296=AXIS2_PLACEMENT_3D('',#19986,#10576,#10577);
#9297=AXIS2_PLACEMENT_3D('',#19987,#10578,#10579);
#9298=AXIS2_PLACEMENT_3D('',#19988,#10580,#10581);
#9299=AXIS2_PLACEMENT_3D('',#19989,#10582,#10583);
#9300=AXIS2_PLACEMENT_3D('',#19990,#10584,#10585);
#9301=AXIS2_PLACEMENT_3D('',#19991,#10586,#10587);
#9302=AXIS2_PLACEMENT_3D('',#19992,#10588,#10589);
#9303=AXIS2_PLACEMENT_3D('',#19993,#10590,#10591);
#9304=AXIS2_PLACEMENT_3D('',#19994,#10592,#10593);
#9305=AXIS2_PLACEMENT_3D('',#19995,#10594,#10595);
#9306=AXIS2_PLACEMENT_3D('',#19996,#10596,#10597);
#9307=AXIS2_PLACEMENT_3D('',#19997,#10598,#10599);
#9308=AXIS2_PLACEMENT_3D('',#19998,#10600,#10601);
#9309=AXIS2_PLACEMENT_3D('',#19999,#10602,#10603);
#9310=AXIS2_PLACEMENT_3D('',#20000,#10604,#10605);
#9311=AXIS2_PLACEMENT_3D('',#20001,#10606,#10607);
#9312=AXIS2_PLACEMENT_3D('',#20002,#10608,#10609);
#9313=AXIS2_PLACEMENT_3D('',#20051,#10610,#10611);
#9314=AXIS2_PLACEMENT_3D('',#20052,#10612,#10613);
#9315=AXIS2_PLACEMENT_3D('',#20053,#10614,#10615);
#9316=AXIS2_PLACEMENT_3D('',#20108,#10616,#10617);
#9317=AXIS2_PLACEMENT_3D('',#20109,#10618,#10619);
#9318=AXIS2_PLACEMENT_3D('',#20110,#10620,#10621);
#9319=AXIS2_PLACEMENT_3D('',#20111,#10622,#10623);
#9320=AXIS2_PLACEMENT_3D('',#20112,#10624,#10625);
#9321=AXIS2_PLACEMENT_3D('',#20113,#10626,#10627);
#9322=AXIS2_PLACEMENT_3D('',#20114,#10628,#10629);
#9323=AXIS2_PLACEMENT_3D('',#20115,#10630,#10631);
#9324=AXIS2_PLACEMENT_3D('',#20116,#10632,#10633);
#9325=AXIS2_PLACEMENT_3D('',#20117,#10634,#10635);
#9326=AXIS2_PLACEMENT_3D('',#22074,#10636,#10637);
#9327=AXIS2_PLACEMENT_3D('',#22075,#10638,#10639);
#9328=AXIS2_PLACEMENT_3D('',#32265,#10640,#10641);
#9329=AXIS2_PLACEMENT_3D('',#32266,#10642,#10643);
#9330=AXIS2_PLACEMENT_3D('',#32267,#10644,#10645);
#9331=AXIS2_PLACEMENT_3D('',#32280,#10646,#10647);
#9332=AXIS2_PLACEMENT_3D('',#32299,#10648,#10649);
#9333=AXIS2_PLACEMENT_3D('',#32300,#10650,#10651);
#9334=AXIS2_PLACEMENT_3D('',#32301,#10652,#10653);
#9335=AXIS2_PLACEMENT_3D('',#32302,#10654,#10655);
#9336=AXIS2_PLACEMENT_3D('',#32303,#10656,#10657);
#9337=AXIS2_PLACEMENT_3D('',#32304,#10658,#10659);
#9338=AXIS2_PLACEMENT_3D('',#32305,#10660,#10661);
#9339=AXIS2_PLACEMENT_3D('',#32306,#10662,#10663);
#9340=AXIS2_PLACEMENT_3D('',#32307,#10664,#10665);
#9341=AXIS2_PLACEMENT_3D('',#32308,#10666,#10667);
#9342=AXIS2_PLACEMENT_3D('',#32309,#10668,#10669);
#9343=AXIS2_PLACEMENT_3D('',#32310,#10670,#10671);
#9344=AXIS2_PLACEMENT_3D('',#32329,#10672,#10673);
#9345=AXIS2_PLACEMENT_3D('',#32342,#10674,#10675);
#9346=AXIS2_PLACEMENT_3D('',#32343,#10676,#10677);
#9347=AXIS2_PLACEMENT_3D('',#32358,#10679,#10680);
#9348=AXIS2_PLACEMENT_3D('',#32359,#10681,#10682);
#9349=AXIS2_PLACEMENT_3D('',#32400,#10684,#10685);
#9350=AXIS2_PLACEMENT_3D('',#32433,#10686,#10687);
#9351=AXIS2_PLACEMENT_3D('',#32509,#10689,#10690);
#9352=AXIS2_PLACEMENT_3D('',#32585,#10692,#10693);
#9353=AXIS2_PLACEMENT_3D('',#32661,#10695,#10696);
#9354=AXIS2_PLACEMENT_3D('',#32737,#10698,#10699);
#9355=AXIS2_PLACEMENT_3D('',#32813,#10701,#10702);
#9356=AXIS2_PLACEMENT_3D('',#32889,#10704,#10705);
#9357=AXIS2_PLACEMENT_3D('',#32965,#10707,#10708);
#9358=AXIS2_PLACEMENT_3D('',#33041,#10710,#10711);
#9359=AXIS2_PLACEMENT_3D('',#33117,#10713,#10714);
#9360=AXIS2_PLACEMENT_3D('',#33193,#10716,#10717);
#9361=AXIS2_PLACEMENT_3D('',#33269,#10719,#10720);
#9362=AXIS2_PLACEMENT_3D('',#33345,#10722,#10723);
#9363=AXIS2_PLACEMENT_3D('',#33421,#10725,#10726);
#9364=AXIS2_PLACEMENT_3D('',#33497,#10728,#10729);
#9365=AXIS2_PLACEMENT_3D('',#33573,#10731,#10732);
#9366=AXIS2_PLACEMENT_3D('',#33649,#10734,#10735);
#9367=AXIS2_PLACEMENT_3D('',#33725,#10737,#10738);
#9368=AXIS2_PLACEMENT_3D('',#33801,#10740,#10741);
#9369=AXIS2_PLACEMENT_3D('',#33877,#10743,#10744);
#9370=AXIS2_PLACEMENT_3D('',#33953,#10746,#10747);
#9371=AXIS2_PLACEMENT_3D('',#34029,#10749,#10750);
#9372=AXIS2_PLACEMENT_3D('',#34105,#10752,#10753);
#9373=AXIS2_PLACEMENT_3D('',#34181,#10755,#10756);
#9374=AXIS2_PLACEMENT_3D('',#34257,#10758,#10759);
#9375=AXIS2_PLACEMENT_3D('',#34333,#10761,#10762);
#9376=AXIS2_PLACEMENT_3D('',#34409,#10764,#10765);
#9377=AXIS2_PLACEMENT_3D('',#34485,#10767,#10768);
#9378=AXIS2_PLACEMENT_3D('',#34561,#10770,#10771);
#9379=AXIS2_PLACEMENT_3D('',#34637,#10773,#10774);
#9380=AXIS2_PLACEMENT_3D('',#34713,#10776,#10777);
#9381=AXIS2_PLACEMENT_3D('',#34789,#10779,#10780);
#9382=AXIS2_PLACEMENT_3D('',#34865,#10782,#10783);
#9383=AXIS2_PLACEMENT_3D('',#34941,#10785,#10786);
#9384=AXIS2_PLACEMENT_3D('',#35017,#10788,#10789);
#9385=AXIS2_PLACEMENT_3D('',#35093,#10791,#10792);
#9386=AXIS2_PLACEMENT_3D('',#35169,#10794,#10795);
#9387=AXIS2_PLACEMENT_3D('',#35245,#10797,#10798);
#9388=AXIS2_PLACEMENT_3D('',#35321,#10800,#10801);
#9389=AXIS2_PLACEMENT_3D('',#35326,#10803,#10804);
#9390=AXIS2_PLACEMENT_3D('',#35395,#10805,#10806);
#9391=AXIS2_PLACEMENT_3D('',#35397,#10807,#10808);
#9392=AXIS2_PLACEMENT_3D('',#35400,#10810,#10811);
#9393=AXIS2_PLACEMENT_3D('',#35401,#10812,#10813);
#9394=AXIS2_PLACEMENT_3D('',#35402,#10814,#10815);
#9395=AXIS2_PLACEMENT_3D('',#35473,#10818,#10819);
#9396=AXIS2_PLACEMENT_3D('',#35544,#10822,#10823);
#9397=AXIS2_PLACEMENT_3D('',#35615,#10826,#10827);
#9398=AXIS2_PLACEMENT_3D('',#35686,#10830,#10831);
#9399=AXIS2_PLACEMENT_3D('',#35757,#10834,#10835);
#9400=AXIS2_PLACEMENT_3D('',#35828,#10838,#10839);
#9401=AXIS2_PLACEMENT_3D('',#35899,#10842,#10843);
#9402=AXIS2_PLACEMENT_3D('',#35970,#10846,#10847);
#9403=AXIS2_PLACEMENT_3D('',#36041,#10850,#10851);
#9404=AXIS2_PLACEMENT_3D('',#36112,#10854,#10855);
#9405=AXIS2_PLACEMENT_3D('',#36114,#10856,#10857);
#9406=AXIS2_PLACEMENT_3D('',#36116,#10858,#10859);
#9407=AXIS2_PLACEMENT_3D('',#36118,#10860,#10861);
#9408=AXIS2_PLACEMENT_3D('',#36153,#10862,#10863);
#9409=AXIS2_PLACEMENT_3D('',#36188,#10864,#10865);
#9410=AXIS2_PLACEMENT_3D('',#36223,#10866,#10867);
#9411=AXIS2_PLACEMENT_3D('',#36258,#10868,#10869);
#9412=AXIS2_PLACEMENT_3D('',#36293,#10870,#10871);
#9413=AXIS2_PLACEMENT_3D('',#36328,#10872,#10873);
#9414=AXIS2_PLACEMENT_3D('',#36363,#10874,#10875);
#9415=AXIS2_PLACEMENT_3D('',#36397,#10876,#10877);
#9416=AXIS2_PLACEMENT_3D('',#36398,#10878,#10879);
#9417=AXIS2_PLACEMENT_3D('',#36399,#10880,#10881);
#9418=AXIS2_PLACEMENT_3D('',#36400,#10882,#10883);
#9419=AXIS2_PLACEMENT_3D('',#36401,#10884,#10885);
#9420=AXIS2_PLACEMENT_3D('',#36402,#10886,#10887);
#9421=AXIS2_PLACEMENT_3D('',#36403,#10888,#10889);
#9422=AXIS2_PLACEMENT_3D('',#36404,#10890,#10891);
#9423=AXIS2_PLACEMENT_3D('',#36405,#10892,#10893);
#9424=AXIS2_PLACEMENT_3D('',#36406,#10894,#10895);
#9425=AXIS2_PLACEMENT_3D('',#36408,#10896,#10897);
#9426=AXIS2_PLACEMENT_3D('',#36443,#10898,#10899);
#9427=AXIS2_PLACEMENT_3D('',#36478,#10900,#10901);
#9428=AXIS2_PLACEMENT_3D('',#36513,#10902,#10903);
#9429=AXIS2_PLACEMENT_3D('',#36548,#10904,#10905);
#9430=AXIS2_PLACEMENT_3D('',#36583,#10906,#10907);
#9431=AXIS2_PLACEMENT_3D('',#36618,#10908,#10909);
#9432=AXIS2_PLACEMENT_3D('',#36653,#10910,#10911);
#9433=AXIS2_PLACEMENT_3D('',#36687,#10912,#10913);
#9434=AXIS2_PLACEMENT_3D('',#36688,#10914,#10915);
#9435=AXIS2_PLACEMENT_3D('',#36690,#10916,#10917);
#9436=AXIS2_PLACEMENT_3D('',#36692,#10918,#10919);
#9437=AXIS2_PLACEMENT_3D('',#36693,#10920,#10921);
#9438=AXIS2_PLACEMENT_3D('',#36694,#10922,#10923);
#9439=AXIS2_PLACEMENT_3D('',#36695,#10924,#10925);
#9440=AXIS2_PLACEMENT_3D('',#36696,#10926,#10927);
#9441=AXIS2_PLACEMENT_3D('',#36697,#10928,#10929);
#9442=AXIS2_PLACEMENT_3D('',#36699,#10930,#10931);
#9443=AXIS2_PLACEMENT_3D('',#36734,#10932,#10933);
#9444=AXIS2_PLACEMENT_3D('',#36769,#10934,#10935);
#9445=AXIS2_PLACEMENT_3D('',#36804,#10936,#10937);
#9446=AXIS2_PLACEMENT_3D('',#36839,#10938,#10939);
#9447=AXIS2_PLACEMENT_3D('',#36874,#10940,#10941);
#9448=AXIS2_PLACEMENT_3D('',#36909,#10942,#10943);
#9449=AXIS2_PLACEMENT_3D('',#36944,#10944,#10945);
#9450=AXIS2_PLACEMENT_3D('',#36979,#10946,#10947);
#9451=AXIS2_PLACEMENT_3D('',#37014,#10948,#10949);
#9452=AXIS2_PLACEMENT_3D('',#37049,#10950,#10951);
#9453=AXIS2_PLACEMENT_3D('',#37084,#10952,#10953);
#9454=AXIS2_PLACEMENT_3D('',#37119,#10954,#10955);
#9455=AXIS2_PLACEMENT_3D('',#37154,#10956,#10957);
#9456=AXIS2_PLACEMENT_3D('',#37189,#10958,#10959);
#9457=AXIS2_PLACEMENT_3D('',#37224,#10960,#10961);
#9458=AXIS2_PLACEMENT_3D('',#37258,#10962,#10963);
#9459=AXIS2_PLACEMENT_3D('',#37259,#10964,#10965);
#9460=AXIS2_PLACEMENT_3D('',#37260,#10966,#10967);
#9461=AXIS2_PLACEMENT_3D('',#37261,#10968,#10969);
#9462=AXIS2_PLACEMENT_3D('',#37262,#10970,#10971);
#9463=AXIS2_PLACEMENT_3D('',#37263,#10972,#10973);
#9464=AXIS2_PLACEMENT_3D('',#37264,#10974,#10975);
#9465=AXIS2_PLACEMENT_3D('',#37275,#10976,#10977);
#9466=AXIS2_PLACEMENT_3D('',#37276,#10978,#10979);
#9467=AXIS2_PLACEMENT_3D('',#37278,#10981,#10982);
#9468=AXIS2_PLACEMENT_3D('',#37279,#10983,#10984);
#9469=AXIS2_PLACEMENT_3D('',#37280,#10985,#10986);
#9470=AXIS2_PLACEMENT_3D('',#37281,#10987,#10988);
#9471=AXIS2_PLACEMENT_3D('',#37282,#10989,#10990);
#9472=AXIS2_PLACEMENT_3D('',#37283,#10991,#10992);
#9473=AXIS2_PLACEMENT_3D('',#37284,#10993,#10994);
#9474=AXIS2_PLACEMENT_3D('',#37285,#10995,#10996);
#9475=AXIS2_PLACEMENT_3D('',#37286,#10997,#10998);
#9476=AXIS2_PLACEMENT_3D('',#37288,#11000,#11001);
#9477=AXIS2_PLACEMENT_3D('',#37291,#11004,#11005);
#9478=AXIS2_PLACEMENT_3D('',#37294,#11008,#11009);
#9479=AXIS2_PLACEMENT_3D('',#37297,#11012,#11013);
#9480=AXIS2_PLACEMENT_3D('',#37300,#11016,#11017);
#9481=AXIS2_PLACEMENT_3D('',#37303,#11020,#11021);
#9482=AXIS2_PLACEMENT_3D('',#37306,#11024,#11025);
#9483=AXIS2_PLACEMENT_3D('',#37309,#11028,#11029);
#9484=AXIS2_PLACEMENT_3D('',#37312,#11032,#11033);
#9485=AXIS2_PLACEMENT_3D('',#37315,#11036,#11037);
#9486=AXIS2_PLACEMENT_3D('',#37318,#11040,#11041);
#9487=AXIS2_PLACEMENT_3D('',#37321,#11044,#11045);
#9488=AXIS2_PLACEMENT_3D('',#37324,#11048,#11049);
#9489=AXIS2_PLACEMENT_3D('',#37327,#11052,#11053);
#9490=AXIS2_PLACEMENT_3D('',#37330,#11056,#11057);
#9491=AXIS2_PLACEMENT_3D('',#37367,#11058,#11059);
#9492=AXIS2_PLACEMENT_3D('',#37368,#11060,#11061);
#9493=AXIS2_PLACEMENT_3D('',#37371,#11064,#11065);
#9494=AXIS2_PLACEMENT_3D('',#44258,#11066,#11067);
#9495=AXIS2_PLACEMENT_3D('',#44259,#11068,#11069);
#9496=AXIS2_PLACEMENT_3D('',#44260,#11070,#11071);
#9497=AXIS2_PLACEMENT_3D('',#44261,#11072,#11073);
#9498=AXIS2_PLACEMENT_3D('',#44262,#11074,#11075);
#9499=AXIS2_PLACEMENT_3D('',#44263,#11076,#11077);
#9500=AXIS2_PLACEMENT_3D('',#44264,#11078,#11079);
#9501=AXIS2_PLACEMENT_3D('',#44265,#11080,#11081);
#9502=AXIS2_PLACEMENT_3D('',#44266,#11082,#11083);
#9503=AXIS2_PLACEMENT_3D('',#44267,#11084,#11085);
#9504=AXIS2_PLACEMENT_3D('',#44268,#11086,#11087);
#9505=AXIS2_PLACEMENT_3D('',#44269,#11088,#11089);
#9506=AXIS2_PLACEMENT_3D('',#44270,#11090,#11091);
#9507=AXIS2_PLACEMENT_3D('',#44271,#11092,#11093);
#9508=AXIS2_PLACEMENT_3D('',#44272,#11094,#11095);
#9509=AXIS2_PLACEMENT_3D('',#44273,#11096,#11097);
#9510=AXIS2_PLACEMENT_3D('',#44274,#11098,#11099);
#9511=AXIS2_PLACEMENT_3D('',#44275,#11100,#11101);
#9512=AXIS2_PLACEMENT_3D('',#44276,#11102,#11103);
#9513=AXIS2_PLACEMENT_3D('',#44316,#11104,#11105);
#9514=AXIS2_PLACEMENT_3D('',#44353,#11107,#11108);
#9515=AXIS2_PLACEMENT_3D('',#44354,#11109,#11110);
#9516=AXIS2_PLACEMENT_3D('',#44355,#11111,#11112);
#9517=AXIS2_PLACEMENT_3D('',#44358,#11113,#11114);
#9518=AXIS2_PLACEMENT_3D('',#44360,#11115,#11116);
#9519=AXIS2_PLACEMENT_3D('',#44362,#11117,#11118);
#9520=AXIS2_PLACEMENT_3D('',#44363,#11119,#11120);
#9521=AXIS2_PLACEMENT_3D('',#44364,#11121,#11122);
#9522=AXIS2_PLACEMENT_3D('',#44367,#11123,#11124);
#9523=AXIS2_PLACEMENT_3D('',#44369,#11125,#11126);
#9524=AXIS2_PLACEMENT_3D('',#44371,#11127,#11128);
#9525=AXIS2_PLACEMENT_3D('',#44372,#11129,#11130);
#9526=AXIS2_PLACEMENT_3D('',#44373,#11131,#11132);
#9527=AXIS2_PLACEMENT_3D('',#44375,#11133,#11134);
#9528=AXIS2_PLACEMENT_3D('',#44378,#11136,#11137);
#9529=AXIS2_PLACEMENT_3D('',#44379,#11138,#11139);
#9530=AXIS2_PLACEMENT_3D('',#44381,#11140,#11141);
#9531=AXIS2_PLACEMENT_3D('',#44384,#11143,#11144);
#9532=AXIS2_PLACEMENT_3D('',#44385,#11145,#11146);
#9533=AXIS2_PLACEMENT_3D('',#44387,#11147,#11148);
#9534=AXIS2_PLACEMENT_3D('',#44390,#11150,#11151);
#9535=AXIS2_PLACEMENT_3D('',#44391,#11152,#11153);
#9536=AXIS2_PLACEMENT_3D('',#44394,#11154,#11155);
#9537=AXIS2_PLACEMENT_3D('',#44396,#11156,#11157);
#9538=AXIS2_PLACEMENT_3D('',#44398,#11158,#11159);
#9539=AXIS2_PLACEMENT_3D('',#44442,#11160,#11161);
#9540=AXIS2_PLACEMENT_3D('',#44445,#11162,#11163);
#9541=AXIS2_PLACEMENT_3D('',#44447,#11164,#11165);
#9542=AXIS2_PLACEMENT_3D('',#44449,#11166,#11167);
#9543=AXIS2_PLACEMENT_3D('',#44458,#11168,#11169);
#9544=AXIS2_PLACEMENT_3D('',#44461,#11170,#11171);
#9545=AXIS2_PLACEMENT_3D('',#44465,#11173,#11174);
#9546=AXIS2_PLACEMENT_3D('',#44467,#11176,#11177);
#9547=AXIS2_PLACEMENT_3D('',#44470,#11180,#11181);
#9548=AXIS2_PLACEMENT_3D('',#44473,#11182,#11183);
#9549=AXIS2_PLACEMENT_3D('',#44477,#11185,#11186);
#9550=AXIS2_PLACEMENT_3D('',#44479,#11188,#11189);
#9551=AXIS2_PLACEMENT_3D('',#44482,#11190,#11191);
#9552=AXIS2_PLACEMENT_3D('',#44484,#11192,#11193);
#9553=AXIS2_PLACEMENT_3D('',#44527,#11194,#11195);
#9554=AXIS2_PLACEMENT_3D('',#44531,#11197,#11198);
#9555=AXIS2_PLACEMENT_3D('',#44571,#11199,#11200);
#9556=AXIS2_PLACEMENT_3D('',#44573,#11201,#11202);
#9557=AXIS2_PLACEMENT_3D('',#44575,#11204,#11205);
#9558=AXIS2_PLACEMENT_3D('',#44578,#11206,#11207);
#9559=AXIS2_PLACEMENT_3D('',#44582,#11209,#11210);
#9560=AXIS2_PLACEMENT_3D('',#44584,#11212,#11213);
#9561=AXIS2_PLACEMENT_3D('',#44589,#11215,#11216);
#9562=AXIS2_PLACEMENT_3D('',#44592,#11218,#11219);
#9563=AXIS2_PLACEMENT_3D('',#44593,#11220,#11221);
#9564=AXIS2_PLACEMENT_3D('',#44596,#11222,#11223);
#9565=AXIS2_PLACEMENT_3D('',#44598,#11224,#11225);
#9566=AXIS2_PLACEMENT_3D('',#44600,#11226,#11227);
#9567=AXIS2_PLACEMENT_3D('',#44601,#11228,#11229);
#9568=AXIS2_PLACEMENT_3D('',#44603,#11230,#11231);
#9569=AXIS2_PLACEMENT_3D('',#44604,#11232,#11233);
#9570=AXIS2_PLACEMENT_3D('',#44608,#11235,#11236);
#9571=AXIS2_PLACEMENT_3D('',#44610,#11237,#11238);
#9572=AXIS2_PLACEMENT_3D('',#44611,#11239,#11240);
#9573=AXIS2_PLACEMENT_3D('',#44612,#11241,#11242);
#9574=AXIS2_PLACEMENT_3D('',#44615,#11243,#11244);
#9575=AXIS2_PLACEMENT_3D('',#44617,#11245,#11246);
#9576=AXIS2_PLACEMENT_3D('',#44619,#11247,#11248);
#9577=AXIS2_PLACEMENT_3D('',#44621,#11249,#11250);
#9578=AXIS2_PLACEMENT_3D('',#44624,#11252,#11253);
#9579=AXIS2_PLACEMENT_3D('',#44625,#11254,#11255);
#9580=AXIS2_PLACEMENT_3D('',#44627,#11256,#11257);
#9581=AXIS2_PLACEMENT_3D('',#44629,#11258,#11259);
#9582=AXIS2_PLACEMENT_3D('',#44630,#11260,#11261);
#9583=AXIS2_PLACEMENT_3D('',#44631,#11262,#11263);
#9584=AXIS2_PLACEMENT_3D('',#44642,#11270,#11271);
#9585=AXIS2_PLACEMENT_3D('',#44644,#11272,#11273);
#9586=AXIS2_PLACEMENT_3D('',#44648,#11275,#11276);
#9587=AXIS2_PLACEMENT_3D('',#44652,#11278,#11279);
#9588=AXIS2_PLACEMENT_3D('',#44655,#11281,#11282);
#9589=AXIS2_PLACEMENT_3D('',#44656,#11283,#11284);
#9590=AXIS2_PLACEMENT_3D('',#44661,#11286,#11287);
#9591=AXIS2_PLACEMENT_3D('',#44664,#11289,#11290);
#9592=AXIS2_PLACEMENT_3D('',#44665,#11291,#11292);
#9593=AXIS2_PLACEMENT_3D('',#44666,#11293,#11294);
#9594=AXIS2_PLACEMENT_3D('',#44667,#11295,#11296);
#9595=AXIS2_PLACEMENT_3D('',#44668,#11297,#11298);
#9596=AXIS2_PLACEMENT_3D('',#44674,#11302,#11303);
#9597=AXIS2_PLACEMENT_3D('',#44676,#11304,#11305);
#9598=AXIS2_PLACEMENT_3D('',#44718,#11306,#11307);
#9599=AXIS2_PLACEMENT_3D('',#44722,#11309,#11310);
#9600=AXIS2_PLACEMENT_3D('',#44760,#11311,#11312);
#9601=AXIS2_PLACEMENT_3D('',#44761,#11313,#11314);
#9602=AXIS2_PLACEMENT_3D('',#44762,#11315,#11316);
#9603=AXIS2_PLACEMENT_3D('',#44763,#11317,#11318);
#9604=AXIS2_PLACEMENT_3D('',#44764,#11319,#11320);
#9605=AXIS2_PLACEMENT_3D('',#44779,#11321,#11322);
#9606=AXIS2_PLACEMENT_3D('',#44781,#11323,#11324);
#9607=AXIS2_PLACEMENT_3D('',#44783,#11325,#11326);
#9608=AXIS2_PLACEMENT_3D('',#44825,#11346,#11347);
#9609=AXIS2_PLACEMENT_3D('',#44828,#11349,#11350);
#9610=AXIS2_PLACEMENT_3D('',#44830,#11352,#11353);
#9611=AXIS2_PLACEMENT_3D('',#44835,#11354,#11355);
#9612=AXIS2_PLACEMENT_3D('',#44842,#11356,#11357);
#9613=AXIS2_PLACEMENT_3D('',#44844,#11358,#11359);
#9614=AXIS2_PLACEMENT_3D('',#44845,#11360,#11361);
#9615=AXIS2_PLACEMENT_3D('',#44846,#11362,#11363);
#9616=AXIS2_PLACEMENT_3D('',#44849,#11364,#11365);
#9617=AXIS2_PLACEMENT_3D('',#44851,#11366,#11367);
#9618=AXIS2_PLACEMENT_3D('',#44853,#11368,#11369);
#9619=AXIS2_PLACEMENT_3D('',#44855,#11371,#11372);
#9620=AXIS2_PLACEMENT_3D('',#44864,#11374,#11375);
#9621=AXIS2_PLACEMENT_3D('',#44867,#11376,#11377);
#9622=AXIS2_PLACEMENT_3D('',#44873,#11379,#11380);
#9623=AXIS2_PLACEMENT_3D('',#44874,#11381,#11382);
#9624=AXIS2_PLACEMENT_3D('',#44875,#11383,#11384);
#9625=AXIS2_PLACEMENT_3D('',#44876,#11385,#11386);
#9626=AXIS2_PLACEMENT_3D('',#44928,#11405,#11406);
#9627=AXIS2_PLACEMENT_3D('',#44963,#11407,#11408);
#9628=AXIS2_PLACEMENT_3D('',#44964,#11409,#11410);
#9629=AXIS2_PLACEMENT_3D('',#44965,#11411,#11412);
#9630=AXIS2_PLACEMENT_3D('',#45003,#11413,#11414);
#9631=AXIS2_PLACEMENT_3D('',#45004,#11415,#11416);
#9632=AXIS2_PLACEMENT_3D('',#45005,#11417,#11418);
#9633=AXIS2_PLACEMENT_3D('',#45006,#11419,#11420);
#9634=AXIS2_PLACEMENT_3D('',#45007,#11421,#11422);
#9635=AXIS2_PLACEMENT_3D('',#45008,#11423,#11424);
#9636=AXIS2_PLACEMENT_3D('',#45014,#11428,#11429);
#9637=AXIS2_PLACEMENT_3D('',#45017,#11431,#11432);
#9638=AXIS2_PLACEMENT_3D('',#45018,#11433,#11434);
#9639=AXIS2_PLACEMENT_3D('',#45020,#11435,#11436);
#9640=AXIS2_PLACEMENT_3D('',#45022,#11438,#11439);
#9641=AXIS2_PLACEMENT_3D('',#45024,#11441,#11442);
#9642=AXIS2_PLACEMENT_3D('',#45025,#11443,#11444);
#9643=AXIS2_PLACEMENT_3D('',#45028,#11447,#11448);
#9644=AXIS2_PLACEMENT_3D('',#45029,#11449,#11450);
#9645=AXIS2_PLACEMENT_3D('',#45031,#11452,#11453);
#9646=AXIS2_PLACEMENT_3D('',#45034,#11456,#11457);
#9647=AXIS2_PLACEMENT_3D('',#45037,#11460,#11461);
#9648=AXIS2_PLACEMENT_3D('',#45040,#11464,#11465);
#9649=AXIS2_PLACEMENT_3D('',#45043,#11468,#11469);
#9650=AXIS2_PLACEMENT_3D('',#45046,#11472,#11473);
#9651=AXIS2_PLACEMENT_3D('',#45047,#11474,#11475);
#9652=AXIS2_PLACEMENT_3D('',#45048,#11476,#11477);
#9653=AXIS2_PLACEMENT_3D('',#45049,#11478,#11479);
#9654=AXIS2_PLACEMENT_3D('',#45050,#11480,#11481);
#9655=AXIS2_PLACEMENT_3D('',#45051,#11482,#11483);
#9656=AXIS2_PLACEMENT_3D('',#45052,#11484,#11485);
#9657=AXIS2_PLACEMENT_3D('',#45054,#11487,#11488);
#9658=AXIS2_PLACEMENT_3D('',#45055,#11489,#11490);
#9659=AXIS2_PLACEMENT_3D('',#45057,#11492,#11493);
#9660=AXIS2_PLACEMENT_3D('',#45058,#11494,#11495);
#9661=AXIS2_PLACEMENT_3D('',#45059,#11496,#11497);
#9662=AXIS2_PLACEMENT_3D('',#45060,#11498,#11499);
#9663=AXIS2_PLACEMENT_3D('',#45061,#11500,#11501);
#9664=AXIS2_PLACEMENT_3D('',#45062,#11502,#11503);
#9665=AXIS2_PLACEMENT_3D('',#45063,#11504,#11505);
#9666=AXIS2_PLACEMENT_3D('',#45064,#11506,#11507);
#9667=AXIS2_PLACEMENT_3D('',#45065,#11508,#11509);
#9668=AXIS2_PLACEMENT_3D('',#45066,#11510,#11511);
#9669=AXIS2_PLACEMENT_3D('',#45067,#11512,#11513);
#9670=AXIS2_PLACEMENT_3D('',#45092,#11514,#11515);
#9671=AXIS2_PLACEMENT_3D('',#45105,#11516,#11517);
#9672=AXIS2_PLACEMENT_3D('',#45106,#11518,#11519);
#9673=AXIS2_PLACEMENT_3D('',#45107,#11520,#11521);
#9674=AXIS2_PLACEMENT_3D('',#45108,#11522,#11523);
#9675=AXIS2_PLACEMENT_3D('',#45109,#11524,#11525);
#9676=AXIS2_PLACEMENT_3D('',#45110,#11526,#11527);
#9677=AXIS2_PLACEMENT_3D('',#45111,#11528,#11529);
#9678=AXIS2_PLACEMENT_3D('',#45112,#11530,#11531);
#9679=AXIS2_PLACEMENT_3D('',#45113,#11532,#11533);
#9680=AXIS2_PLACEMENT_3D('',#45114,#11534,#11535);
#9681=AXIS2_PLACEMENT_3D('',#45139,#11536,#11537);
#9682=AXIS2_PLACEMENT_3D('',#45164,#11538,#11539);
#9683=AXIS2_PLACEMENT_3D('',#45189,#11540,#11541);
#9684=AXIS2_PLACEMENT_3D('',#45190,#11542,#11543);
#9685=AXIS2_PLACEMENT_3D('',#45191,#11544,#11545);
#9686=AXIS2_PLACEMENT_3D('',#45192,#11546,#11547);
#9687=AXIS2_PLACEMENT_3D('',#45193,#11548,#11549);
#9688=AXIS2_PLACEMENT_3D('',#45194,#11550,#11551);
#9689=AXIS2_PLACEMENT_3D('',#45195,#11552,#11553);
#9690=AXIS2_PLACEMENT_3D('',#45196,#11554,#11555);
#9691=AXIS2_PLACEMENT_3D('',#45197,#11556,#11557);
#9692=AXIS2_PLACEMENT_3D('',#45198,#11558,#11559);
#9693=AXIS2_PLACEMENT_3D('',#45199,#11560,#11561);
#9694=AXIS2_PLACEMENT_3D('',#45200,#11562,#11563);
#9695=AXIS2_PLACEMENT_3D('',#45201,#11564,#11565);
#9696=AXIS2_PLACEMENT_3D('',#45202,#11566,#11567);
#9697=AXIS2_PLACEMENT_3D('',#45203,#11568,#11569);
#9698=AXIS2_PLACEMENT_3D('',#45204,#11570,#11571);
#9699=AXIS2_PLACEMENT_3D('',#45205,#11572,#11573);
#9700=AXIS2_PLACEMENT_3D('',#45206,#11574,#11575);
#9701=AXIS2_PLACEMENT_3D('',#45207,#11576,#11577);
#9702=AXIS2_PLACEMENT_3D('',#45232,#11578,#11579);
#9703=AXIS2_PLACEMENT_3D('',#45245,#11580,#11581);
#9704=AXIS2_PLACEMENT_3D('',#45246,#11582,#11583);
#9705=AXIS2_PLACEMENT_3D('',#45249,#11584,#11585);
#9706=AXIS2_PLACEMENT_3D('',#45266,#11586,#11587);
#9707=AXIS2_PLACEMENT_3D('',#45288,#11588,#11589);
#9708=AXIS2_PLACEMENT_3D('',#45291,#11590,#11591);
#9709=AXIS2_PLACEMENT_3D('',#45308,#11592,#11593);
#9710=AXIS2_PLACEMENT_3D('',#45332,#11594,#11595);
#9711=AXIS2_PLACEMENT_3D('',#45335,#11596,#11597);
#9712=AXIS2_PLACEMENT_3D('',#45360,#11598,#11599);
#9713=AXIS2_PLACEMENT_3D('',#45377,#11600,#11601);
#9714=AXIS2_PLACEMENT_3D('',#45380,#11602,#11603);
#9715=AXIS2_PLACEMENT_3D('',#45405,#11604,#11605);
#9716=AXIS2_PLACEMENT_3D('',#45422,#11606,#11607);
#9717=AXIS2_PLACEMENT_3D('',#45425,#11608,#11609);
#9718=AXIS2_PLACEMENT_3D('',#45429,#11611,#11612);
#9719=AXIS2_PLACEMENT_3D('',#45431,#11614,#11615);
#9720=AXIS2_PLACEMENT_3D('',#45433,#11616,#11617);
#9721=AXIS2_PLACEMENT_3D('',#45436,#11619,#11620);
#9722=AXIS2_PLACEMENT_3D('',#45437,#11621,#11622);
#9723=AXIS2_PLACEMENT_3D('',#45439,#11623,#11624);
#9724=AXIS2_PLACEMENT_3D('',#45442,#11626,#11627);
#9725=AXIS2_PLACEMENT_3D('',#45443,#11628,#11629);
#9726=AXIS2_PLACEMENT_3D('',#45445,#11630,#11631);
#9727=AXIS2_PLACEMENT_3D('',#45448,#11633,#11634);
#9728=AXIS2_PLACEMENT_3D('',#45449,#11635,#11636);
#9729=AXIS2_PLACEMENT_3D('',#45453,#11638,#11639);
#9730=AXIS2_PLACEMENT_3D('',#45455,#11641,#11642);
#9731=AXIS2_PLACEMENT_3D('',#45457,#11643,#11644);
#9732=AXIS2_PLACEMENT_3D('',#45460,#11646,#11647);
#9733=AXIS2_PLACEMENT_3D('',#45461,#11648,#11649);
#9734=AXIS2_PLACEMENT_3D('',#45463,#11650,#11651);
#9735=AXIS2_PLACEMENT_3D('',#45466,#11653,#11654);
#9736=AXIS2_PLACEMENT_3D('',#45467,#11655,#11656);
#9737=AXIS2_PLACEMENT_3D('',#45469,#11657,#11658);
#9738=AXIS2_PLACEMENT_3D('',#45472,#11660,#11661);
#9739=AXIS2_PLACEMENT_3D('',#45473,#11662,#11663);
#9740=AXIS2_PLACEMENT_3D('',#45476,#11664,#11665);
#9741=AXIS2_PLACEMENT_3D('',#45479,#11668,#11669);
#9742=AXIS2_PLACEMENT_3D('',#45482,#11672,#11673);
#9743=AXIS2_PLACEMENT_3D('',#45486,#11676,#11677);
#9744=AXIS2_PLACEMENT_3D('',#45490,#11680,#11681);
#9745=AXIS2_PLACEMENT_3D('',#45496,#11685,#11686);
#9746=AXIS2_PLACEMENT_3D('',#45507,#11692,#11693);
#9747=AXIS2_PLACEMENT_3D('',#45508,#11694,#11695);
#9748=AXIS2_PLACEMENT_3D('',#45509,#11696,#11697);
#9749=AXIS2_PLACEMENT_3D('',#45521,#11703,#11704);
#9750=AXIS2_PLACEMENT_3D('',#45523,#11706,#11707);
#9751=AXIS2_PLACEMENT_3D('',#45524,#11708,#11709);
#9752=AXIS2_PLACEMENT_3D('',#45528,#11711,#11712);
#9753=AXIS2_PLACEMENT_3D('',#45538,#11718,#11719);
#9754=AXIS2_PLACEMENT_3D('',#45547,#11724,#11725);
#9755=AXIS2_PLACEMENT_3D('',#45549,#11726,#11727);
#9756=AXIS2_PLACEMENT_3D('',#45552,#11729,#11730);
#9757=AXIS2_PLACEMENT_3D('',#45553,#11731,#11732);
#9758=AXIS2_PLACEMENT_3D('',#45556,#11735,#11736);
#9759=AXIS2_PLACEMENT_3D('',#45562,#11740,#11741);
#9760=AXIS2_PLACEMENT_3D('',#45570,#11745,#11746);
#9761=AXIS2_PLACEMENT_3D('',#45574,#11749,#11750);
#9762=AXIS2_PLACEMENT_3D('',#45578,#11752,#11753);
#9763=AXIS2_PLACEMENT_3D('',#45579,#11754,#11755);
#9764=AXIS2_PLACEMENT_3D('',#45580,#11756,#11757);
#9765=AXIS2_PLACEMENT_3D('',#45587,#11760,#11761);
#9766=AXIS2_PLACEMENT_3D('',#45589,#11763,#11764);
#9767=AXIS2_PLACEMENT_3D('',#45592,#11765,#11766);
#9768=AXIS2_PLACEMENT_3D('',#45595,#11769,#11770);
#9769=AXIS2_PLACEMENT_3D('',#45596,#11771,#11772);
#9770=AXIS2_PLACEMENT_3D('',#45597,#11773,#11774);
#9771=AXIS2_PLACEMENT_3D('',#45598,#11775,#11776);
#9772=AXIS2_PLACEMENT_3D('',#45606,#11780,#11781);
#9773=AXIS2_PLACEMENT_3D('',#45607,#11782,#11783);
#9774=AXIS2_PLACEMENT_3D('',#45608,#11784,#11785);
#9775=AXIS2_PLACEMENT_3D('',#45609,#11786,#11787);
#9776=AXIS2_PLACEMENT_3D('',#45613,#11789,#11790);
#9777=AXIS2_PLACEMENT_3D('',#45617,#11793,#11794);
#9778=AXIS2_PLACEMENT_3D('',#45618,#11795,#11796);
#9779=AXIS2_PLACEMENT_3D('',#45624,#11799,#11800);
#9780=AXIS2_PLACEMENT_3D('',#45626,#11802,#11803);
#9781=AXIS2_PLACEMENT_3D('',#45637,#11810,#11811);
#9782=AXIS2_PLACEMENT_3D('',#45639,#11813,#11814);
#9783=AXIS2_PLACEMENT_3D('',#45640,#11815,#11816);
#9784=AXIS2_PLACEMENT_3D('',#45642,#11818,#11819);
#9785=AXIS2_PLACEMENT_3D('',#45647,#11823,#11824);
#9786=AXIS2_PLACEMENT_3D('',#45651,#11827,#11828);
#9787=AXIS2_PLACEMENT_3D('',#45652,#11829,#11830);
#9788=AXIS2_PLACEMENT_3D('',#45654,#11832,#11833);
#9789=AXIS2_PLACEMENT_3D('',#45742,#11834,#11835);
#9790=AXIS2_PLACEMENT_3D('',#45751,#11836,#11837);
#9791=AXIS2_PLACEMENT_3D('',#45839,#11838,#11839);
#9792=AXIS2_PLACEMENT_3D('',#45848,#11840,#11841);
#9793=AXIS2_PLACEMENT_3D('',#45849,#11842,#11843);
#9794=AXIS2_PLACEMENT_3D('',#45850,#11844,#11845);
#9795=AXIS2_PLACEMENT_3D('',#45853,#11847,#11848);
#9796=AXIS2_PLACEMENT_3D('',#45854,#11849,#11850);
#9797=AXIS2_PLACEMENT_3D('',#45865,#11851,#11852);
#9798=AXIS2_PLACEMENT_3D('',#45867,#11853,#11854);
#9799=AXIS2_PLACEMENT_3D('',#45868,#11855,#11856);
#9800=AXIS2_PLACEMENT_3D('',#45869,#11857,#11858);
#9801=AXIS2_PLACEMENT_3D('',#45871,#11860,#11861);
#9802=AXIS2_PLACEMENT_3D('',#45873,#11862,#11863);
#9803=AXIS2_PLACEMENT_3D('',#45875,#11865,#11866);
#9804=AXIS2_PLACEMENT_3D('',#45886,#11867,#11868);
#9805=AXIS2_PLACEMENT_3D('',#45888,#11869,#11870);
#9806=AXIS2_PLACEMENT_3D('',#45889,#11871,#11872);
#9807=AXIS2_PLACEMENT_3D('',#45890,#11873,#11874);
#9808=AXIS2_PLACEMENT_3D('',#45892,#11876,#11877);
#9809=AXIS2_PLACEMENT_3D('',#45893,#11878,#11879);
#9810=AXIS2_PLACEMENT_3D('',#45896,#11882,#11883);
#9811=AXIS2_PLACEMENT_3D('',#45897,#11884,#11885);
#9812=AXIS2_PLACEMENT_3D('',#45898,#11886,#11887);
#9813=AXIS2_PLACEMENT_3D('',#45899,#11888,#11889);
#9814=AXIS2_PLACEMENT_3D('',#45901,#11890,#11891);
#9815=AXIS2_PLACEMENT_3D('',#45903,#11892,#11893);
#9816=AXIS2_PLACEMENT_3D('',#45904,#11894,#11895);
#9817=AXIS2_PLACEMENT_3D('',#45906,#11896,#11897);
#9818=AXIS2_PLACEMENT_3D('',#45908,#11898,#11899);
#9819=AXIS2_PLACEMENT_3D('',#45909,#11900,#11901);
#9820=AXIS2_PLACEMENT_3D('',#45911,#11902,#11903);
#9821=AXIS2_PLACEMENT_3D('',#45914,#11905,#11906);
#9822=AXIS2_PLACEMENT_3D('',#45915,#11907,#11908);
#9823=AXIS2_PLACEMENT_3D('',#45916,#11909,#11910);
#9824=AXIS2_PLACEMENT_3D('',#45917,#11911,#11912);
#9825=AXIS2_PLACEMENT_3D('',#45918,#11913,#11914);
#9826=AXIS2_PLACEMENT_3D('',#45920,#11915,#11916);
#9827=AXIS2_PLACEMENT_3D('',#45921,#11917,#11918);
#9828=AXIS2_PLACEMENT_3D('',#45923,#11919,#11920);
#9829=AXIS2_PLACEMENT_3D('',#45926,#11922,#11923);
#9830=AXIS2_PLACEMENT_3D('',#45927,#11924,#11925);
#9831=AXIS2_PLACEMENT_3D('',#45929,#11926,#11927);
#9832=AXIS2_PLACEMENT_3D('',#45930,#11928,#11929);
#9833=AXIS2_PLACEMENT_3D('',#45931,#11930,#11931);
#9834=AXIS2_PLACEMENT_3D('',#45932,#11932,#11933);
#9835=AXIS2_PLACEMENT_3D('',#45933,#11934,#11935);
#9836=AXIS2_PLACEMENT_3D('',#45935,#11936,#11937);
#9837=AXIS2_PLACEMENT_3D('',#45939,#11939,#11940);
#9838=AXIS2_PLACEMENT_3D('',#45941,#11941,#11942);
#9839=AXIS2_PLACEMENT_3D('',#45942,#11943,#11944);
#9840=AXIS2_PLACEMENT_3D('',#45943,#11945,#11946);
#9841=AXIS2_PLACEMENT_3D('',#45946,#11947,#11948);
#9842=AXIS2_PLACEMENT_3D('',#45954,#11952,#11953);
#9843=AXIS2_PLACEMENT_3D('',#46082,#11955,#11956);
#9844=AXIS2_PLACEMENT_3D('',#46085,#11957,#11958);
#9845=AXIS2_PLACEMENT_3D('',#46088,#11960,#11961);
#9846=AXIS2_PLACEMENT_3D('',#46090,#11962,#11963);
#9847=AXIS2_PLACEMENT_3D('',#46091,#11964,#11965);
#9848=AXIS2_PLACEMENT_3D('',#46092,#11966,#11967);
#9849=AXIS2_PLACEMENT_3D('',#46138,#11974,#11975);
#9850=AXIS2_PLACEMENT_3D('',#46140,#11976,#11977);
#9851=AXIS2_PLACEMENT_3D('',#46141,#11978,#11979);
#9852=AXIS2_PLACEMENT_3D('',#46154,#11980,#11981);
#9853=AXIS2_PLACEMENT_3D('',#46159,#11983,#11984);
#9854=AXIS2_PLACEMENT_3D('',#46167,#11985,#11986);
#9855=AXIS2_PLACEMENT_3D('',#46247,#11987,#11988);
#9856=AXIS2_PLACEMENT_3D('',#46249,#11989,#11990);
#9857=AXIS2_PLACEMENT_3D('',#46414,#11994,#11995);
#9858=AXIS2_PLACEMENT_3D('',#46416,#11996,#11997);
#9859=AXIS2_PLACEMENT_3D('',#46429,#11998,#11999);
#9860=AXIS2_PLACEMENT_3D('',#46471,#12000,#12001);
#9861=AXIS2_PLACEMENT_3D('',#46725,#12003,#12004);
#9862=AXIS2_PLACEMENT_3D('',#47028,#12005,#12006);
#9863=AXIS2_PLACEMENT_3D('',#47029,#12007,#12008);
#9864=AXIS2_PLACEMENT_3D('',#47030,#12009,#12010);
#9865=AXIS2_PLACEMENT_3D('',#47031,#12011,#12012);
#9866=AXIS2_PLACEMENT_3D('',#47032,#12013,#12014);
#9867=AXIS2_PLACEMENT_3D('',#47139,#12015,#12016);
#9868=AXIS2_PLACEMENT_3D('',#47206,#12017,#12018);
#9869=AXIS2_PLACEMENT_3D('',#47309,#12019,#12020);
#9870=AXIS2_PLACEMENT_3D('',#47376,#12021,#12022);
#9871=AXIS2_PLACEMENT_3D('',#47413,#12023,#12024);
#9872=AXIS2_PLACEMENT_3D('',#47414,#12025,#12026);
#9873=AXIS2_PLACEMENT_3D('',#47416,#12027,#12028);
#9874=AXIS2_PLACEMENT_3D('',#47418,#12029,#12030);
#9875=AXIS2_PLACEMENT_3D('',#47419,#12031,#12032);
#9876=AXIS2_PLACEMENT_3D('',#47420,#12033,#12034);
#9877=AXIS2_PLACEMENT_3D('',#47423,#12035,#12036);
#9878=AXIS2_PLACEMENT_3D('',#47425,#12037,#12038);
#9879=AXIS2_PLACEMENT_3D('',#47427,#12039,#12040);
#9880=AXIS2_PLACEMENT_3D('',#47428,#12041,#12042);
#9881=AXIS2_PLACEMENT_3D('',#47429,#12043,#12044);
#9882=AXIS2_PLACEMENT_3D('',#47431,#12045,#12046);
#9883=AXIS2_PLACEMENT_3D('',#47433,#12047,#12048);
#9884=AXIS2_PLACEMENT_3D('',#47434,#12049,#12050);
#9885=AXIS2_PLACEMENT_3D('',#47435,#12051,#12052);
#9886=AXIS2_PLACEMENT_3D('',#47438,#12053,#12054);
#9887=AXIS2_PLACEMENT_3D('',#47440,#12055,#12056);
#9888=AXIS2_PLACEMENT_3D('',#47442,#12057,#12058);
#9889=AXIS2_PLACEMENT_3D('',#47443,#12059,#12060);
#9890=AXIS2_PLACEMENT_3D('',#47444,#12061,#12062);
#9891=AXIS2_PLACEMENT_3D('',#47446,#12063,#12064);
#9892=AXIS2_PLACEMENT_3D('',#47448,#12065,#12066);
#9893=AXIS2_PLACEMENT_3D('',#47449,#12067,#12068);
#9894=AXIS2_PLACEMENT_3D('',#47450,#12069,#12070);
#9895=AXIS2_PLACEMENT_3D('',#47452,#12071,#12072);
#9896=AXIS2_PLACEMENT_3D('',#47454,#12073,#12074);
#9897=AXIS2_PLACEMENT_3D('',#47455,#12075,#12076);
#9898=AXIS2_PLACEMENT_3D('',#47456,#12077,#12078);
#9899=AXIS2_PLACEMENT_3D('',#47458,#12080,#12081);
#9900=AXIS2_PLACEMENT_3D('',#47460,#12083,#12084);
#9901=AXIS2_PLACEMENT_3D('',#47463,#12087,#12088);
#9902=AXIS2_PLACEMENT_3D('',#47466,#12089,#12090);
#9903=AXIS2_PLACEMENT_3D('',#47467,#12091,#12092);
#9904=AXIS2_PLACEMENT_3D('',#47471,#12094,#12095);
#9905=AXIS2_PLACEMENT_3D('',#47475,#12097,#12098);
#9906=AXIS2_PLACEMENT_3D('',#47477,#12100,#12101);
#9907=AXIS2_PLACEMENT_3D('',#47480,#12102,#12103);
#9908=AXIS2_PLACEMENT_3D('',#47483,#12105,#12106);
#9909=AXIS2_PLACEMENT_3D('',#47485,#12107,#12108);
#9910=AXIS2_PLACEMENT_3D('',#47489,#12110,#12111);
#9911=AXIS2_PLACEMENT_3D('',#47491,#12113,#12114);
#9912=AXIS2_PLACEMENT_3D('',#47497,#12118,#12119);
#9913=AXIS2_PLACEMENT_3D('',#47501,#12121,#12122);
#9914=AXIS2_PLACEMENT_3D('',#47502,#12123,#12124);
#9915=AXIS2_PLACEMENT_3D('',#47503,#12125,#12126);
#9916=AXIS2_PLACEMENT_3D('',#47509,#12130,#12131);
#9917=AXIS2_PLACEMENT_3D('',#47513,#12133,#12134);
#9918=AXIS2_PLACEMENT_3D('',#47514,#12135,#12136);
#9919=AXIS2_PLACEMENT_3D('',#47515,#12137,#12138);
#9920=AXIS2_PLACEMENT_3D('',#47521,#12142,#12143);
#9921=AXIS2_PLACEMENT_3D('',#47525,#12145,#12146);
#9922=AXIS2_PLACEMENT_3D('',#47526,#12147,#12148);
#9923=AXIS2_PLACEMENT_3D('',#47527,#12149,#12150);
#9924=AXIS2_PLACEMENT_3D('',#47528,#12151,#12152);
#9925=AXIS2_PLACEMENT_3D('',#47529,#12153,#12154);
#9926=AXIS2_PLACEMENT_3D('',#47530,#12155,#12156);
#9927=AXIS2_PLACEMENT_3D('',#47545,#12157,#12158);
#9928=AXIS2_PLACEMENT_3D('',#47546,#12159,#12160);
#9929=AXIS2_PLACEMENT_3D('',#47559,#12161,#12162);
#9930=AXIS2_PLACEMENT_3D('',#47572,#12163,#12164);
#9931=AXIS2_PLACEMENT_3D('',#47601,#12165,#12166);
#9932=AXIS2_PLACEMENT_3D('',#47602,#12167,#12168);
#9933=AXIS2_PLACEMENT_3D('',#47603,#12169,#12170);
#9934=AXIS2_PLACEMENT_3D('',#47604,#12171,#12172);
#9935=AXIS2_PLACEMENT_3D('',#47605,#12173,#12174);
#9936=AXIS2_PLACEMENT_3D('',#47646,#12175,#12176);
#9937=AXIS2_PLACEMENT_3D('',#47647,#12177,#12178);
#9938=AXIS2_PLACEMENT_3D('',#47648,#12179,#12180);
#9939=AXIS2_PLACEMENT_3D('',#47649,#12181,#12182);
#9940=AXIS2_PLACEMENT_3D('',#47650,#12183,#12184);
#9941=AXIS2_PLACEMENT_3D('',#47651,#12185,#12186);
#9942=AXIS2_PLACEMENT_3D('',#47664,#12187,#12188);
#9943=AXIS2_PLACEMENT_3D('',#47677,#12189,#12190);
#9944=AXIS2_PLACEMENT_3D('',#47678,#12191,#12192);
#9945=AXIS2_PLACEMENT_3D('',#47679,#12193,#12194);
#9946=AXIS2_PLACEMENT_3D('',#47680,#12195,#12196);
#9947=AXIS2_PLACEMENT_3D('',#47681,#12197,#12198);
#9948=AXIS2_PLACEMENT_3D('',#47682,#12199,#12200);
#9949=AXIS2_PLACEMENT_3D('',#47683,#12201,#12202);
#9950=AXIS2_PLACEMENT_3D('',#47684,#12203,#12204);
#9951=AXIS2_PLACEMENT_3D('',#47685,#12205,#12206);
#9952=AXIS2_PLACEMENT_3D('',#47686,#12207,#12208);
#9953=AXIS2_PLACEMENT_3D('',#47687,#12209,#12210);
#9954=AXIS2_PLACEMENT_3D('',#47688,#12211,#12212);
#9955=AXIS2_PLACEMENT_3D('',#47689,#12213,#12214);
#9956=DIRECTION('axis',(0.,0.,1.));
#9957=DIRECTION('refdir',(1.,0.,0.));
#9958=DIRECTION('axis',(0.,0.,1.));
#9959=DIRECTION('refdir',(1.,0.,0.));
#9960=DIRECTION('center_axis',(0.,-1.,0.));
#9961=DIRECTION('ref_axis',(1.,0.,0.));
#9962=DIRECTION('center_axis',(2.50063434304147E-17,1.27632226958495E-16,
1.));
#9963=DIRECTION('ref_axis',(3.19161530011276E-33,-1.,1.27632226958495E-16));
#9964=DIRECTION('center_axis',(2.50063434304147E-17,1.27632226958495E-16,
1.));
#9965=DIRECTION('ref_axis',(3.19161530011276E-33,-1.,1.27632226958495E-16));
#9966=DIRECTION('center_axis',(2.50063434304147E-17,1.27632226958495E-16,
1.));
#9967=DIRECTION('ref_axis',(3.19161530011276E-33,-1.,1.27632226958495E-16));
#9968=DIRECTION('',(-2.50063434304147E-17,-1.27632226958495E-16,-1.));
#9969=DIRECTION('center_axis',(2.50063434304147E-17,1.27632226958495E-16,
1.));
#9970=DIRECTION('ref_axis',(3.19161530011276E-33,-1.,1.27632226958495E-16));
#9971=DIRECTION('center_axis',(0.,1.,0.));
#9972=DIRECTION('ref_axis',(1.,0.,0.));
#9973=DIRECTION('center_axis',(2.50063434304147E-17,1.27632226958495E-16,
1.));
#9974=DIRECTION('ref_axis',(3.19161530011276E-33,-1.,1.27632226958495E-16));
#9975=DIRECTION('center_axis',(2.50063434304147E-17,1.27632226958495E-16,
1.));
#9976=DIRECTION('ref_axis',(2.50063434304147E-17,-1.,1.27632226958495E-16));
#9977=DIRECTION('center_axis',(-2.50063434304147E-17,-1.27632226958495E-16,
-1.));
#9978=DIRECTION('ref_axis',(2.50063434304147E-17,-1.,1.27632226958495E-16));
#9979=DIRECTION('axis',(0.,0.,1.));
#9980=DIRECTION('refdir',(1.,0.,0.));
#9981=DIRECTION('center_axis',(0.981909603155918,0.18935028711409,1.69243964532307E-17));
#9982=DIRECTION('ref_axis',(0.,9.25185853854295E-17,-1.));
#9983=DIRECTION('center_axis',(0.099658045849521,-0.516794527976799,-0.850289180073869));
#9984=DIRECTION('ref_axis',(-0.177993700909268,-0.850018762193619,0.495768440257597));
#9985=DIRECTION('center_axis',(0.099658045849521,-0.516794527976799,-0.850289180073869));
#9986=DIRECTION('ref_axis',(-0.177993700909268,-0.850018762193619,0.495768440257597));
#9987=DIRECTION('center_axis',(-0.981909603155918,-0.18935028711409,-1.69243964532307E-17));
#9988=DIRECTION('ref_axis',(4.91815976796491E-19,8.68310150104084E-17,-1.));
#9989=DIRECTION('center_axis',(0.18935028711409,-0.981909603155918,4.32306217395459E-16));
#9990=DIRECTION('ref_axis',(-0.329651622039256,-0.063569629098379,0.941960036489437));
#9991=DIRECTION('center_axis',(0.18935028711409,-0.981909603155918,4.32306217395459E-16));
#9992=DIRECTION('ref_axis',(-0.329651622039256,-0.063569629098379,0.941960036489437));
#9993=DIRECTION('center_axis',(-0.981909603155918,-0.18935028711409,-1.69243964532307E-17));
#9994=DIRECTION('ref_axis',(0.,0.,1.));
#9995=DIRECTION('center_axis',(0.18935028711409,-0.981909603155918,-6.2240565599844E-16));
#9996=DIRECTION('ref_axis',(-1.17852689664738E-16,6.11146090683426E-16,
-1.));
#9997=DIRECTION('center_axis',(0.981909603155918,0.18935028711409,1.69243964532307E-17));
#9998=DIRECTION('ref_axis',(-1.66182274050451E-17,-3.20463932765191E-18,
1.));
#9999=DIRECTION('center_axis',(0.0996580458495207,-0.516794527976797,-0.85028918007387));
#10000=DIRECTION('ref_axis',(-0.161002500376988,0.834907111374105,-0.526315789473682));
#10001=DIRECTION('center_axis',(0.0996580458495207,-0.516794527976797,-0.85028918007387));
#10002=DIRECTION('ref_axis',(-0.161002500376988,0.834907111374105,-0.526315789473682));
#10003=DIRECTION('center_axis',(0.981909603155918,0.18935028711409,1.69243964532307E-17));
#10004=DIRECTION('ref_axis',(0.188087212577509,-0.975359705419448,-0.115311081466222));
#10005=DIRECTION('center_axis',(-0.981909603155918,-0.18935028711409,-1.69243964532307E-17));
#10006=DIRECTION('ref_axis',(0.188087212577511,-0.975359705419448,-0.115311081466224));
#10007=DIRECTION('center_axis',(-0.133890872037992,0.694314938903739,-0.70710678118655));
#10008=DIRECTION('ref_axis',(-0.133890872037987,0.694314938903745,0.707106781186545));
#10009=DIRECTION('center_axis',(-0.981909603155918,-0.18935028711409,-1.69243964532307E-17));
#10010=DIRECTION('ref_axis',(-0.188087212577509,0.975359705419448,0.115311081466222));
#10011=DIRECTION('center_axis',(-0.133890872037992,0.694314938903738,-0.707106781186551));
#10012=DIRECTION('ref_axis',(-0.203531771328762,-0.717586554283311,-0.666066329408401));
#10013=DIRECTION('center_axis',(0.981909603155918,0.18935028711409,1.69243964532307E-17));
#10014=DIRECTION('ref_axis',(-0.188087212577511,0.975359705419448,0.115311081466223));
#10015=DIRECTION('center_axis',(-0.18935028711409,0.981909603155918,6.72941436858614E-17));
#10016=DIRECTION('ref_axis',(0.981909603155918,0.18935028711409,8.26841968029962E-32));
#10017=DIRECTION('',(0.18935028711409,-0.981909603155918,-6.72941436858614E-17));
#10018=DIRECTION('center_axis',(0.18935028711409,-0.981909603155918,4.32306217395459E-16));
#10019=DIRECTION('ref_axis',(-0.329651622039256,-0.063569629098379,0.941960036489437));
#10020=DIRECTION('center_axis',(0.18935028711409,-0.981909603155918,4.32306217395459E-16));
#10021=DIRECTION('ref_axis',(-0.329651622039256,-0.063569629098379,0.941960036489437));
#10022=DIRECTION('center_axis',(0.18935028711409,-0.981909603155918,4.32306217395459E-16));
#10023=DIRECTION('ref_axis',(-0.329651622039256,-0.063569629098379,0.941960036489437));
#10024=DIRECTION('center_axis',(-0.650733917652094,-0.302831987743225,-0.696303206668362));
#10025=DIRECTION('ref_axis',(-0.734158582489553,0.484984699073061,0.475185245374835));
#10026=DIRECTION('center_axis',(-0.650733917651975,-0.302831987743205,-0.696303206668483));
#10027=DIRECTION('ref_axis',(-0.734238772574636,0.484644912666334,0.475407965304257));
#10028=DIRECTION('center_axis',(0.18935028711409,-0.981909603155918,1.5475046123917E-16));
#10029=DIRECTION('ref_axis',(2.93020442666747E-17,-1.51950963983549E-16,
-1.));
#10030=DIRECTION('center_axis',(-0.18935028711409,0.981909603155918,-7.59938514614303E-16));
#10031=DIRECTION('ref_axis',(-1.43894575931273E-16,7.46190925307827E-16,
1.));
#10032=DIRECTION('',(0.18935028711409,-0.981909603155918,7.59938514614303E-16));
#10033=DIRECTION('center_axis',(0.18935028711409,-0.981909603155918,1.5475046123917E-16));
#10034=DIRECTION('ref_axis',(2.93020442666747E-17,-1.51950963983549E-16,
-1.));
#10035=DIRECTION('center_axis',(-0.650733917652094,-0.302831987743225,-0.696303206668362));
#10036=DIRECTION('ref_axis',(-0.734158582489553,0.484984699073061,0.475185245374835));
#10037=DIRECTION('center_axis',(-0.650733917651975,-0.302831987743205,-0.696303206668483));
#10038=DIRECTION('ref_axis',(-0.734238772574636,0.484644912666334,0.475407965304257));
#10039=DIRECTION('center_axis',(-0.133890872037992,0.694314938903738,-0.707106781186551));
#10040=DIRECTION('ref_axis',(-0.203531771328761,-0.717586554283311,-0.666066329408402));
#10041=DIRECTION('center_axis',(-0.133890872037992,0.694314938903739,-0.70710678118655));
#10042=DIRECTION('ref_axis',(-0.133890872037993,0.694314938903744,0.707106781186545));
#10043=DIRECTION('axis',(0.,0.,1.));
#10044=DIRECTION('refdir',(1.,0.,0.));
#10045=DIRECTION('center_axis',(0.,-1.,0.));
#10046=DIRECTION('ref_axis',(1.,0.,0.));
#10047=DIRECTION('center_axis',(2.50063434304147E-17,1.27632226958495E-16,
1.));
#10048=DIRECTION('ref_axis',(3.19161530011276E-33,-1.,1.27632226958495E-16));
#10049=DIRECTION('center_axis',(2.50063434304147E-17,1.27632226958495E-16,
1.));
#10050=DIRECTION('ref_axis',(3.19161530011276E-33,-1.,1.27632226958495E-16));
#10051=DIRECTION('center_axis',(2.50063434304147E-17,1.27632226958495E-16,
1.));
#10052=DIRECTION('ref_axis',(3.19161530011276E-33,-1.,1.27632226958495E-16));
#10053=DIRECTION('',(-2.50063434304147E-17,-1.27632226958495E-16,-1.));
#10054=DIRECTION('center_axis',(2.50063434304147E-17,1.27632226958495E-16,
1.));
#10055=DIRECTION('ref_axis',(3.19161530011276E-33,-1.,1.27632226958495E-16));
#10056=DIRECTION('center_axis',(0.,1.,0.));
#10057=DIRECTION('ref_axis',(1.,0.,0.));
#10058=DIRECTION('center_axis',(2.50063434304147E-17,1.27632226958495E-16,
1.));
#10059=DIRECTION('ref_axis',(3.19161530011276E-33,-1.,1.27632226958495E-16));
#10060=DIRECTION('center_axis',(2.50063434304147E-17,1.27632226958495E-16,
1.));
#10061=DIRECTION('ref_axis',(2.50063434304147E-17,-1.,1.27632226958495E-16));
#10062=DIRECTION('center_axis',(-2.50063434304147E-17,-1.27632226958495E-16,
-1.));
#10063=DIRECTION('ref_axis',(2.50063434304147E-17,-1.,1.27632226958495E-16));
#10064=DIRECTION('axis',(0.,0.,1.));
#10065=DIRECTION('refdir',(1.,0.,0.));
#10066=DIRECTION('center_axis',(0.,0.,-1.));
#10067=DIRECTION('ref_axis',(-0.994365489657067,0.106006004448152,0.));
#10068=DIRECTION('center_axis',(0.,0.,-1.));
#10069=DIRECTION('ref_axis',(0.994365489657067,-0.106006004448146,0.));
#10070=DIRECTION('',(0.,0.,1.));
#10071=DIRECTION('center_axis',(0.,0.,1.));
#10072=DIRECTION('ref_axis',(0.994365489657067,-0.106006004448152,0.));
#10073=DIRECTION('',(0.,0.,-1.));
#10074=DIRECTION('center_axis',(0.,0.,-1.));
#10075=DIRECTION('ref_axis',(0.994365489657067,-0.106006004448153,0.));
#10076=DIRECTION('',(0.,0.,-1.));
#10077=DIRECTION('center_axis',(0.,0.,1.));
#10078=DIRECTION('ref_axis',(0.994365489657067,-0.106006004448152,0.));
#10079=DIRECTION('',(0.,0.,1.));
#10080=DIRECTION('center_axis',(0.,0.,1.));
#10081=DIRECTION('ref_axis',(0.994365489657067,-0.106006004448152,0.));
#10082=DIRECTION('center_axis',(0.,0.,-1.));
#10083=DIRECTION('ref_axis',(0.994365489657067,-0.106006004448152,0.));
#10084=DIRECTION('center_axis',(-0.568143764888917,0.822929317996295,-6.78809094260901E-15));
#10085=DIRECTION('ref_axis',(-0.822929317996295,-0.568143764888917,-2.73194523340008E-29));
#10086=DIRECTION('center_axis',(0.,0.,1.));
#10087=DIRECTION('ref_axis',(0.994365489657067,-0.106006004448152,0.));
#10088=DIRECTION('center_axis',(0.,0.,1.));
#10089=DIRECTION('ref_axis',(0.994365489657067,-0.106006004448152,0.));
#10090=DIRECTION('center_axis',(0.,0.,-1.));
#10091=DIRECTION('ref_axis',(0.994365489657067,-0.106006004448152,0.));
#10092=DIRECTION('center_axis',(-0.568143764888923,0.822929317996291,0.));
#10093=DIRECTION('ref_axis',(-0.822929317996291,-0.568143764888923,0.));
#10094=DIRECTION('center_axis',(0.,0.,1.));
#10095=DIRECTION('ref_axis',(0.994365489657067,-0.106006004448152,0.));
#10096=DIRECTION('center_axis',(0.,0.,1.));
#10097=DIRECTION('ref_axis',(0.994365489657067,-0.106006004448151,0.));
#10098=DIRECTION('center_axis',(0.,0.,1.));
#10099=DIRECTION('ref_axis',(-0.994365489657068,0.106006004448146,0.));
#10100=DIRECTION('center_axis',(0.,0.,-1.));
#10101=DIRECTION('ref_axis',(0.99436548965707,-0.106006004448119,0.));
#10102=DIRECTION('center_axis',(0.125069777171418,-0.992147948055995,-2.56328127499069E-6));
#10103=DIRECTION('ref_axis',(-0.000144711787631079,-1.5658743047867E-5,
-0.999999989406651));
#10104=DIRECTION('center_axis',(0.,0.,1.));
#10105=DIRECTION('ref_axis',(0.994365489657067,-0.106006004448151,0.));
#10106=DIRECTION('center_axis',(0.,0.,1.));
#10107=DIRECTION('ref_axis',(0.994365489657067,-0.106006004448152,0.));
#10108=DIRECTION('center_axis',(0.,0.,-1.));
#10109=DIRECTION('ref_axis',(-0.994365489657067,0.106006004448152,0.));
#10110=DIRECTION('center_axis',(0.125069777171398,-0.992147948055998,2.56328132497629E-6));
#10111=DIRECTION('ref_axis',(-0.85915326949364,-0.108303228584418,0.500126054306892));
#10112=DIRECTION('center_axis',(0.,0.,1.));
#10113=DIRECTION('ref_axis',(0.994365489657067,-0.106006004448152,0.));
#10114=DIRECTION('center_axis',(0.,0.,-1.));
#10115=DIRECTION('ref_axis',(0.994365489657067,-0.106006004448152,0.));
#10116=DIRECTION('center_axis',(0.,0.,-1.));
#10117=DIRECTION('ref_axis',(0.994365489657067,-0.106006004448152,0.));
#10118=DIRECTION('center_axis',(0.,0.,-1.));
#10119=DIRECTION('ref_axis',(0.994365489657068,-0.106006004448145,0.));
#10120=DIRECTION('center_axis',(0.,0.,1.));
#10121=DIRECTION('ref_axis',(0.994365489657067,-0.106006004448151,0.));
#10122=DIRECTION('center_axis',(0.,0.,1.));
#10123=DIRECTION('ref_axis',(0.994365489657067,-0.106006004448151,0.));
#10124=DIRECTION('',(0.,0.,1.));
#10125=DIRECTION('center_axis',(0.,0.,1.));
#10126=DIRECTION('ref_axis',(0.994365489657067,-0.106006004448151,0.));
#10127=DIRECTION('center_axis',(0.,0.,1.));
#10128=DIRECTION('ref_axis',(0.994365489657067,-0.106006004448151,0.));
#10129=DIRECTION('center_axis',(0.,0.,1.));
#10130=DIRECTION('ref_axis',(0.994365489657067,-0.106006004448151,0.));
#10131=DIRECTION('',(0.,0.,1.));
#10132=DIRECTION('center_axis',(0.,0.,1.));
#10133=DIRECTION('ref_axis',(0.994365489657067,-0.106006004448151,0.));
#10134=DIRECTION('center_axis',(0.,0.,-1.));
#10135=DIRECTION('ref_axis',(-0.994365489657067,0.106006004448152,0.));
#10136=DIRECTION('center_axis',(0.,0.,-1.));
#10137=DIRECTION('ref_axis',(0.994365489657067,-0.106006004448152,0.));
#10138=DIRECTION('',(0.,0.,1.));
#10139=DIRECTION('center_axis',(0.,0.,1.));
#10140=DIRECTION('ref_axis',(0.994365489657067,-0.106006004448152,0.));
#10141=DIRECTION('',(0.,0.,-1.));
#10142=DIRECTION('center_axis',(0.,0.,-1.));
#10143=DIRECTION('ref_axis',(-0.994365489657067,0.106006004448152,0.));
#10144=DIRECTION('center_axis',(0.,0.,-1.));
#10145=DIRECTION('ref_axis',(0.994365489657067,-0.106006004448152,0.));
#10146=DIRECTION('',(0.,0.,1.));
#10147=DIRECTION('center_axis',(0.,0.,1.));
#10148=DIRECTION('ref_axis',(0.994365489657067,-0.106006004448152,0.));
#10149=DIRECTION('',(0.,0.,-1.));
#10150=DIRECTION('center_axis',(-0.106006004448152,-0.994365489657067,0.));
#10151=DIRECTION('ref_axis',(0.994365489657067,-0.106006004448152,1.08418380562736E-14));
#10152=DIRECTION('',(-0.106006004448152,-0.994365489657067,0.));
#10153=DIRECTION('',(-0.106006004448152,-0.994365489657067,0.));
#10154=DIRECTION('center_axis',(-0.106006004448152,-0.994365489657067,0.));
#10155=DIRECTION('ref_axis',(0.,0.,-1.));
#10156=DIRECTION('',(0.106006004448152,0.994365489657067,0.));
#10157=DIRECTION('',(0.106006004448152,0.994365489657067,0.));
#10158=DIRECTION('center_axis',(-0.106006004448152,-0.994365489657067,0.));
#10159=DIRECTION('ref_axis',(0.,0.,-1.));
#10160=DIRECTION('',(-0.106006004448152,-0.994365489657067,0.));
#10161=DIRECTION('',(-0.106006004448152,-0.994365489657067,0.));
#10162=DIRECTION('center_axis',(-0.106006004448152,-0.994365489657067,0.));
#10163=DIRECTION('ref_axis',(0.994365489657067,-0.106006004448152,-4.06725102863337E-14));
#10164=DIRECTION('',(-0.106006004448152,-0.994365489657067,0.));
#10165=DIRECTION('',(-0.106006004448152,-0.994365489657067,0.));
#10166=DIRECTION('center_axis',(-0.106006004448152,-0.994365489657067,0.));
#10167=DIRECTION('ref_axis',(0.994365489657067,-0.106006004448152,5.51276753807285E-15));
#10168=DIRECTION('',(-0.106006004448152,-0.994365489657067,0.));
#10169=DIRECTION('center_axis',(-0.106006004448152,-0.994365489657067,0.));
#10170=DIRECTION('ref_axis',(0.,0.,-1.));
#10171=DIRECTION('',(-0.106006004448152,-0.994365489657067,0.));
#10172=DIRECTION('center_axis',(-0.106006004448152,-0.994365489657067,0.));
#10173=DIRECTION('ref_axis',(0.,0.,-1.));
#10174=DIRECTION('',(-0.106006004448152,-0.994365489657067,0.));
#10175=DIRECTION('',(-0.104595521960225,-0.994514394606886,0.000946417226730482));
#10176=DIRECTION('center_axis',(-0.106006004448152,-0.994365489657067,0.));
#10177=DIRECTION('ref_axis',(0.,0.,-1.));
#10178=DIRECTION('',(-0.106006004448152,-0.994365489657067,0.));
#10179=DIRECTION('',(-0.104644914852541,-0.994509228045758,0.000914946629410067));
#10180=DIRECTION('center_axis',(-0.106006004448152,-0.994365489657067,0.));
#10181=DIRECTION('ref_axis',(0.,0.,-1.));
#10182=DIRECTION('',(-0.106006004448152,-0.994365489657067,0.));
#10183=DIRECTION('',(-0.104789157575189,-0.994494123194127,0.000819382100487921));
#10184=DIRECTION('center_axis',(-0.106006004448152,-0.994365489657067,0.));
#10185=DIRECTION('ref_axis',(0.,0.,-1.));
#10186=DIRECTION('',(-0.106006004448152,-0.994365489657067,0.));
#10187=DIRECTION('',(-0.105011768308297,-0.994470753208597,0.000670469604745426));
#10188=DIRECTION('center_axis',(-0.106006004448152,-0.994365489657067,0.));
#10189=DIRECTION('ref_axis',(0.,0.,-1.));
#10190=DIRECTION('',(-0.106006004448152,-0.994365489657067,0.));
#10191=DIRECTION('',(-0.105293840413202,-0.994441036965239,0.000480801975987768));
#10192=DIRECTION('center_axis',(-0.106006004448152,-0.994365489657067,0.));
#10193=DIRECTION('ref_axis',(0.,0.,-1.));
#10194=DIRECTION('',(-0.106006004448152,-0.994365489657067,0.));
#10195=DIRECTION('',(-0.10561478582907,-0.994407083215312,0.000264320818382655));
#10196=DIRECTION('center_axis',(-0.106006004448152,-0.994365489657067,0.));
#10197=DIRECTION('ref_axis',(0.,0.,-1.));
#10198=DIRECTION('',(-0.106006004448152,-0.994365489657067,0.));
#10199=DIRECTION('',(-0.105953253909959,-0.994371111162663,3.56514048180235E-5));
#10200=DIRECTION('center_axis',(0.,0.,1.));
#10201=DIRECTION('ref_axis',(0.994365489657067,-0.106006004448152,0.));
#10202=DIRECTION('center_axis',(-5.29294451150809E-11,5.6426324652942E-12,
1.));
#10203=DIRECTION('ref_axis',(0.775613864659347,0.6312076781442,3.74911385429433E-11));
#10204=DIRECTION('',(0.994365489657067,-0.106006004448152,0.));
#10205=DIRECTION('',(-0.106006004448152,-0.994365489657067,0.));
#10206=DIRECTION('center_axis',(-5.29294451147456E-11,5.64263246525919E-12,
1.));
#10207=DIRECTION('ref_axis',(0.775613853926467,0.631207691332523,3.7491137900203E-11));
#10208=DIRECTION('',(-0.106006004448152,-0.994365489657067,0.));
#10209=DIRECTION('center_axis',(-4.940081544063E-11,5.26645696759596E-12,
1.));
#10210=DIRECTION('ref_axis',(0.775613813195398,0.631207741381943,3.49917264312677E-11));
#10211=DIRECTION('',(-0.106006004448152,-0.994365489657067,0.));
#10212=DIRECTION('center_axis',(-5.1157602968305E-11,5.52519915316751E-12,
1.));
#10213=DIRECTION('ref_axis',(0.775613834257577,0.631207715501212,3.61909962545137E-11));
#10214=DIRECTION('',(-0.106006004448152,-0.994365489657067,0.));
#10215=DIRECTION('center_axis',(-5.4686232642848E-11,5.90137465087394E-12,
1.));
#10216=DIRECTION('ref_axis',(0.7756138251515,0.631207726690555,3.86904048055168E-11));
#10217=DIRECTION('',(-0.106006004448152,-0.994365489657067,0.));
#10218=DIRECTION('center_axis',(-5.64580747891702E-11,6.01880796295792E-12,
1.));
#10219=DIRECTION('ref_axis',(0.775613814734935,0.631207739490195,3.99905445910943E-11));
#10220=DIRECTION('',(-0.106006004448152,-0.994365489657067,0.));
#10221=DIRECTION('center_axis',(-5.46862326427878E-11,5.90137465086926E-12,
1.));
#10222=DIRECTION('ref_axis',(0.775613821569081,0.631207731092551,3.86904045835862E-11));
#10223=DIRECTION('',(-0.106006004448152,-0.994365489657067,0.));
#10224=DIRECTION('',(0.994365489657067,-0.106006004448152,0.));
#10225=DIRECTION('',(0.106006004448152,0.994365489657067,0.));
#10226=DIRECTION('center_axis',(0.,0.,1.));
#10227=DIRECTION('ref_axis',(0.994365489657067,-0.106006004448152,0.));
#10228=DIRECTION('',(-0.0682742201674492,0.997666593036234,0.));
#10229=DIRECTION('center_axis',(0.,0.,-1.));
#10230=DIRECTION('ref_axis',(0.994365489657067,-0.106006004448152,0.));
#10231=DIRECTION('',(-0.992147762966023,-0.125071245462399,0.));
#10232=DIRECTION('',(0.994365489657067,-0.106006004448152,0.));
#10233=DIRECTION('center_axis',(-4.94008154407823E-11,5.26645696761484E-12,
1.));
#10234=DIRECTION('ref_axis',(0.775613862100156,0.631207681288877,3.49917291637863E-11));
#10235=DIRECTION('center_axis',(-4.94008154408169E-11,5.266456967615E-12,
1.));
#10236=DIRECTION('ref_axis',(0.775613846609227,0.631207700323783,3.49917282983021E-11));
#10237=DIRECTION('',(0.105718986639004,0.994396026866766,0.000193947443827362));
#10238=DIRECTION('',(0.105390335156554,0.99443084444827,0.000415770959693973));
#10239=DIRECTION('',(0.105093973279893,0.994462104966823,0.000615276524171631));
#10240=DIRECTION('',(0.104850811522338,0.994487657870431,0.000778245777930233));
#10241=DIRECTION('',(0.104680345174056,0.994505520521614,0.000891620028430924));
#10242=DIRECTION('',(0.104599853734027,0.994513941261197,0.000944052933083771));
#10243=DIRECTION('center_axis',(-0.106006004448152,-0.994365489657067,0.));
#10244=DIRECTION('ref_axis',(0.00297357138932237,-0.00031700257621784,0.999995528681283));
#10245=DIRECTION('center_axis',(-0.106006004448152,-0.994365489657067,0.));
#10246=DIRECTION('ref_axis',(0.0028493267959079,-0.000303757272494865,0.999995894525737));
#10247=DIRECTION('center_axis',(-0.106006004448152,-0.994365489657067,0.));
#10248=DIRECTION('ref_axis',(0.00262933317937824,-0.000280304483218709,
0.999996504012103));
#10249=DIRECTION('center_axis',(-0.106006004448152,-0.994365489657067,0.));
#10250=DIRECTION('ref_axis',(0.00232579287797141,-0.000247945059168078,
0.999997264601627));
#10251=DIRECTION('center_axis',(-0.106006004448152,-0.994365489657067,0.));
#10252=DIRECTION('ref_axis',(0.00195706334323466,-0.000208636027322103,
0.999998063185164));
#10253=DIRECTION('center_axis',(-0.106006004448152,-0.994365489657067,0.));
#10254=DIRECTION('ref_axis',(0.00154710569925948,-0.000164931803590671,
0.999998789629995));
#10255=DIRECTION('center_axis',(-0.106006004448152,-0.994365489657067,0.));
#10256=DIRECTION('ref_axis',(-0.164515306403286,0.0175384307719592,0.986218595142624));
#10257=DIRECTION('center_axis',(-0.106006004448152,-0.994365489657067,0.));
#10258=DIRECTION('ref_axis',(0.,0.,-1.));
#10259=DIRECTION('center_axis',(-0.106006004448152,-0.994365489657067,0.));
#10260=DIRECTION('ref_axis',(0.,0.,-1.));
#10261=DIRECTION('',(0.,0.,-1.));
#10262=DIRECTION('center_axis',(0.,0.,1.));
#10263=DIRECTION('ref_axis',(0.994365489657067,-0.106006004448152,0.));
#10264=DIRECTION('',(-0.992147762966023,-0.125071245462401,0.));
#10265=DIRECTION('center_axis',(0.,0.,-1.));
#10266=DIRECTION('ref_axis',(0.994365489657067,-0.106006004448152,0.));
#10267=DIRECTION('center_axis',(0.,0.,-1.));
#10268=DIRECTION('ref_axis',(0.994365489657067,-0.10600600444815,0.));
#10269=DIRECTION('center_axis',(0.,0.,1.));
#10270=DIRECTION('ref_axis',(0.994365489657067,-0.106006004448152,0.));
#10271=DIRECTION('',(-0.125071245462401,0.992147762966023,0.));
#10272=DIRECTION('center_axis',(0.125071245462402,-0.992147762966023,0.));
#10273=DIRECTION('ref_axis',(0.992147762966023,0.125071245462402,0.));
#10274=DIRECTION('',(-0.992147762966023,-0.125071245462401,0.));
#10275=DIRECTION('center_axis',(0.125071245462402,-0.992147762966023,0.));
#10276=DIRECTION('ref_axis',(0.992147762966023,0.125071245462401,0.));
#10277=DIRECTION('',(0.,0.,-1.));
#10278=DIRECTION('',(-0.992147762966023,-0.125071245462401,0.));
#10279=DIRECTION('center_axis',(0.125071245462402,-0.992147762966023,0.));
#10280=DIRECTION('ref_axis',(0.992147762966023,0.125071245462401,0.));
#10281=DIRECTION('',(0.992147762966023,0.125071245462401,0.));
#10282=DIRECTION('',(0.,0.,-1.));
#10283=DIRECTION('center_axis',(0.997666593036234,0.0682742201674492,0.));
#10284=DIRECTION('ref_axis',(-0.0682742201674492,0.997666593036234,0.));
#10285=DIRECTION('',(0.0682742201674492,-0.997666593036234,0.));
#10286=DIRECTION('',(0.,0.,1.));
#10287=DIRECTION('',(0.0682742201674492,-0.997666593036234,0.));
#10288=DIRECTION('center_axis',(0.994365489657067,-0.106006004448152,0.));
#10289=DIRECTION('ref_axis',(0.,0.,-1.));
#10290=DIRECTION('',(0.,0.,-1.));
#10291=DIRECTION('',(-0.106006004448152,-0.994365489657067,0.));
#10292=DIRECTION('',(0.,0.,-1.));
#10293=DIRECTION('',(-0.106006004448152,-0.994365489657067,0.));
#10294=DIRECTION('center_axis',(0.106006004448152,0.994365489657067,0.));
#10295=DIRECTION('ref_axis',(0.,0.,1.));
#10296=DIRECTION('',(0.994365489657067,-0.106006004448152,0.));
#10297=DIRECTION('center_axis',(-0.106006004448152,-0.994365489657067,0.));
#10298=DIRECTION('ref_axis',(0.,0.,1.));
#10299=DIRECTION('',(0.994365489657067,-0.106006004448152,0.));
#10300=DIRECTION('center_axis',(-0.106006004448152,-0.994365489657067,0.));
#10301=DIRECTION('ref_axis',(0.,0.,1.));
#10302=DIRECTION('',(0.,0.,-1.));
#10303=DIRECTION('center_axis',(-0.106006004448152,-0.994365489657067,0.));
#10304=DIRECTION('ref_axis',(0.,0.,1.));
#10305=DIRECTION('',(0.994365489657067,-0.106006004448152,0.));
#10306=DIRECTION('center_axis',(-0.106006004448152,-0.994365489657067,0.));
#10307=DIRECTION('ref_axis',(0.,0.,1.));
#10308=DIRECTION('',(0.,0.,-1.));
#10309=DIRECTION('center_axis',(-0.106006004448152,-0.994365489657067,0.));
#10310=DIRECTION('ref_axis',(0.,0.,1.));
#10311=DIRECTION('center_axis',(-0.106006004448152,-0.994365489657067,0.));
#10312=DIRECTION('ref_axis',(0.990000482593489,-0.105540665533024,-0.093596006236942));
#10313=DIRECTION('',(0.,0.,-1.));
#10314=DIRECTION('center_axis',(-0.106006004448152,-0.994365489657067,0.));
#10315=DIRECTION('ref_axis',(0.,0.,1.));
#10316=DIRECTION('center_axis',(0.,0.,1.));
#10317=DIRECTION('ref_axis',(0.994365489657067,-0.106006004448152,0.));
#10318=DIRECTION('',(0.,0.,1.));
#10319=DIRECTION('center_axis',(0.,0.,-1.));
#10320=DIRECTION('ref_axis',(0.994365489657065,-0.106006004448171,0.));
#10321=DIRECTION('',(0.,0.,-1.));
#10322=DIRECTION('center_axis',(0.,0.,1.));
#10323=DIRECTION('ref_axis',(0.994365489657067,-0.106006004448152,0.));
#10324=DIRECTION('',(0.,0.,1.));
#10325=DIRECTION('center_axis',(0.997666593036234,0.0682742201674492,0.));
#10326=DIRECTION('ref_axis',(-0.0682742201674492,0.997666593036234,0.));
#10327=DIRECTION('',(0.0682742201674492,-0.997666593036234,0.));
#10328=DIRECTION('',(-0.0682742201674492,0.997666593036234,0.));
#10329=DIRECTION('center_axis',(0.994365489657067,-0.106006004448152,0.));
#10330=DIRECTION('ref_axis',(0.,0.,-1.));
#10331=DIRECTION('',(-0.106006004448152,-0.994365489657067,0.));
#10332=DIRECTION('',(0.106006004448152,0.994365489657067,0.));
#10333=DIRECTION('center_axis',(0.,0.,1.));
#10334=DIRECTION('ref_axis',(0.994365489657067,-0.106006004448152,0.));
#10335=DIRECTION('',(-0.992147762966023,-0.125071245462401,0.));
#10336=DIRECTION('center_axis',(0.,0.,1.));
#10337=DIRECTION('ref_axis',(0.994365489657067,-0.106006004448152,0.));
#10338=DIRECTION('',(0.0682742201674492,-0.997666593036234,0.));
#10339=DIRECTION('center_axis',(0.,0.,-1.));
#10340=DIRECTION('ref_axis',(0.994365489657065,-0.106006004448169,0.));
#10341=DIRECTION('',(-0.106006004448152,-0.994365489657067,0.));
#10342=DIRECTION('center_axis',(0.,0.,1.));
#10343=DIRECTION('ref_axis',(0.994365489657067,-0.106006004448152,0.));
#10344=DIRECTION('',(0.106006004448152,0.994365489657067,0.));
#10345=DIRECTION('center_axis',(0.,0.,1.));
#10346=DIRECTION('ref_axis',(0.994365489657067,-0.106006004448152,0.));
#10347=DIRECTION('',(-0.0682742201674492,0.997666593036234,0.));
#10348=DIRECTION('center_axis',(0.,0.,-1.));
#10349=DIRECTION('ref_axis',(0.994365489657067,-0.106006004448152,0.));
#10350=DIRECTION('',(0.992147762966023,0.125071245462401,0.));
#10351=DIRECTION('center_axis',(0.,0.,1.));
#10352=DIRECTION('ref_axis',(0.994365489657067,-0.106006004448152,0.));
#10353=DIRECTION('center_axis',(0.,0.,-1.));
#10354=DIRECTION('ref_axis',(0.994365489657065,-0.106006004448171,0.));
#10355=DIRECTION('center_axis',(0.,0.,1.));
#10356=DIRECTION('ref_axis',(0.994365489657067,-0.106006004448152,0.));
#10357=DIRECTION('',(-0.106092348033695,-0.994356281062627,0.));
#10358=DIRECTION('center_axis',(0.,0.,1.));
#10359=DIRECTION('ref_axis',(0.994365489657067,-0.106006004448152,0.));
#10360=DIRECTION('center_axis',(4.31480997391025E-8,-4.59987570007986E-9,
0.999999999999999));
#10361=DIRECTION('ref_axis',(0.551662933371381,-0.834067148342435,-2.76398124793695E-8));
#10362=DIRECTION('center_axis',(4.31463281213693E-8,-4.59975829069094E-9,
0.999999999999999));
#10363=DIRECTION('ref_axis',(0.551662908720544,-0.834067164646822,-2.76387362276229E-8));
#10364=DIRECTION('center_axis',(4.31480997391815E-8,-4.59987570008751E-9,
0.999999999999999));
#10365=DIRECTION('ref_axis',(0.551662934443112,-0.834067147633579,-2.7639812522402E-8));
#10366=DIRECTION('',(0.994365489657067,-0.106006004448152,0.));
#10367=DIRECTION('',(-0.992147762966023,-0.125071245462399,0.));
#10368=DIRECTION('center_axis',(7.37052354886326E-6,-1.28250520570221E-6,
0.999999999972015));
#10369=DIRECTION('ref_axis',(0.8981791063997,-0.43962972235215,-7.18387766251503E-6));
#10370=DIRECTION('center_axis',(4.31480997391323E-8,-4.59987570008457E-9,
0.999999999999999));
#10371=DIRECTION('ref_axis',(0.55166291981908,-0.834067157306105,-2.76398119358656E-8));
#10372=DIRECTION('center_axis',(4.31445711081758E-8,-4.59949952444789E-9,
0.999999999999999));
#10373=DIRECTION('ref_axis',(0.551662901360848,-0.83406716951462,-2.76375508250458E-8));
#10374=DIRECTION('center_axis',(4.3144571108166E-8,-4.59949952444854E-9,
0.999999999999999));
#10375=DIRECTION('ref_axis',(0.551662893412369,-0.834067174771848,-2.76375505062878E-8));
#10376=DIRECTION('center_axis',(4.31480851344174E-8,-4.60001705691756E-9,
0.999999999999999));
#10377=DIRECTION('ref_axis',(0.55166290335284,-0.834067168197091,-2.76399211196898E-8));
#10378=DIRECTION('center_axis',(4.31480997391094E-8,-4.59987570007966E-9,
0.999999999999999));
#10379=DIRECTION('ref_axis',(0.551662947457436,-0.834067139025734,-2.7639813044304E-8));
#10380=DIRECTION('center_axis',(4.31498421474835E-8,-4.60027582314505E-9,
0.999999999999999));
#10381=DIRECTION('ref_axis',(0.551662900079072,-0.834067170362404,-2.76411060957321E-8));
#10382=DIRECTION('',(0.994365489657067,-0.106006004448152,0.));
#10383=DIRECTION('',(-0.106006004448152,-0.994365489657067,0.));
#10384=DIRECTION('center_axis',(0.10614193441841,0.994350989134504,-1.28511006137957E-5));
#10385=DIRECTION('ref_axis',(0.261552703869028,-0.0279069580928212,0.964785667798193));
#10386=DIRECTION('center_axis',(0.125071245462399,-0.992147762966023,0.));
#10387=DIRECTION('ref_axis',(0.992147762966023,0.125071245462399,0.));
#10388=DIRECTION('center_axis',(0.,0.,1.));
#10389=DIRECTION('ref_axis',(0.994365489657067,-0.106006004448152,0.));
#10390=DIRECTION('center_axis',(0.,0.,-1.));
#10391=DIRECTION('ref_axis',(0.994365489657067,-0.106006004448151,0.));
#10392=DIRECTION('center_axis',(0.,0.,1.));
#10393=DIRECTION('ref_axis',(0.994365489657067,-0.106006004448152,0.));
#10394=DIRECTION('center_axis',(0.,0.,1.));
#10395=DIRECTION('ref_axis',(0.994365489657067,-0.106006004448152,0.));
#10396=DIRECTION('',(0.125071245462401,-0.992147762966023,0.));
#10397=DIRECTION('center_axis',(0.,0.,-1.));
#10398=DIRECTION('ref_axis',(0.961056660210967,0.276351399244047,0.));
#10399=DIRECTION('',(0.,0.,-1.));
#10400=DIRECTION('center_axis',(0.232004772421175,0.972714647557956,0.));
#10401=DIRECTION('ref_axis',(-0.972714647557956,0.232004772421175,0.));
#10402=DIRECTION('',(0.972714647557956,-0.232004772421175,0.));
#10403=DIRECTION('',(0.972714647557956,-0.232004772421175,0.));
#10404=DIRECTION('',(0.,0.,-1.));
#10405=DIRECTION('center_axis',(-0.992147762966023,-0.125071245462401,0.));
#10406=DIRECTION('ref_axis',(0.125071245462401,-0.992147762966023,0.));
#10407=DIRECTION('',(0.,0.,1.));
#10408=DIRECTION('',(-0.125071245462401,0.992147762966023,0.));
#10409=DIRECTION('',(-0.125071245462401,0.992147762966023,0.));
#10410=DIRECTION('center_axis',(0.,0.,-1.));
#10411=DIRECTION('ref_axis',(0.884759974153376,-0.466046980610451,0.));
#10412=DIRECTION('center_axis',(0.,0.,1.));
#10413=DIRECTION('ref_axis',(0.994365489657067,-0.106006004448152,0.));
#10414=DIRECTION('center_axis',(0.,0.,-1.));
#10415=DIRECTION('ref_axis',(0.994365489657067,-0.106006004448152,0.));
#10416=DIRECTION('',(0.,0.,1.));
#10417=DIRECTION('center_axis',(0.,0.,1.));
#10418=DIRECTION('ref_axis',(0.994365489657067,-0.106006004448152,0.));
#10419=DIRECTION('center_axis',(0.,0.,1.));
#10420=DIRECTION('ref_axis',(0.994365489657067,-0.106006004448152,0.));
#10421=DIRECTION('',(0.,0.,1.));
#10422=DIRECTION('center_axis',(0.,0.,1.));
#10423=DIRECTION('ref_axis',(0.994365489657067,-0.106006004448152,0.));
#10424=DIRECTION('',(0.125071245462401,-0.992147762966023,0.));
#10425=DIRECTION('center_axis',(0.,0.,1.));
#10426=DIRECTION('ref_axis',(0.994365489657067,-0.106006004448152,0.));
#10427=DIRECTION('',(-0.789993136930247,0.61311568533443,0.));
#10428=DIRECTION('',(0.613115685334428,0.789993136930249,0.));
#10429=DIRECTION('',(-0.789993136930257,0.613115685334417,0.));
#10430=DIRECTION('',(0.613115685334426,0.78999313693025,0.));
#10431=DIRECTION('',(-0.789993136930246,0.613115685334431,0.));
#10432=DIRECTION('',(0.613115685334426,0.78999313693025,0.));
#10433=DIRECTION('',(-0.789993136930246,0.613115685334431,0.));
#10434=DIRECTION('',(0.613115685334426,0.78999313693025,0.));
#10435=DIRECTION('',(-0.789993136930246,0.613115685334431,0.));
#10436=DIRECTION('',(0.613115685334426,0.78999313693025,0.));
#10437=DIRECTION('',(-0.789993136930246,0.613115685334431,0.));
#10438=DIRECTION('',(0.613115685334426,0.78999313693025,0.));
#10439=DIRECTION('',(-0.789993136930246,0.613115685334431,0.));
#10440=DIRECTION('',(0.613115685334426,0.78999313693025,0.));
#10441=DIRECTION('',(-0.789993136930246,0.613115685334431,0.));
#10442=DIRECTION('',(0.613115685334426,0.78999313693025,0.));
#10443=DIRECTION('',(-0.789993136930246,0.613115685334431,0.));
#10444=DIRECTION('',(0.613115685334426,0.78999313693025,0.));
#10445=DIRECTION('',(0.992014908988184,0.126120657884284,0.));
#10446=DIRECTION('center_axis',(0.859225167036477,0.108314875853399,0.500000000000001));
#10447=DIRECTION('ref_axis',(0.50730728131349,-0.05408234545433,-0.860066521983314));
#10448=DIRECTION('',(-0.125071245462401,0.992147762966023,-1.16159728063882E-17));
#10449=DIRECTION('',(-0.496073881483013,-0.0625356227312008,0.866025403784438));
#10450=DIRECTION('center_axis',(0.859225167036477,0.108314875853399,-0.500000000000001));
#10451=DIRECTION('ref_axis',(-0.50730728131349,0.05408234545433,-0.860066521983314));
#10452=DIRECTION('',(0.496073881483013,0.0625356227312008,0.866025403784438));
#10453=DIRECTION('',(0.125071245462401,-0.992147762966023,-1.46206020038625E-17));
#10454=DIRECTION('',(0.125071245462401,-0.992147762966023,0.));
#10455=DIRECTION('center_axis',(0.,0.,1.));
#10456=DIRECTION('ref_axis',(0.994365489657067,-0.106006004448152,0.));
#10457=DIRECTION('',(0.992014908988184,0.126120657884284,0.));
#10458=DIRECTION('',(0.613115685334426,0.78999313693025,0.));
#10459=DIRECTION('',(-0.789993136930246,0.613115685334431,0.));
#10460=DIRECTION('',(0.613115685334426,0.78999313693025,0.));
#10461=DIRECTION('',(-0.789993136930246,0.613115685334431,0.));
#10462=DIRECTION('',(0.613115685334426,0.78999313693025,0.));
#10463=DIRECTION('',(-0.789993136930246,0.613115685334431,0.));
#10464=DIRECTION('',(0.613115685334426,0.78999313693025,0.));
#10465=DIRECTION('',(-0.789993136930246,0.613115685334431,0.));
#10466=DIRECTION('',(0.613115685334426,0.78999313693025,0.));
#10467=DIRECTION('',(-0.789993136930246,0.613115685334431,0.));
#10468=DIRECTION('',(0.613115685334426,0.78999313693025,0.));
#10469=DIRECTION('',(-0.789993136930246,0.613115685334431,0.));
#10470=DIRECTION('',(0.613115685334426,0.78999313693025,0.));
#10471=DIRECTION('',(-0.789993136930246,0.613115685334431,0.));
#10472=DIRECTION('',(0.613115685334426,0.78999313693025,0.));
#10473=DIRECTION('',(-0.789993136930257,0.613115685334417,0.));
#10474=DIRECTION('',(0.613115685334428,0.789993136930249,0.));
#10475=DIRECTION('',(-0.789993136930247,0.61311568533443,0.));
#10476=DIRECTION('center_axis',(0.,0.,-1.));
#10477=DIRECTION('ref_axis',(0.994365489657067,-0.106006004448149,0.));
#10478=DIRECTION('center_axis',(0.,0.,1.));
#10479=DIRECTION('ref_axis',(0.994365489657067,-0.106006004448152,0.));
#10480=DIRECTION('center_axis',(0.,0.,-1.));
#10481=DIRECTION('ref_axis',(-0.994365489657067,0.106006004448152,0.));
#10482=DIRECTION('center_axis',(0.,0.,-1.));
#10483=DIRECTION('ref_axis',(0.994365489657067,-0.106006004448152,0.));
#10484=DIRECTION('center_axis',(0.,0.,1.));
#10485=DIRECTION('ref_axis',(-0.994365489657067,0.106006004448152,0.));
#10486=DIRECTION('center_axis',(0.61311568533443,0.789993136930247,0.));
#10487=DIRECTION('ref_axis',(-0.789993136930247,0.61311568533443,0.));
#10488=DIRECTION('',(0.,0.,1.));
#10489=DIRECTION('center_axis',(0.789993136930249,-0.613115685334428,0.));
#10490=DIRECTION('ref_axis',(0.613115685334428,0.789993136930249,0.));
#10491=DIRECTION('',(0.,0.,1.));
#10492=DIRECTION('center_axis',(0.613115685334417,0.789993136930257,0.));
#10493=DIRECTION('ref_axis',(-0.789993136930257,0.613115685334417,0.));
#10494=DIRECTION('',(0.,0.,1.));
#10495=DIRECTION('center_axis',(0.78999313693025,-0.613115685334426,0.));
#10496=DIRECTION('ref_axis',(0.613115685334426,0.78999313693025,0.));
#10497=DIRECTION('',(0.,0.,1.));
#10498=DIRECTION('center_axis',(0.613115685334431,0.789993136930246,0.));
#10499=DIRECTION('ref_axis',(-0.789993136930246,0.613115685334431,0.));
#10500=DIRECTION('',(0.,0.,1.));
#10501=DIRECTION('center_axis',(0.78999313693025,-0.613115685334426,0.));
#10502=DIRECTION('ref_axis',(0.613115685334426,0.78999313693025,0.));
#10503=DIRECTION('',(0.,0.,1.));
#10504=DIRECTION('center_axis',(0.613115685334431,0.789993136930246,0.));
#10505=DIRECTION('ref_axis',(-0.789993136930246,0.613115685334431,0.));
#10506=DIRECTION('',(0.,0.,1.));
#10507=DIRECTION('center_axis',(0.78999313693025,-0.613115685334426,0.));
#10508=DIRECTION('ref_axis',(0.613115685334426,0.78999313693025,0.));
#10509=DIRECTION('',(0.,0.,1.));
#10510=DIRECTION('center_axis',(0.613115685334431,0.789993136930246,0.));
#10511=DIRECTION('ref_axis',(-0.789993136930246,0.613115685334431,0.));
#10512=DIRECTION('',(0.,0.,1.));
#10513=DIRECTION('center_axis',(0.78999313693025,-0.613115685334426,0.));
#10514=DIRECTION('ref_axis',(0.613115685334426,0.78999313693025,0.));
#10515=DIRECTION('',(0.,0.,1.));
#10516=DIRECTION('center_axis',(0.613115685334431,0.789993136930246,0.));
#10517=DIRECTION('ref_axis',(-0.789993136930246,0.613115685334431,0.));
#10518=DIRECTION('',(0.,0.,1.));
#10519=DIRECTION('center_axis',(0.78999313693025,-0.613115685334426,0.));
#10520=DIRECTION('ref_axis',(0.613115685334426,0.78999313693025,0.));
#10521=DIRECTION('',(0.,0.,1.));
#10522=DIRECTION('center_axis',(0.613115685334431,0.789993136930246,0.));
#10523=DIRECTION('ref_axis',(-0.789993136930246,0.613115685334431,0.));
#10524=DIRECTION('',(0.,0.,1.));
#10525=DIRECTION('center_axis',(0.78999313693025,-0.613115685334426,0.));
#10526=DIRECTION('ref_axis',(0.613115685334426,0.78999313693025,0.));
#10527=DIRECTION('',(0.,0.,1.));
#10528=DIRECTION('center_axis',(0.613115685334431,0.789993136930246,0.));
#10529=DIRECTION('ref_axis',(-0.789993136930246,0.613115685334431,0.));
#10530=DIRECTION('',(0.,0.,1.));
#10531=DIRECTION('center_axis',(0.78999313693025,-0.613115685334426,0.));
#10532=DIRECTION('ref_axis',(0.613115685334426,0.78999313693025,0.));
#10533=DIRECTION('',(0.,0.,1.));
#10534=DIRECTION('center_axis',(0.613115685334431,0.789993136930246,0.));
#10535=DIRECTION('ref_axis',(-0.789993136930246,0.613115685334431,0.));
#10536=DIRECTION('',(0.,0.,1.));
#10537=DIRECTION('center_axis',(0.78999313693025,-0.613115685334426,0.));
#10538=DIRECTION('ref_axis',(0.613115685334426,0.78999313693025,0.));
#10539=DIRECTION('',(0.,0.,1.));
#10540=DIRECTION('center_axis',(0.126120657884284,-0.992014908988184,0.));
#10541=DIRECTION('ref_axis',(0.992014908988184,0.126120657884283,0.));
#10542=DIRECTION('center_axis',(-0.125071245462401,0.992147762966023,0.));
#10543=DIRECTION('ref_axis',(-0.992147762966023,-0.125071245462401,0.));
#10544=DIRECTION('center_axis',(0.125071245462382,-0.992147762966025,0.));
#10545=DIRECTION('ref_axis',(0.992147762966025,0.125071245462382,0.));
#10546=DIRECTION('center_axis',(0.921021641733725,0.367194793699938,-0.129950448009129));
#10547=DIRECTION('ref_axis',(-0.148531324297176,0.639504090265382,0.754302965814382));
#10548=DIRECTION('center_axis',(0.,0.,1.));
#10549=DIRECTION('ref_axis',(0.994365489657067,-0.106006004448151,0.));
#10550=DIRECTION('center_axis',(0.125071245462401,-0.992147762966023,0.));
#10551=DIRECTION('ref_axis',(0.992147762966023,0.125071245462401,0.));
#10552=DIRECTION('center_axis',(0.921021641736802,0.367194793701463,0.129950447983017));
#10553=DIRECTION('ref_axis',(0.148622468696408,-0.639675044703561,0.754140039370727));
#10554=DIRECTION('center_axis',(0.125071245462387,-0.992147762966025,-1.19456606278864E-15));
#10555=DIRECTION('ref_axis',(0.992147762966025,0.125071245462387,-5.27799728148075E-30));
#10556=DIRECTION('center_axis',(0.,0.,1.));
#10557=DIRECTION('ref_axis',(0.994365489657067,-0.106006004448151,0.));
#10558=DIRECTION('center_axis',(-0.569403560671587,0.821951347323845,0.0132501972451484));
#10559=DIRECTION('ref_axis',(-0.82202351089107,-0.569453551698748,5.99549716779258E-17));
#10560=DIRECTION('center_axis',(-0.523075905343007,0.67621202355281,0.518776345309043));
#10561=DIRECTION('ref_axis',(-0.79097451855598,-0.61184909168449,-8.0247329727962E-16));
#10562=DIRECTION('center_axis',(-0.569403560671589,0.821951347323843,-0.01325019724517));
#10563=DIRECTION('ref_axis',(-0.822023510891069,-0.56945355169875,-3.009874593151E-17));
#10564=DIRECTION('center_axis',(-0.523075905342989,0.676212023552819,-0.51877634530905));
#10565=DIRECTION('ref_axis',(-0.790974518555994,-0.611849091684473,-1.07459757475795E-15));
#10566=DIRECTION('center_axis',(-0.106006004448152,-0.994365489657067,0.));
#10567=DIRECTION('ref_axis',(0.,0.,-1.));
#10568=DIRECTION('center_axis',(-0.106006004448152,-0.994365489657067,0.));
#10569=DIRECTION('ref_axis',(0.,0.,-1.));
#10570=DIRECTION('center_axis',(-0.106006004448152,-0.994365489657067,0.));
#10571=DIRECTION('ref_axis',(0.,0.,-1.));
#10572=DIRECTION('center_axis',(-0.106006004448152,-0.994365489657067,0.));
#10573=DIRECTION('ref_axis',(0.,0.,-1.));
#10574=DIRECTION('center_axis',(-0.106006004448152,-0.994365489657067,0.));
#10575=DIRECTION('ref_axis',(0.,0.,-1.));
#10576=DIRECTION('center_axis',(-0.106006004448152,-0.994365489657067,0.));
#10577=DIRECTION('ref_axis',(0.,0.,-1.));
#10578=DIRECTION('center_axis',(0.106006004448152,0.994365489657067,0.));
#10579=DIRECTION('ref_axis',(0.,0.,1.));
#10580=DIRECTION('center_axis',(0.,0.,1.));
#10581=DIRECTION('ref_axis',(0.994365489657067,-0.106006004448152,0.));
#10582=DIRECTION('center_axis',(-0.0682742201674528,0.997666593036234,0.));
#10583=DIRECTION('ref_axis',(-0.997666593036234,-0.0682742201674528,0.));
#10584=DIRECTION('center_axis',(0.0682742201674492,-0.997666593036234,0.));
#10585=DIRECTION('ref_axis',(0.997666593036234,0.0682742201674492,0.));
#10586=DIRECTION('center_axis',(-0.0682742201674521,0.997666593036234,0.));
#10587=DIRECTION('ref_axis',(-0.997666593036234,-0.0682742201674521,0.));
#10588=DIRECTION('center_axis',(0.,0.,1.));
#10589=DIRECTION('ref_axis',(-0.778213103173909,0.628000291439769,0.));
#10590=DIRECTION('center_axis',(0.106006004448152,0.994365489657067,0.));
#10591=DIRECTION('ref_axis',(0.,0.,1.));
#10592=DIRECTION('center_axis',(0.106006004448152,0.994365489657067,0.));
#10593=DIRECTION('ref_axis',(0.,0.,1.));
#10594=DIRECTION('center_axis',(0.,0.,1.));
#10595=DIRECTION('ref_axis',(0.994365489657067,-0.106006004448152,0.));
#10596=DIRECTION('center_axis',(-0.0682742201674527,0.997666593036234,0.));
#10597=DIRECTION('ref_axis',(-0.997666593036234,-0.0682742201674527,0.));
#10598=DIRECTION('center_axis',(-0.0682742201674492,0.997666593036234,0.));
#10599=DIRECTION('ref_axis',(-0.997666593036234,-0.0682742201674492,0.));
#10600=DIRECTION('center_axis',(-0.0682742201674527,0.997666593036234,-1.2049262814377E-15));
#10601=DIRECTION('ref_axis',(-0.997666593036234,-0.0682742201674527,-8.5942731427727E-31));
#10602=DIRECTION('center_axis',(0.,0.,1.));
#10603=DIRECTION('ref_axis',(-0.77217793226518,0.635406358893795,0.));
#10604=DIRECTION('center_axis',(0.992147762966023,0.125071245462401,-8.44202479736859E-16));
#10605=DIRECTION('ref_axis',(-0.125071245462401,0.992147762966023,-3.17912585643067E-30));
#10606=DIRECTION('center_axis',(0.992147762966023,0.125071245462402,0.));
#10607=DIRECTION('ref_axis',(-0.125071245462401,0.992147762966023,0.));
#10608=DIRECTION('center_axis',(0.992147762966023,0.125071245462403,1.6155123493858E-12));
#10609=DIRECTION('ref_axis',(-0.125071245462403,0.992147762966023,3.33856974702238E-27));
#10610=DIRECTION('center_axis',(0.,0.,-1.));
#10611=DIRECTION('ref_axis',(-0.994365489657067,0.106006004448149,0.));
#10612=DIRECTION('center_axis',(0.,0.,-1.));
#10613=DIRECTION('ref_axis',(0.712495620570301,0.701676557017649,0.));
#10614=DIRECTION('center_axis',(0.,0.,-1.));
#10615=DIRECTION('ref_axis',(-0.994365489657067,0.106006004448149,0.));
#10616=DIRECTION('center_axis',(-0.992147762966023,-0.125071245462403,3.37680991894744E-15));
#10617=DIRECTION('ref_axis',(0.125071245462403,-0.992147762966023,6.989343426552E-30));
#10618=DIRECTION('center_axis',(-0.992147762966023,-0.125071245462402,0.));
#10619=DIRECTION('ref_axis',(0.125071245462401,-0.992147762966023,0.));
#10620=DIRECTION('center_axis',(-0.992147762966023,-0.125071245462401,0.));
#10621=DIRECTION('ref_axis',(0.125071245462401,-0.992147762966023,0.));
#10622=DIRECTION('center_axis',(0.,0.,1.));
#10623=DIRECTION('ref_axis',(-0.77217793226518,0.635406358893796,0.));
#10624=DIRECTION('center_axis',(0.0682742201674527,-0.997666593036234,0.));
#10625=DIRECTION('ref_axis',(0.997666593036234,0.0682742201674527,0.));
#10626=DIRECTION('center_axis',(0.0682742201674492,-0.997666593036234,0.));
#10627=DIRECTION('ref_axis',(0.997666593036234,0.0682742201674492,0.));
#10628=DIRECTION('center_axis',(0.0682742201674527,-0.997666593036234,0.));
#10629=DIRECTION('ref_axis',(0.997666593036234,0.0682742201674527,0.));
#10630=DIRECTION('center_axis',(0.,0.,1.));
#10631=DIRECTION('ref_axis',(0.994365489657067,-0.106006004448152,0.));
#10632=DIRECTION('center_axis',(-0.106006004448152,-0.994365489657067,0.));
#10633=DIRECTION('ref_axis',(0.,0.,-1.));
#10634=DIRECTION('center_axis',(-0.106006004448152,-0.994365489657067,0.));
#10635=DIRECTION('ref_axis',(0.,0.,-1.));
#10636=DIRECTION('center_axis',(-0.703122551293604,0.0749575614553266,0.707106810774047));
#10637=DIRECTION('ref_axis',(0.708373355339574,-0.012663179875062,0.705724332385107));
#10638=DIRECTION('center_axis',(-0.703122551293603,0.0749575614553284,0.707106810774048));
#10639=DIRECTION('ref_axis',(0.703122610135183,-0.074957567728232,0.707106751599046));
#10640=DIRECTION('center_axis',(0.,0.,-1.));
#10641=DIRECTION('ref_axis',(-0.994365489657067,0.106006004448152,0.));
#10642=DIRECTION('center_axis',(0.,0.,1.));
#10643=DIRECTION('ref_axis',(0.994365489657067,-0.106006004448152,0.));
#10644=DIRECTION('center_axis',(0.,0.,-1.));
#10645=DIRECTION('ref_axis',(0.994365489657067,-0.106006004448153,0.));
#10646=DIRECTION('center_axis',(-0.238110783115727,-0.461122963333811,0.854791710096828));
#10647=DIRECTION('ref_axis',(-0.0922560805895924,-0.865387420522683,-0.492537742711504));
#10648=DIRECTION('center_axis',(-0.524045111191337,-0.851690508011249,-5.23133005782331E-15));
#10649=DIRECTION('ref_axis',(0.851690508011249,-0.524045111191337,-3.3077968467653E-30));
#10650=DIRECTION('center_axis',(0.,0.,1.));
#10651=DIRECTION('ref_axis',(0.994365489657067,-0.106006004448151,0.));
#10652=DIRECTION('center_axis',(-0.822883401708071,-0.56821026670886,-1.64367902233808E-15));
#10653=DIRECTION('ref_axis',(0.56821026670886,-0.822883401708071,-1.45228749875528E-30));
#10654=DIRECTION('center_axis',(0.,0.,1.));
#10655=DIRECTION('ref_axis',(0.994365489657067,-0.106006004448152,0.));
#10656=DIRECTION('center_axis',(-0.190413144371284,-0.981704046263761,0.));
#10657=DIRECTION('ref_axis',(0.981704046263761,-0.190413144371284,0.));
#10658=DIRECTION('center_axis',(0.,0.,1.));
#10659=DIRECTION('ref_axis',(-0.999462558498673,0.0327810030244038,0.));
#10660=DIRECTION('center_axis',(0.,0.,1.));
#10661=DIRECTION('ref_axis',(-0.999462558498673,0.0327810030244038,0.));
#10662=DIRECTION('center_axis',(0.190413144371284,0.981704046263761,0.));
#10663=DIRECTION('ref_axis',(-0.981704046263761,0.190413144371284,0.));
#10664=DIRECTION('center_axis',(0.,0.,1.));
#10665=DIRECTION('ref_axis',(0.994365489657067,-0.106006004448152,0.));
#10666=DIRECTION('center_axis',(0.822883401708071,0.56821026670886,1.64367902233808E-16));
#10667=DIRECTION('ref_axis',(-0.56821026670886,0.822883401708071,7.80923877284138E-31));
#10668=DIRECTION('center_axis',(0.,0.,1.));
#10669=DIRECTION('ref_axis',(0.994365489657067,-0.106006004448151,0.));
#10670=DIRECTION('center_axis',(0.524045111191337,0.851690508011249,-6.72599578862997E-15));
#10671=DIRECTION('ref_axis',(-0.851690508011249,0.524045111191337,-4.14233781763102E-30));
#10672=DIRECTION('center_axis',(0.238110783115725,0.461122963333806,0.854791710096832));
#10673=DIRECTION('ref_axis',(-0.0922560805895938,-0.865387420522686,0.492537742711499));
#10674=DIRECTION('axis',(0.,0.,1.));
#10675=DIRECTION('refdir',(1.,0.,0.));
#10676=DIRECTION('center_axis',(0.106006004448151,0.994365489657067,9.53019194070163E-17));
#10677=DIRECTION('ref_axis',(-0.61063877343479,0.0650981728612347,0.789229064510541));
#10678=DIRECTION('',(-0.106006004448151,-0.994365489657067,-9.53019194070163E-17));
#10679=DIRECTION('center_axis',(0.106006004448151,0.994365489657067,9.53019194070163E-17));
#10680=DIRECTION('ref_axis',(-0.61063877343479,0.0650981728612347,0.789229064510541));
#10681=DIRECTION('center_axis',(0.106006004448151,0.994365489657067,9.53019194070163E-17));
#10682=DIRECTION('ref_axis',(-0.61063877343479,0.0650981728612347,0.789229064510541));
#10683=DIRECTION('',(-0.106006004448151,-0.994365489657067,-9.53019194070163E-17));
#10684=DIRECTION('center_axis',(0.106006004448151,0.994365489657067,9.53019194070163E-17));
#10685=DIRECTION('ref_axis',(-0.61063877343479,0.0650981728612347,0.789229064510541));
#10686=DIRECTION('center_axis',(0.106006004448151,0.994365489657067,9.53019194070163E-17));
#10687=DIRECTION('ref_axis',(-0.61063877343479,0.0650981728612347,0.789229064510541));
#10688=DIRECTION('',(-0.106006004448151,-0.994365489657067,-9.53019194070163E-17));
#10689=DIRECTION('center_axis',(0.106006004448151,0.994365489657067,9.53019194070163E-17));
#10690=DIRECTION('ref_axis',(-0.61063877343479,0.0650981728612347,0.789229064510541));
#10691=DIRECTION('',(-0.106006004448151,-0.994365489657067,-9.53019194070163E-17));
#10692=DIRECTION('center_axis',(0.106006004448151,0.994365489657067,9.53019194070163E-17));
#10693=DIRECTION('ref_axis',(-0.61063877343479,0.0650981728612347,0.789229064510541));
#10694=DIRECTION('',(-0.106006004448151,-0.994365489657067,-9.53019194070163E-17));
#10695=DIRECTION('center_axis',(0.106006004448151,0.994365489657067,9.53019194070163E-17));
#10696=DIRECTION('ref_axis',(-0.61063877343479,0.0650981728612347,0.789229064510541));
#10697=DIRECTION('',(-0.106006004448151,-0.994365489657067,-9.53019194070163E-17));
#10698=DIRECTION('center_axis',(0.106006004448151,0.994365489657067,9.53019194070163E-17));
#10699=DIRECTION('ref_axis',(-0.61063877343479,0.0650981728612347,0.789229064510541));
#10700=DIRECTION('',(-0.106006004448151,-0.994365489657067,-9.53019194070163E-17));
#10701=DIRECTION('center_axis',(0.106006004448151,0.994365489657067,9.53019194070163E-17));
#10702=DIRECTION('ref_axis',(-0.61063877343479,0.0650981728612347,0.789229064510541));
#10703=DIRECTION('',(-0.106006004448151,-0.994365489657067,-9.53019194070163E-17));
#10704=DIRECTION('center_axis',(0.106006004448151,0.994365489657067,9.53019194070163E-17));
#10705=DIRECTION('ref_axis',(-0.61063877343479,0.0650981728612347,0.789229064510541));
#10706=DIRECTION('',(-0.106006004448151,-0.994365489657067,-9.53019194070163E-17));
#10707=DIRECTION('center_axis',(0.106006004448151,0.994365489657067,9.53019194070163E-17));
#10708=DIRECTION('ref_axis',(-0.61063877343479,0.0650981728612347,0.789229064510541));
#10709=DIRECTION('',(-0.106006004448151,-0.994365489657067,-9.53019194070163E-17));
#10710=DIRECTION('center_axis',(0.106006004448151,0.994365489657067,9.53019194070163E-17));
#10711=DIRECTION('ref_axis',(-0.61063877343479,0.0650981728612347,0.789229064510541));
#10712=DIRECTION('',(-0.106006004448151,-0.994365489657067,-9.53019194070163E-17));
#10713=DIRECTION('center_axis',(0.106006004448151,0.994365489657067,9.53019194070163E-17));
#10714=DIRECTION('ref_axis',(-0.61063877343479,0.0650981728612347,0.789229064510541));
#10715=DIRECTION('',(-0.106006004448151,-0.994365489657067,-9.53019194070163E-17));
#10716=DIRECTION('center_axis',(0.106006004448151,0.994365489657067,9.53019194070163E-17));
#10717=DIRECTION('ref_axis',(-0.61063877343479,0.0650981728612347,0.789229064510541));
#10718=DIRECTION('',(-0.106006004448151,-0.994365489657067,-9.53019194070163E-17));
#10719=DIRECTION('center_axis',(0.106006004448151,0.994365489657067,9.53019194070163E-17));
#10720=DIRECTION('ref_axis',(-0.61063877343479,0.0650981728612347,0.789229064510541));
#10721=DIRECTION('',(-0.106006004448151,-0.994365489657067,-9.53019194070163E-17));
#10722=DIRECTION('center_axis',(0.106006004448151,0.994365489657067,9.53019194070163E-17));
#10723=DIRECTION('ref_axis',(-0.61063877343479,0.0650981728612347,0.789229064510541));
#10724=DIRECTION('',(-0.106006004448151,-0.994365489657067,-9.53019194070163E-17));
#10725=DIRECTION('center_axis',(0.106006004448151,0.994365489657067,9.53019194070163E-17));
#10726=DIRECTION('ref_axis',(-0.61063877343479,0.0650981728612347,0.789229064510541));
#10727=DIRECTION('',(-0.106006004448151,-0.994365489657067,-9.53019194070163E-17));
#10728=DIRECTION('center_axis',(0.106006004448151,0.994365489657067,9.53019194070163E-17));
#10729=DIRECTION('ref_axis',(-0.61063877343479,0.0650981728612347,0.789229064510541));
#10730=DIRECTION('',(-0.106006004448151,-0.994365489657067,-9.53019194070163E-17));
#10731=DIRECTION('center_axis',(0.106006004448151,0.994365489657067,9.53019194070163E-17));
#10732=DIRECTION('ref_axis',(-0.61063877343479,0.0650981728612347,0.789229064510541));
#10733=DIRECTION('',(-0.106006004448151,-0.994365489657067,-9.53019194070163E-17));
#10734=DIRECTION('center_axis',(0.106006004448151,0.994365489657067,9.53019194070163E-17));
#10735=DIRECTION('ref_axis',(-0.61063877343479,0.0650981728612347,0.789229064510541));
#10736=DIRECTION('',(-0.106006004448151,-0.994365489657067,-9.53019194070163E-17));
#10737=DIRECTION('center_axis',(0.106006004448151,0.994365489657067,9.53019194070163E-17));
#10738=DIRECTION('ref_axis',(-0.61063877343479,0.0650981728612347,0.789229064510541));
#10739=DIRECTION('',(-0.106006004448151,-0.994365489657067,-9.53019194070163E-17));
#10740=DIRECTION('center_axis',(0.106006004448151,0.994365489657067,9.53019194070163E-17));
#10741=DIRECTION('ref_axis',(-0.61063877343479,0.0650981728612347,0.789229064510541));
#10742=DIRECTION('',(-0.106006004448151,-0.994365489657067,-9.53019194070163E-17));
#10743=DIRECTION('center_axis',(0.106006004448151,0.994365489657067,9.53019194070163E-17));
#10744=DIRECTION('ref_axis',(-0.61063877343479,0.0650981728612347,0.789229064510541));
#10745=DIRECTION('',(-0.106006004448151,-0.994365489657067,-9.53019194070163E-17));
#10746=DIRECTION('center_axis',(0.106006004448151,0.994365489657067,9.53019194070163E-17));
#10747=DIRECTION('ref_axis',(-0.61063877343479,0.0650981728612347,0.789229064510541));
#10748=DIRECTION('',(-0.106006004448151,-0.994365489657067,-9.53019194070163E-17));
#10749=DIRECTION('center_axis',(0.106006004448151,0.994365489657067,9.53019194070163E-17));
#10750=DIRECTION('ref_axis',(-0.61063877343479,0.0650981728612347,0.789229064510541));
#10751=DIRECTION('',(-0.106006004448151,-0.994365489657067,-9.53019194070163E-17));
#10752=DIRECTION('center_axis',(0.106006004448151,0.994365489657067,9.53019194070163E-17));
#10753=DIRECTION('ref_axis',(-0.61063877343479,0.0650981728612347,0.789229064510541));
#10754=DIRECTION('',(-0.106006004448151,-0.994365489657067,-9.53019194070163E-17));
#10755=DIRECTION('center_axis',(0.106006004448151,0.994365489657067,9.53019194070163E-17));
#10756=DIRECTION('ref_axis',(-0.61063877343479,0.0650981728612347,0.789229064510541));
#10757=DIRECTION('',(-0.106006004448151,-0.994365489657067,-9.53019194070163E-17));
#10758=DIRECTION('center_axis',(0.106006004448151,0.994365489657067,9.53019194070163E-17));
#10759=DIRECTION('ref_axis',(-0.61063877343479,0.0650981728612347,0.789229064510541));
#10760=DIRECTION('',(-0.106006004448151,-0.994365489657067,-9.53019194070163E-17));
#10761=DIRECTION('center_axis',(0.106006004448151,0.994365489657067,9.53019194070163E-17));
#10762=DIRECTION('ref_axis',(-0.61063877343479,0.0650981728612347,0.789229064510541));
#10763=DIRECTION('',(-0.106006004448151,-0.994365489657067,-9.53019194070163E-17));
#10764=DIRECTION('center_axis',(0.106006004448151,0.994365489657067,9.53019194070163E-17));
#10765=DIRECTION('ref_axis',(-0.61063877343479,0.0650981728612347,0.789229064510541));
#10766=DIRECTION('',(-0.106006004448151,-0.994365489657067,-9.53019194070163E-17));
#10767=DIRECTION('center_axis',(0.106006004448151,0.994365489657067,9.53019194070163E-17));
#10768=DIRECTION('ref_axis',(-0.61063877343479,0.0650981728612347,0.789229064510541));
#10769=DIRECTION('',(-0.106006004448151,-0.994365489657067,-9.53019194070163E-17));
#10770=DIRECTION('center_axis',(0.106006004448151,0.994365489657067,9.53019194070163E-17));
#10771=DIRECTION('ref_axis',(-0.61063877343479,0.0650981728612347,0.789229064510541));
#10772=DIRECTION('',(-0.106006004448151,-0.994365489657067,-9.53019194070163E-17));
#10773=DIRECTION('center_axis',(0.106006004448151,0.994365489657067,9.53019194070163E-17));
#10774=DIRECTION('ref_axis',(-0.61063877343479,0.0650981728612347,0.789229064510541));
#10775=DIRECTION('',(-0.106006004448151,-0.994365489657067,-9.53019194070163E-17));
#10776=DIRECTION('center_axis',(0.106006004448151,0.994365489657067,9.53019194070163E-17));
#10777=DIRECTION('ref_axis',(-0.61063877343479,0.0650981728612347,0.789229064510541));
#10778=DIRECTION('',(-0.106006004448151,-0.994365489657067,-9.53019194070163E-17));
#10779=DIRECTION('center_axis',(0.106006004448151,0.994365489657067,9.53019194070163E-17));
#10780=DIRECTION('ref_axis',(-0.61063877343479,0.0650981728612347,0.789229064510541));
#10781=DIRECTION('',(-0.106006004448151,-0.994365489657067,-9.53019194070163E-17));
#10782=DIRECTION('center_axis',(0.106006004448151,0.994365489657067,9.53019194070163E-17));
#10783=DIRECTION('ref_axis',(-0.61063877343479,0.0650981728612347,0.789229064510541));
#10784=DIRECTION('',(-0.106006004448151,-0.994365489657067,-9.53019194070163E-17));
#10785=DIRECTION('center_axis',(0.106006004448151,0.994365489657067,9.53019194070163E-17));
#10786=DIRECTION('ref_axis',(-0.61063877343479,0.0650981728612347,0.789229064510541));
#10787=DIRECTION('',(-0.106006004448151,-0.994365489657067,-9.53019194070163E-17));
#10788=DIRECTION('center_axis',(0.106006004448151,0.994365489657067,9.53019194070163E-17));
#10789=DIRECTION('ref_axis',(-0.61063877343479,0.0650981728612347,0.789229064510541));
#10790=DIRECTION('',(-0.106006004448151,-0.994365489657067,-9.53019194070163E-17));
#10791=DIRECTION('center_axis',(0.106006004448151,0.994365489657067,9.53019194070163E-17));
#10792=DIRECTION('ref_axis',(-0.61063877343479,0.0650981728612347,0.789229064510541));
#10793=DIRECTION('',(-0.106006004448151,-0.994365489657067,-9.53019194070163E-17));
#10794=DIRECTION('center_axis',(0.106006004448151,0.994365489657067,9.53019194070163E-17));
#10795=DIRECTION('ref_axis',(-0.61063877343479,0.0650981728612347,0.789229064510541));
#10796=DIRECTION('',(-0.106006004448151,-0.994365489657067,-9.53019194070163E-17));
#10797=DIRECTION('center_axis',(0.106006004448151,0.994365489657067,9.53019194070163E-17));
#10798=DIRECTION('ref_axis',(-0.61063877343479,0.0650981728612347,0.789229064510541));
#10799=DIRECTION('',(-0.106006004448151,-0.994365489657067,-9.53019194070163E-17));
#10800=DIRECTION('center_axis',(0.106006004448151,0.994365489657067,9.53019194070163E-17));
#10801=DIRECTION('ref_axis',(-0.61063877343479,0.0650981728612347,0.789229064510541));
#10802=DIRECTION('',(-0.106006004448151,-0.994365489657067,-9.53019194070163E-17));
#10803=DIRECTION('center_axis',(0.106006004448151,0.994365489657067,9.53019194070163E-17));
#10804=DIRECTION('ref_axis',(-0.610638773434788,0.0650981728612345,0.789229064510543));
#10805=DIRECTION('center_axis',(-0.106006004448151,-0.994365489657067,-9.53019194070163E-17));
#10806=DIRECTION('ref_axis',(-0.61063877343479,0.0650981728612347,0.789229064510541));
#10807=DIRECTION('center_axis',(0.106006004448151,0.994365489657067,9.53019194070163E-17));
#10808=DIRECTION('ref_axis',(-0.61063877343479,0.0650981728612347,0.789229064510541));
#10809=DIRECTION('',(-0.356829252959397,0.749153940187426,0.55806922342492));
#10810=DIRECTION('center_axis',(0.106006004448151,0.994365489657067,9.53019194070163E-17));
#10811=DIRECTION('ref_axis',(-0.61063877343479,0.0650981728612347,0.789229064510541));
#10812=DIRECTION('center_axis',(0.106006004448151,0.994365489657067,9.53019194070163E-17));
#10813=DIRECTION('ref_axis',(-0.610638773434788,0.0650981728612345,0.789229064510543));
#10814=DIRECTION('center_axis',(-0.106006004448151,-0.994365489657067,-9.53019194070163E-17));
#10815=DIRECTION('ref_axis',(0.610638773434775,-0.0650981728612332,-0.789229064510553));
#10816=DIRECTION('',(-0.106006004448151,-0.994365489657067,-9.53019194070163E-17));
#10817=DIRECTION('',(0.106006004448151,0.994365489657067,9.53019194070163E-17));
#10818=DIRECTION('center_axis',(-0.106006004448151,-0.994365489657067,-9.53019194070163E-17));
#10819=DIRECTION('ref_axis',(0.610638773434775,-0.0650981728612332,-0.789229064510553));
#10820=DIRECTION('',(-0.106006004448151,-0.994365489657067,-9.53019194070163E-17));
#10821=DIRECTION('',(0.106006004448151,0.994365489657067,9.53019194070163E-17));
#10822=DIRECTION('center_axis',(-0.106006004448151,-0.994365489657067,-9.53019194070163E-17));
#10823=DIRECTION('ref_axis',(0.610638773434775,-0.0650981728612332,-0.789229064510553));
#10824=DIRECTION('',(-0.106006004448151,-0.994365489657067,-9.53019194070163E-17));
#10825=DIRECTION('',(0.106006004448151,0.994365489657067,9.53019194070163E-17));
#10826=DIRECTION('center_axis',(-0.106006004448151,-0.994365489657067,-9.53019194070163E-17));
#10827=DIRECTION('ref_axis',(0.610638773434775,-0.0650981728612332,-0.789229064510553));
#10828=DIRECTION('',(-0.106006004448151,-0.994365489657067,-9.53019194070163E-17));
#10829=DIRECTION('',(0.106006004448151,0.994365489657067,9.53019194070163E-17));
#10830=DIRECTION('center_axis',(-0.106006004448151,-0.994365489657067,-9.53019194070163E-17));
#10831=DIRECTION('ref_axis',(0.610638773434775,-0.0650981728612332,-0.789229064510553));
#10832=DIRECTION('',(-0.106006004448151,-0.994365489657067,-9.53019194070163E-17));
#10833=DIRECTION('',(0.106006004448151,0.994365489657067,9.53019194070163E-17));
#10834=DIRECTION('center_axis',(-0.106006004448151,-0.994365489657067,-9.53019194070163E-17));
#10835=DIRECTION('ref_axis',(0.610638773434775,-0.0650981728612332,-0.789229064510553));
#10836=DIRECTION('',(-0.106006004448151,-0.994365489657067,-9.53019194070163E-17));
#10837=DIRECTION('',(0.106006004448151,0.994365489657067,9.53019194070163E-17));
#10838=DIRECTION('center_axis',(-0.106006004448151,-0.994365489657067,-9.53019194070163E-17));
#10839=DIRECTION('ref_axis',(0.610638773434775,-0.0650981728612332,-0.789229064510553));
#10840=DIRECTION('',(-0.106006004448151,-0.994365489657067,-9.53019194070163E-17));
#10841=DIRECTION('',(0.106006004448151,0.994365489657067,9.53019194070163E-17));
#10842=DIRECTION('center_axis',(-0.106006004448151,-0.994365489657067,-9.53019194070163E-17));
#10843=DIRECTION('ref_axis',(0.610638773434775,-0.0650981728612332,-0.789229064510553));
#10844=DIRECTION('',(-0.106006004448151,-0.994365489657067,-9.53019194070163E-17));
#10845=DIRECTION('',(0.106006004448151,0.994365489657067,9.53019194070163E-17));
#10846=DIRECTION('center_axis',(-0.106006004448151,-0.994365489657067,-9.53019194070163E-17));
#10847=DIRECTION('ref_axis',(0.610638773434775,-0.0650981728612332,-0.789229064510553));
#10848=DIRECTION('',(-0.106006004448151,-0.994365489657067,-9.53019194070163E-17));
#10849=DIRECTION('',(0.106006004448151,0.994365489657067,9.53019194070163E-17));
#10850=DIRECTION('center_axis',(-0.106006004448151,-0.994365489657067,-9.53019194070163E-17));
#10851=DIRECTION('ref_axis',(0.610638773434775,-0.0650981728612332,-0.789229064510553));
#10852=DIRECTION('',(-0.106006004448151,-0.994365489657067,-9.53019194070163E-17));
#10853=DIRECTION('',(0.106006004448151,0.994365489657067,9.53019194070163E-17));
#10854=DIRECTION('center_axis',(0.106006004448151,0.994365489657067,9.53019194070163E-17));
#10855=DIRECTION('ref_axis',(-0.610638773434788,0.0650981728612347,0.789229064510543));
#10856=DIRECTION('center_axis',(0.106006004448151,0.994365489657067,9.53019194070163E-17));
#10857=DIRECTION('ref_axis',(-0.610638773434787,0.0650981728612345,0.789229064510543));
#10858=DIRECTION('center_axis',(-0.784782145183616,0.0836630197231152,-0.614098920151967));
#10859=DIRECTION('ref_axis',(0.610638773434786,-0.0650981728612341,-0.789229064510544));
#10860=DIRECTION('center_axis',(-0.106006004448151,-0.994365489657067,-9.53019194070163E-17));
#10861=DIRECTION('ref_axis',(-0.610638773434768,0.0650981728612323,0.789229064510559));
#10862=DIRECTION('center_axis',(-0.106006004448151,-0.994365489657067,-9.53019194070163E-17));
#10863=DIRECTION('ref_axis',(-0.610638773434788,0.0650981728612345,0.789229064510543));
#10864=DIRECTION('center_axis',(-0.106006004448151,-0.994365489657067,-9.53019194070163E-17));
#10865=DIRECTION('ref_axis',(-0.610638773434769,0.0650981728612324,0.789229064510558));
#10866=DIRECTION('center_axis',(-0.106006004448151,-0.994365489657067,-9.53019194070163E-17));
#10867=DIRECTION('ref_axis',(-0.610638773434788,0.0650981728612345,0.789229064510543));
#10868=DIRECTION('center_axis',(-0.106006004448151,-0.994365489657067,-9.53019194070163E-17));
#10869=DIRECTION('ref_axis',(-0.61063877343478,0.0650981728612337,0.789229064510549));
#10870=DIRECTION('center_axis',(-0.106006004448151,-0.994365489657067,-9.53019194070163E-17));
#10871=DIRECTION('ref_axis',(-0.610638773434788,0.0650981728612345,0.789229064510543));
#10872=DIRECTION('center_axis',(-0.106006004448151,-0.994365489657067,-9.53019194070163E-17));
#10873=DIRECTION('ref_axis',(-0.610638773434782,0.0650981728612339,0.789229064510547));
#10874=DIRECTION('center_axis',(-0.106006004448151,-0.994365489657067,-9.53019194070163E-17));
#10875=DIRECTION('ref_axis',(-0.610638773434798,0.0650981728612356,0.789229064510535));
#10876=DIRECTION('center_axis',(-0.106006004448151,-0.994365489657067,-9.53019194070163E-17));
#10877=DIRECTION('ref_axis',(-0.610638773434789,0.0650981728612346,0.789229064510542));
#10878=DIRECTION('center_axis',(-0.106006004448151,-0.994365489657067,-9.53019194070163E-17));
#10879=DIRECTION('ref_axis',(-0.610638773434784,0.065098172861234,0.789229064510546));
#10880=DIRECTION('center_axis',(-0.106006004448151,-0.994365489657067,-9.53019194070163E-17));
#10881=DIRECTION('ref_axis',(-0.610638773434788,0.0650981728612345,0.789229064510543));
#10882=DIRECTION('center_axis',(-0.106006004448151,-0.994365489657067,-9.53019194070163E-17));
#10883=DIRECTION('ref_axis',(-0.610638773434788,0.0650981728612345,0.789229064510543));
#10884=DIRECTION('center_axis',(-0.106006004448151,-0.994365489657067,-9.53019194070163E-17));
#10885=DIRECTION('ref_axis',(-0.610638773434786,0.0650981728612343,0.789229064510544));
#10886=DIRECTION('center_axis',(-0.106006004448151,-0.994365489657067,-9.53019194070163E-17));
#10887=DIRECTION('ref_axis',(-0.610638773434773,0.065098172861233,0.789229064510554));
#10888=DIRECTION('center_axis',(-0.106006004448151,-0.994365489657067,-9.53019194070163E-17));
#10889=DIRECTION('ref_axis',(-0.6106387734348,0.0650981728612358,0.789229064510533));
#10890=DIRECTION('center_axis',(-0.106006004448151,-0.994365489657067,-9.53019194070163E-17));
#10891=DIRECTION('ref_axis',(-0.610638773434733,0.0650981728612287,0.789229064510586));
#10892=DIRECTION('center_axis',(-0.106006004448151,-0.994365489657067,-9.53019194070163E-17));
#10893=DIRECTION('ref_axis',(-0.610638773434788,0.0650981728612345,0.789229064510543));
#10894=DIRECTION('center_axis',(-0.106006004448151,-0.994365489657067,-9.53019194070163E-17));
#10895=DIRECTION('ref_axis',(-0.6106387734348,0.0650981728612358,0.789229064510533));
#10896=DIRECTION('center_axis',(-0.106006004448151,-0.994365489657067,-9.53019194070163E-17));
#10897=DIRECTION('ref_axis',(-0.610638773434739,0.0650981728612293,0.789229064510581));
#10898=DIRECTION('center_axis',(-0.106006004448151,-0.994365489657067,-9.53019194070163E-17));
#10899=DIRECTION('ref_axis',(-0.610638773434803,0.0650981728612361,0.789229064510531));
#10900=DIRECTION('center_axis',(-0.106006004448151,-0.994365489657067,-9.53019194070163E-17));
#10901=DIRECTION('ref_axis',(-0.61063877343481,0.0650981728612369,0.789229064510525));
#10902=DIRECTION('center_axis',(-0.106006004448151,-0.994365489657067,-9.53019194070163E-17));
#10903=DIRECTION('ref_axis',(-0.61063877343478,0.0650981728612337,0.789229064510549));
#10904=DIRECTION('center_axis',(-0.106006004448151,-0.994365489657067,-9.53019194070163E-17));
#10905=DIRECTION('ref_axis',(-0.610638773434775,0.0650981728612331,0.789229064510553));
#10906=DIRECTION('center_axis',(-0.106006004448151,-0.994365489657067,-9.53019194070163E-17));
#10907=DIRECTION('ref_axis',(-0.610638773434788,0.0650981728612345,0.789229064510543));
#10908=DIRECTION('center_axis',(-0.106006004448151,-0.994365489657067,-9.53019194070163E-17));
#10909=DIRECTION('ref_axis',(-0.6106387734348,0.0650981728612358,0.789229064510533));
#10910=DIRECTION('center_axis',(-0.106006004448151,-0.994365489657067,-9.53019194070163E-17));
#10911=DIRECTION('ref_axis',(-0.610638773434788,0.0650981728612345,0.789229064510543));
#10912=DIRECTION('center_axis',(-0.106006004448151,-0.994365489657067,-9.53019194070163E-17));
#10913=DIRECTION('ref_axis',(-0.610638773434768,0.0650981728612323,0.789229064510559));
#10914=DIRECTION('center_axis',(-0.106006004448151,-0.994365489657067,-9.53019194070163E-17));
#10915=DIRECTION('ref_axis',(0.610638773434788,-0.0650981728612367,-0.789229064510542));
#10916=DIRECTION('center_axis',(-0.106006004448151,-0.994365489657067,-9.53019194070163E-17));
#10917=DIRECTION('ref_axis',(0.610638773434787,-0.0650981728612345,-0.789229064510543));
#10918=DIRECTION('center_axis',(-0.784782145183614,0.0836630197231149,-0.61409892015197));
#10919=DIRECTION('ref_axis',(-0.61063877343479,0.0650981728612343,0.789229064510542));
#10920=DIRECTION('center_axis',(0.106006004448151,0.994365489657067,9.53019194070163E-17));
#10921=DIRECTION('ref_axis',(0.610638773434869,-0.0650981728612432,-0.789229064510479));
#10922=DIRECTION('center_axis',(0.106006004448151,0.994365489657067,9.53019194070163E-17));
#10923=DIRECTION('ref_axis',(0.610638773434769,-0.0650981728612324,-0.789229064510558));
#10924=DIRECTION('center_axis',(0.106006004448151,0.994365489657067,9.53019194070163E-17));
#10925=DIRECTION('ref_axis',(0.610638773434814,-0.0650981728612372,-0.789229064510522));
#10926=DIRECTION('center_axis',(0.106006004448151,0.994365489657067,9.53019194070163E-17));
#10927=DIRECTION('ref_axis',(0.610638773434779,-0.0650981728612335,-0.78922906451055));
#10928=DIRECTION('center_axis',(0.106006004448151,0.994365489657067,9.53019194070163E-17));
#10929=DIRECTION('ref_axis',(0.610638773434794,-0.0650981728612351,-0.789229064510538));
#10930=DIRECTION('center_axis',(0.106006004448151,0.994365489657067,9.53019194070163E-17));
#10931=DIRECTION('ref_axis',(0.6106387734348,-0.0650981728612357,-0.789229064510534));
#10932=DIRECTION('center_axis',(0.106006004448151,0.994365489657067,9.53019194070163E-17));
#10933=DIRECTION('ref_axis',(0.610638773434788,-0.0650981728612346,-0.789229064510543));
#10934=DIRECTION('center_axis',(0.106006004448151,0.994365489657067,9.53019194070163E-17));
#10935=DIRECTION('ref_axis',(0.610638773434794,-0.0650981728612351,-0.789229064510538));
#10936=DIRECTION('center_axis',(0.106006004448151,0.994365489657067,9.53019194070163E-17));
#10937=DIRECTION('ref_axis',(0.610638773434789,-0.0650981728612346,-0.789229064510542));
#10938=DIRECTION('center_axis',(0.106006004448151,0.994365489657067,9.53019194070163E-17));
#10939=DIRECTION('ref_axis',(0.610638773434785,-0.0650981728612342,-0.789229064510545));
#10940=DIRECTION('center_axis',(0.106006004448151,0.994365489657067,9.53019194070163E-17));
#10941=DIRECTION('ref_axis',(0.610638773434789,-0.0650981728612346,-0.789229064510542));
#10942=DIRECTION('center_axis',(0.106006004448151,0.994365489657067,9.53019194070163E-17));
#10943=DIRECTION('ref_axis',(0.610638773434789,-0.0650981728612346,-0.789229064510542));
#10944=DIRECTION('center_axis',(0.106006004448151,0.994365489657067,9.53019194070163E-17));
#10945=DIRECTION('ref_axis',(0.610638773434788,-0.0650981728612345,-0.789229064510543));
#10946=DIRECTION('center_axis',(0.106006004448151,0.994365489657067,9.53019194070163E-17));
#10947=DIRECTION('ref_axis',(0.610638773434677,-0.0650981728612226,-0.78922906451063));
#10948=DIRECTION('center_axis',(0.106006004448151,0.994365489657067,9.53019194070163E-17));
#10949=DIRECTION('ref_axis',(0.610638773434818,-0.0650981728612377,-0.789229064510519));
#10950=DIRECTION('center_axis',(0.106006004448151,0.994365489657067,9.53019194070163E-17));
#10951=DIRECTION('ref_axis',(0.610638773434805,-0.0650981728612363,-0.789229064510529));
#10952=DIRECTION('center_axis',(0.106006004448151,0.994365489657067,9.53019194070163E-17));
#10953=DIRECTION('ref_axis',(0.610638773434784,-0.065098172861234,-0.789229064510546));
#10954=DIRECTION('center_axis',(0.106006004448151,0.994365489657067,9.53019194070163E-17));
#10955=DIRECTION('ref_axis',(0.610638773434769,-0.0650981728612325,-0.789229064510557));
#10956=DIRECTION('center_axis',(0.106006004448151,0.994365489657067,9.53019194070163E-17));
#10957=DIRECTION('ref_axis',(0.610638773434788,-0.0650981728612346,-0.789229064510543));
#10958=DIRECTION('center_axis',(0.106006004448151,0.994365489657067,9.53019194070163E-17));
#10959=DIRECTION('ref_axis',(0.610638773434803,-0.0650981728612361,-0.789229064510531));
#10960=DIRECTION('center_axis',(0.106006004448151,0.994365489657067,9.53019194070163E-17));
#10961=DIRECTION('ref_axis',(0.610638773434803,-0.0650981728612361,-0.789229064510531));
#10962=DIRECTION('center_axis',(0.106006004448151,0.994365489657067,9.53019194070163E-17));
#10963=DIRECTION('ref_axis',(0.610638773434838,-0.0650981728612399,-0.789229064510503));
#10964=DIRECTION('center_axis',(0.106006004448151,0.994365489657067,9.53019194070163E-17));
#10965=DIRECTION('ref_axis',(0.610638773434801,-0.0650981728612359,-0.789229064510533));
#10966=DIRECTION('center_axis',(0.106006004448151,0.994365489657067,9.53019194070163E-17));
#10967=DIRECTION('ref_axis',(0.610638773434788,-0.0650981728612346,-0.789229064510543));
#10968=DIRECTION('center_axis',(0.106006004448151,0.994365489657067,9.53019194070163E-17));
#10969=DIRECTION('ref_axis',(0.610638773434777,-0.0650981728612333,-0.789229064510551));
#10970=DIRECTION('center_axis',(0.106006004448151,0.994365489657067,9.53019194070163E-17));
#10971=DIRECTION('ref_axis',(0.610638773434788,-0.0650981728612346,-0.789229064510543));
#10972=DIRECTION('center_axis',(0.106006004448151,0.994365489657067,9.53019194070163E-17));
#10973=DIRECTION('ref_axis',(0.610638773434869,-0.0650981728612432,-0.789229064510479));
#10974=DIRECTION('center_axis',(0.106006004448151,0.994365489657067,9.53019194070163E-17));
#10975=DIRECTION('ref_axis',(-0.61063877343479,0.0650981728612347,0.789229064510541));
#10976=DIRECTION('center_axis',(0.106006004448151,0.994365489657067,9.53019194070163E-17));
#10977=DIRECTION('ref_axis',(-0.610638773434788,0.0650981728612345,0.789229064510543));
#10978=DIRECTION('center_axis',(0.106006004448151,0.994365489657067,9.53019194070163E-17));
#10979=DIRECTION('ref_axis',(-0.610638773434788,0.0650981728612345,0.789229064510543));
#10980=DIRECTION('',(0.106006004448151,0.994365489657067,9.53019194070163E-17));
#10981=DIRECTION('center_axis',(0.106006004448151,0.994365489657067,9.53019194070163E-17));
#10982=DIRECTION('ref_axis',(-0.610638773434788,0.0650981728612345,0.789229064510543));
#10983=DIRECTION('center_axis',(0.106006004448151,0.994365489657067,9.53019194070163E-17));
#10984=DIRECTION('ref_axis',(-0.610638773434788,0.0650981728612345,0.789229064510543));
#10985=DIRECTION('center_axis',(0.106006004448151,0.994365489657067,9.53019194070163E-17));
#10986=DIRECTION('ref_axis',(-0.610638773434788,0.0650981728612345,0.789229064510543));
#10987=DIRECTION('center_axis',(0.106006004448151,0.994365489657067,9.53019194070163E-17));
#10988=DIRECTION('ref_axis',(-0.610638773434788,0.0650981728612345,0.789229064510543));
#10989=DIRECTION('center_axis',(0.106006004448151,0.994365489657067,9.53019194070163E-17));
#10990=DIRECTION('ref_axis',(-0.610638773434788,0.0650981728612345,0.789229064510543));
#10991=DIRECTION('center_axis',(0.106006004448151,0.994365489657067,9.53019194070163E-17));
#10992=DIRECTION('ref_axis',(-0.610638773434788,0.0650981728612345,0.789229064510543));
#10993=DIRECTION('center_axis',(0.106006004448151,0.994365489657067,9.53019194070163E-17));
#10994=DIRECTION('ref_axis',(-0.610638773434788,0.0650981728612345,0.789229064510543));
#10995=DIRECTION('center_axis',(0.106006004448151,0.994365489657067,9.53019194070163E-17));
#10996=DIRECTION('ref_axis',(-0.610638773434788,0.0650981728612345,0.789229064510543));
#10997=DIRECTION('center_axis',(0.106006004448151,0.994365489657067,9.53019194070163E-17));
#10998=DIRECTION('ref_axis',(-0.610638773434788,0.0650981728612345,0.789229064510543));
#10999=DIRECTION('',(-0.106006004448151,-0.994365489657067,-9.53019194070163E-17));
#11000=DIRECTION('center_axis',(0.106006004448151,0.994365489657067,9.53019194070163E-17));
#11001=DIRECTION('ref_axis',(-0.610638773434788,0.0650981728612345,0.789229064510543));
#11002=DIRECTION('',(0.106006004448151,0.994365489657067,9.53019194070163E-17));
#11003=DIRECTION('',(-0.106006004448151,-0.994365489657067,-9.53019194070163E-17));
#11004=DIRECTION('center_axis',(0.106006004448151,0.994365489657067,9.53019194070163E-17));
#11005=DIRECTION('ref_axis',(-0.610638773434788,0.0650981728612345,0.789229064510543));
#11006=DIRECTION('',(0.106006004448151,0.994365489657067,9.53019194070163E-17));
#11007=DIRECTION('',(-0.106006004448151,-0.994365489657067,-9.53019194070163E-17));
#11008=DIRECTION('center_axis',(0.106006004448151,0.994365489657067,9.53019194070163E-17));
#11009=DIRECTION('ref_axis',(-0.610638773434788,0.0650981728612345,0.789229064510543));
#11010=DIRECTION('',(0.106006004448151,0.994365489657067,9.53019194070163E-17));
#11011=DIRECTION('',(-0.106006004448151,-0.994365489657067,-9.53019194070163E-17));
#11012=DIRECTION('center_axis',(0.106006004448151,0.994365489657067,9.53019194070163E-17));
#11013=DIRECTION('ref_axis',(-0.610638773434788,0.0650981728612345,0.789229064510543));
#11014=DIRECTION('',(0.106006004448151,0.994365489657067,9.53019194070163E-17));
#11015=DIRECTION('',(-0.106006004448151,-0.994365489657067,-9.53019194070163E-17));
#11016=DIRECTION('center_axis',(0.106006004448151,0.994365489657067,9.53019194070163E-17));
#11017=DIRECTION('ref_axis',(-0.610638773434788,0.0650981728612345,0.789229064510543));
#11018=DIRECTION('',(0.106006004448151,0.994365489657067,9.53019194070163E-17));
#11019=DIRECTION('',(-0.106006004448151,-0.994365489657067,-9.53019194070163E-17));
#11020=DIRECTION('center_axis',(0.106006004448151,0.994365489657067,9.53019194070163E-17));
#11021=DIRECTION('ref_axis',(-0.610638773434788,0.0650981728612345,0.789229064510543));
#11022=DIRECTION('',(0.106006004448151,0.994365489657067,9.53019194070163E-17));
#11023=DIRECTION('',(-0.106006004448151,-0.994365489657067,-9.53019194070163E-17));
#11024=DIRECTION('center_axis',(0.106006004448151,0.994365489657067,9.53019194070163E-17));
#11025=DIRECTION('ref_axis',(-0.610638773434788,0.0650981728612345,0.789229064510543));
#11026=DIRECTION('',(0.106006004448151,0.994365489657067,9.53019194070163E-17));
#11027=DIRECTION('',(-0.106006004448151,-0.994365489657067,-9.53019194070163E-17));
#11028=DIRECTION('center_axis',(0.106006004448151,0.994365489657067,9.53019194070163E-17));
#11029=DIRECTION('ref_axis',(0.61063877343478,-0.0650981728612336,-0.789229064510549));
#11030=DIRECTION('',(0.106006004448151,0.994365489657067,9.53019194070163E-17));
#11031=DIRECTION('',(-0.106006004448151,-0.994365489657067,-9.53019194070163E-17));
#11032=DIRECTION('center_axis',(0.106006004448151,0.994365489657067,9.53019194070163E-17));
#11033=DIRECTION('ref_axis',(-0.610638773434788,0.0650981728612345,0.789229064510543));
#11034=DIRECTION('',(0.106006004448151,0.994365489657067,9.53019194070163E-17));
#11035=DIRECTION('',(-0.106006004448151,-0.994365489657067,-9.53019194070163E-17));
#11036=DIRECTION('center_axis',(0.106006004448151,0.994365489657067,9.53019194070163E-17));
#11037=DIRECTION('ref_axis',(-0.610638773434788,0.0650981728612345,0.789229064510543));
#11038=DIRECTION('',(0.106006004448151,0.994365489657067,9.53019194070163E-17));
#11039=DIRECTION('',(-0.106006004448151,-0.994365489657067,-9.53019194070163E-17));
#11040=DIRECTION('center_axis',(0.106006004448151,0.994365489657067,9.53019194070163E-17));
#11041=DIRECTION('ref_axis',(-0.610638773434788,0.0650981728612345,0.789229064510543));
#11042=DIRECTION('',(0.106006004448151,0.994365489657067,9.53019194070163E-17));
#11043=DIRECTION('',(-0.106006004448151,-0.994365489657067,-9.53019194070163E-17));
#11044=DIRECTION('center_axis',(0.106006004448151,0.994365489657067,9.53019194070163E-17));
#11045=DIRECTION('ref_axis',(-0.610638773434788,0.0650981728612345,0.789229064510543));
#11046=DIRECTION('',(0.106006004448151,0.994365489657067,9.53019194070163E-17));
#11047=DIRECTION('',(-0.106006004448151,-0.994365489657067,-9.53019194070163E-17));
#11048=DIRECTION('center_axis',(0.106006004448151,0.994365489657067,9.53019194070163E-17));
#11049=DIRECTION('ref_axis',(-0.610638773434788,0.0650981728612345,0.789229064510543));
#11050=DIRECTION('',(0.106006004448151,0.994365489657067,9.53019194070163E-17));
#11051=DIRECTION('',(-0.106006004448151,-0.994365489657067,-9.53019194070163E-17));
#11052=DIRECTION('center_axis',(0.106006004448151,0.994365489657067,9.53019194070163E-17));
#11053=DIRECTION('ref_axis',(-0.610638773434788,0.0650981728612345,0.789229064510543));
#11054=DIRECTION('',(0.106006004448151,0.994365489657067,9.53019194070163E-17));
#11055=DIRECTION('',(-0.106006004448151,-0.994365489657067,-9.53019194070163E-17));
#11056=DIRECTION('center_axis',(0.106006004448151,0.994365489657067,8.32667268468867E-17));
#11057=DIRECTION('ref_axis',(-0.610638773434788,0.0650981728612344,0.789229064510543));
#11058=DIRECTION('center_axis',(-0.106006004448151,-0.994365489657067,-8.32667268468867E-17));
#11059=DIRECTION('ref_axis',(0.610638773434788,-0.0650981728612344,-0.789229064510543));
#11060=DIRECTION('center_axis',(0.106006004448151,0.994365489657067,9.53019194070163E-17));
#11061=DIRECTION('ref_axis',(-0.610638773434788,0.0650981728612345,0.789229064510543));
#11062=DIRECTION('',(-0.106006004448151,-0.994365489657067,-9.53019194070163E-17));
#11063=DIRECTION('',(0.106006004448151,0.994365489657067,9.53019194070163E-17));
#11064=DIRECTION('center_axis',(0.106006004448151,0.994365489657067,8.32667268468867E-17));
#11065=DIRECTION('ref_axis',(-0.610638773434788,0.0650981728612344,0.789229064510543));
#11066=DIRECTION('center_axis',(-0.106006004448151,-0.994365489657067,-9.53019194070163E-17));
#11067=DIRECTION('ref_axis',(0.610638773434775,-0.0650981728612332,-0.789229064510553));
#11068=DIRECTION('center_axis',(-0.106006004448151,-0.994365489657067,-9.53019194070163E-17));
#11069=DIRECTION('ref_axis',(0.610638773434775,-0.0650981728612332,-0.789229064510553));
#11070=DIRECTION('center_axis',(-0.106006004448151,-0.994365489657067,-9.53019194070163E-17));
#11071=DIRECTION('ref_axis',(0.411112091514325,-0.0438272955518462,0.910530623524178));
#11072=DIRECTION('center_axis',(-0.106006004448151,-0.994365489657067,-9.53019194070163E-17));
#11073=DIRECTION('ref_axis',(0.182489463977752,-0.0194545960528438,0.983015317393139));
#11074=DIRECTION('center_axis',(-0.106006004448151,-0.994365489657067,-9.53019194070163E-17));
#11075=DIRECTION('ref_axis',(-0.0567387878830537,0.00604873385417662,0.998370734130525));
#11076=DIRECTION('center_axis',(-0.106006004448151,-0.994365489657067,-9.53019194070163E-17));
#11077=DIRECTION('ref_axis',(-0.292669587629176,0.0312005333358429,0.955704472730209));
#11078=DIRECTION('center_axis',(-0.106006004448151,-0.994365489657067,-9.53019194070163E-17));
#11079=DIRECTION('ref_axis',(-0.511591494752952,0.0545390712293536,0.857496141219236));
#11080=DIRECTION('center_axis',(-0.106006004448151,-0.994365489657067,-9.53019194070163E-17));
#11081=DIRECTION('ref_axis',(-0.700781563761136,0.0747079965444751,0.709453250852237));
#11082=DIRECTION('center_axis',(-0.106006004448151,-0.994365489657067,-9.53019194070163E-17));
#11083=DIRECTION('ref_axis',(-0.849244755520856,0.0905351646529493,0.520179516303349));
#11084=DIRECTION('center_axis',(-0.106006004448151,-0.994365489657067,-9.53019194070163E-17));
#11085=DIRECTION('ref_axis',(-0.948352928968786,0.101100758073727,0.300674839042517));
#11086=DIRECTION('center_axis',(-0.106006004448151,-0.994365489657067,-9.53019194070163E-17));
#11087=DIRECTION('ref_axis',(-0.992346277307685,0.105790742921563,0.0636960330451088));
#11088=DIRECTION('center_axis',(-0.106006004448151,-0.994365489657067,-9.53019194070163E-17));
#11089=DIRECTION('ref_axis',(-0.978668067041421,0.104332554324503,-0.176984554867181));
#11090=DIRECTION('center_axis',(-0.106006004448151,-0.994365489657067,-9.53019194070163E-17));
#11091=DIRECTION('ref_axis',(0.610638773434775,-0.0650981728612332,-0.789229064510553));
#11092=DIRECTION('center_axis',(-0.106006004448151,-0.994365489657067,-9.53019194070163E-17));
#11093=DIRECTION('ref_axis',(0.610638773434775,-0.0650981728612332,-0.789229064510553));
#11094=DIRECTION('center_axis',(-0.106006004448151,-0.994365489657067,-9.53019194070163E-17));
#11095=DIRECTION('ref_axis',(0.610638773434775,-0.0650981728612332,-0.789229064510553));
#11096=DIRECTION('center_axis',(-0.106006004448151,-0.994365489657067,-9.53019194070163E-17));
#11097=DIRECTION('ref_axis',(0.610638773434775,-0.0650981728612332,-0.789229064510553));
#11098=DIRECTION('center_axis',(0.106006004448151,0.994365489657067,8.32667268468867E-17));
#11099=DIRECTION('ref_axis',(-0.610638773434788,0.0650981728612344,0.789229064510543));
#11100=DIRECTION('axis',(0.,0.,1.));
#11101=DIRECTION('refdir',(1.,0.,0.));
#11102=DIRECTION('center_axis',(0.106006004448152,0.994365489657067,0.));
#11103=DIRECTION('ref_axis',(0.,0.,1.));
#11104=DIRECTION('center_axis',(0.,0.,-1.));
#11105=DIRECTION('ref_axis',(-0.994365489657067,0.106006004448153,0.));
#11106=DIRECTION('',(0.,0.,1.));
#11107=DIRECTION('center_axis',(0.106006004448152,0.994365489657067,0.));
#11108=DIRECTION('ref_axis',(1.21774651409112E-16,-1.29819914037829E-17,
-1.));
#11109=DIRECTION('axis',(0.,0.,1.));
#11110=DIRECTION('refdir',(1.,0.,0.));
#11111=DIRECTION('center_axis',(-2.46563637061793E-17,-5.67162995353388E-17,
-1.));
#11112=DIRECTION('ref_axis',(-0.99065493718706,0.136392065117079,0.));
#11113=DIRECTION('center_axis',(2.46563637061793E-17,5.67162995353388E-17,
1.));
#11114=DIRECTION('ref_axis',(-0.99065493718706,0.136392065117079,1.66902952191827E-17));
#11115=DIRECTION('center_axis',(0.813167683561177,0.582029482424859,1.13956207311045E-15));
#11116=DIRECTION('ref_axis',(-0.582029482424859,0.813167683561177,2.73196138259506E-30));
#11117=DIRECTION('center_axis',(-2.46563637061793E-17,-5.67162995353388E-17,
-1.));
#11118=DIRECTION('ref_axis',(-0.99065493718706,0.136392065117079,1.66902952191827E-17));
#11119=DIRECTION('center_axis',(-0.916721549040254,-0.399526721916366,4.52626971630092E-17));
#11120=DIRECTION('ref_axis',(0.399526721916366,-0.916721549040254,2.21817733744602E-31));
#11121=DIRECTION('center_axis',(-2.46563637061793E-17,-5.67162995353388E-17,
-1.));
#11122=DIRECTION('ref_axis',(-0.99065493718706,0.136392065117079,0.));
#11123=DIRECTION('center_axis',(2.46563637061793E-17,5.67162995353388E-17,
1.));
#11124=DIRECTION('ref_axis',(-0.99065493718706,0.136392065117079,1.66902952191827E-17));
#11125=DIRECTION('center_axis',(0.813167683561178,0.582029482424858,-5.30603166236022E-17));
#11126=DIRECTION('ref_axis',(-0.582029482424858,0.813167683561178,-1.88716532676391E-31));
#11127=DIRECTION('center_axis',(-2.46563637061793E-17,-5.67162995353388E-17,
-1.));
#11128=DIRECTION('ref_axis',(-0.99065493718706,0.136392065117079,1.66902952191827E-17));
#11129=DIRECTION('center_axis',(-0.916721549040254,-0.399526721916366,4.52626971630092E-17));
#11130=DIRECTION('ref_axis',(0.399526721916366,-0.916721549040254,2.43484877201396E-31));
#11131=DIRECTION('center_axis',(-2.46563637061793E-17,-5.67162995353388E-17,
-1.));
#11132=DIRECTION('ref_axis',(-0.99065493718706,0.136392065117078,1.66902952191827E-17));
#11133=DIRECTION('center_axis',(2.46563637061793E-17,5.67162995353388E-17,
1.));
#11134=DIRECTION('ref_axis',(0.99065493718706,-0.136392065117078,-1.66902952191827E-17));
#11135=DIRECTION('',(-2.46563637061793E-17,-5.67162995353388E-17,-1.));
#11136=DIRECTION('center_axis',(2.46563637061793E-17,5.67162995353388E-17,
1.));
#11137=DIRECTION('ref_axis',(0.99065493718706,-0.136392065117078,-1.66902952191827E-17));
#11138=DIRECTION('center_axis',(2.46563637061793E-17,5.67162995353388E-17,
1.));
#11139=DIRECTION('ref_axis',(0.99065493718706,-0.136392065117079,-1.66902952191827E-17));
#11140=DIRECTION('center_axis',(-2.46563637061793E-17,-5.67162995353388E-17,
-1.));
#11141=DIRECTION('ref_axis',(-0.99065493718706,0.136392065117079,1.66902952191827E-17));
#11142=DIRECTION('',(2.46563637061793E-17,5.67162995353388E-17,1.));
#11143=DIRECTION('center_axis',(2.46563637061793E-17,5.67162995353388E-17,
1.));
#11144=DIRECTION('ref_axis',(0.99065493718706,-0.136392065117079,-1.66902952191827E-17));
#11145=DIRECTION('center_axis',(2.46563637061793E-17,5.67162995353388E-17,
1.));
#11146=DIRECTION('ref_axis',(0.99065493718706,-0.136392065117079,-1.66902952191827E-17));
#11147=DIRECTION('center_axis',(-2.46563637061793E-17,-5.67162995353388E-17,
-1.));
#11148=DIRECTION('ref_axis',(-0.99065493718706,0.136392065117079,1.66902952191827E-17));
#11149=DIRECTION('',(2.46563637061793E-17,5.67162995353388E-17,1.));
#11150=DIRECTION('center_axis',(2.46563637061793E-17,5.67162995353388E-17,
1.));
#11151=DIRECTION('ref_axis',(0.99065493718706,-0.136392065117079,-1.66902952191827E-17));
#11152=DIRECTION('center_axis',(-2.46563637061793E-17,-5.67162995353388E-17,
-1.));
#11153=DIRECTION('ref_axis',(-0.99065493718706,0.136392065117079,0.));
#11154=DIRECTION('center_axis',(-2.46563637061793E-17,-5.67162995353388E-17,
-1.));
#11155=DIRECTION('ref_axis',(-0.99065493718706,0.136392065117079,1.66902952191827E-17));
#11156=DIRECTION('center_axis',(-0.089158316805357,-0.996017466987621,9.09675535379384E-13));
#11157=DIRECTION('ref_axis',(0.996017466987621,-0.089158316805357,-1.17238054377005E-27));
#11158=DIRECTION('center_axis',(2.46563637061793E-17,5.67162995353388E-17,
1.));
#11159=DIRECTION('ref_axis',(-0.990654937187062,0.136392065117066,1.66902952191835E-17));
#11160=DIRECTION('center_axis',(-2.46563637061793E-17,-5.67162995353388E-17,
-1.));
#11161=DIRECTION('ref_axis',(-0.99065493718706,0.136392065117079,0.));
#11162=DIRECTION('center_axis',(-2.46563637061793E-17,-5.67162995353388E-17,
-1.));
#11163=DIRECTION('ref_axis',(-0.99065493718706,0.136392065117079,1.66902952191827E-17));
#11164=DIRECTION('center_axis',(-0.0891583168058793,-0.996017466987574,
5.86887448866932E-17));
#11165=DIRECTION('ref_axis',(0.996017466987574,-0.0891583168058793,2.42436373273487E-32));
#11166=DIRECTION('center_axis',(2.46563637061793E-17,5.67162995353388E-17,
1.));
#11167=DIRECTION('ref_axis',(-0.990654937187062,0.136392065117067,1.66902952191834E-17));
#11168=DIRECTION('center_axis',(-2.46563637061793E-17,-5.67162995353388E-17,
-1.));
#11169=DIRECTION('ref_axis',(-0.99065493718706,0.136392065117079,1.66902952191827E-17));
#11170=DIRECTION('center_axis',(-2.46563637061793E-17,-5.67162995353388E-17,
-1.));
#11171=DIRECTION('ref_axis',(0.99065493718706,-0.136392065117079,-1.66902952191827E-17));
#11172=DIRECTION('',(-2.46563637061793E-17,-5.67162995353388E-17,-1.));
#11173=DIRECTION('center_axis',(-2.46563637061793E-17,-5.67162995353388E-17,
-1.));
#11174=DIRECTION('ref_axis',(0.99065493718706,-0.136392065117079,-1.66902952191827E-17));
#11175=DIRECTION('',(-2.46563637061793E-17,-5.67162995353388E-17,-1.));
#11176=DIRECTION('center_axis',(-2.46563637061793E-17,-5.67162995353388E-17,
-1.));
#11177=DIRECTION('ref_axis',(-0.99065493718706,0.136392065117079,1.66902952191827E-17));
#11178=DIRECTION('',(-2.46563637061793E-17,-5.67162995353388E-17,-1.));
#11179=DIRECTION('',(-2.46563637061793E-17,-5.67162995353388E-17,-1.));
#11180=DIRECTION('center_axis',(-2.46563637061793E-17,-5.67162995353388E-17,
-1.));
#11181=DIRECTION('ref_axis',(-0.99065493718706,0.136392065117079,1.66902952191827E-17));
#11182=DIRECTION('center_axis',(-2.46563637061793E-17,-5.67162995353388E-17,
-1.));
#11183=DIRECTION('ref_axis',(0.99065493718706,-0.136392065117079,-1.66902952191827E-17));
#11184=DIRECTION('',(2.46563637061793E-17,5.67162995353388E-17,1.));
#11185=DIRECTION('center_axis',(-2.46563637061793E-17,-5.67162995353388E-17,
-1.));
#11186=DIRECTION('ref_axis',(0.99065493718706,-0.136392065117079,-1.66902952191827E-17));
#11187=DIRECTION('',(-2.46563637061793E-17,-5.67162995353388E-17,-1.));
#11188=DIRECTION('center_axis',(-2.46563637061793E-17,-5.67162995353388E-17,
-1.));
#11189=DIRECTION('ref_axis',(-0.99065493718706,0.136392065117079,1.66902952191827E-17));
#11190=DIRECTION('center_axis',(-2.46563637061793E-17,-5.67162995353388E-17,
-1.));
#11191=DIRECTION('ref_axis',(0.99065493718706,-0.136392065117079,-1.66902952191827E-17));
#11192=DIRECTION('center_axis',(0.272924859769355,-0.826517122498203,0.492322523491631));
#11193=DIRECTION('ref_axis',(-0.96059955766106,-0.262077780098513,0.0925404073905592));
#11194=DIRECTION('center_axis',(2.46563637061793E-17,5.67162995353388E-17,
1.));
#11195=DIRECTION('ref_axis',(-0.99065493718706,0.136392065117079,1.66902952191827E-17));
#11196=DIRECTION('',(-2.46563637061793E-17,-5.67162995353388E-17,-1.));
#11197=DIRECTION('center_axis',(-2.46563637061793E-17,-5.67162995353388E-17,
-1.));
#11198=DIRECTION('ref_axis',(-0.99065493718706,0.136392065117079,1.66902952191827E-17));
#11199=DIRECTION('center_axis',(0.272924859943062,-0.826517122450901,-0.492322523474746));
#11200=DIRECTION('ref_axis',(-0.960787153734946,-0.26023504479525,-0.0957380106243915));
#11201=DIRECTION('center_axis',(-2.46563637061793E-17,-5.67162995353388E-17,
-1.));
#11202=DIRECTION('ref_axis',(0.99065493718706,-0.136392065117079,-1.66902952191827E-17));
#11203=DIRECTION('',(2.46563637061793E-17,5.67162995353388E-17,1.));
#11204=DIRECTION('center_axis',(-2.46563637061793E-17,-5.67162995353388E-17,
-1.));
#11205=DIRECTION('ref_axis',(-0.99065493718706,0.136392065117079,1.66902952191827E-17));
#11206=DIRECTION('center_axis',(-2.46563637061793E-17,-5.67162995353388E-17,
-1.));
#11207=DIRECTION('ref_axis',(0.990654937187061,-0.136392065117078,-1.66902952191827E-17));
#11208=DIRECTION('',(2.46563637061793E-17,5.67162995353388E-17,1.));
#11209=DIRECTION('center_axis',(-2.46563637061793E-17,-5.67162995353388E-17,
-1.));
#11210=DIRECTION('ref_axis',(0.990654937187061,-0.136392065117078,-1.66902952191827E-17));
#11211=DIRECTION('',(-2.46563637061793E-17,-5.67162995353388E-17,-1.));
#11212=DIRECTION('center_axis',(-2.46563637061793E-17,-5.67162995353388E-17,
-1.));
#11213=DIRECTION('ref_axis',(-0.99065493718706,0.136392065117079,1.66902952191827E-17));
#11214=DIRECTION('',(2.46563637061793E-17,5.67162995353388E-17,1.));
#11215=DIRECTION('center_axis',(-2.46563637061793E-17,-5.67162995353388E-17,
-1.));
#11216=DIRECTION('ref_axis',(-0.99065493718706,0.136392065117079,1.66902952191827E-17));
#11217=DIRECTION('',(-2.46563637061793E-17,-5.67162995353388E-17,-1.));
#11218=DIRECTION('center_axis',(-2.46563637061793E-17,-5.67162995353388E-17,
-1.));
#11219=DIRECTION('ref_axis',(0.990654937187061,-0.136392065117077,-1.66902952191828E-17));
#11220=DIRECTION('center_axis',(-2.46563637061793E-17,-5.67162995353388E-17,
-1.));
#11221=DIRECTION('ref_axis',(-0.99065493718706,0.136392065117079,1.66902952191827E-17));
#11222=DIRECTION('center_axis',(-2.46563637061793E-17,-5.67162995353388E-17,
-1.));
#11223=DIRECTION('ref_axis',(-0.99065493718706,0.136392065117079,1.66902952191827E-17));
#11224=DIRECTION('center_axis',(-2.46563637061793E-17,-5.67162995353388E-17,
-1.));
#11225=DIRECTION('ref_axis',(-0.99065493718706,0.136392065117079,1.66902952191827E-17));
#11226=DIRECTION('center_axis',(-2.46563637061793E-17,-5.67162995353388E-17,
-1.));
#11227=DIRECTION('ref_axis',(-0.99065493718706,0.136392065117078,1.66902952191827E-17));
#11228=DIRECTION('center_axis',(-2.46563637061793E-17,-5.67162995353388E-17,
-1.));
#11229=DIRECTION('ref_axis',(-0.99065493718706,0.136392065117079,1.66902952191827E-17));
#11230=DIRECTION('center_axis',(2.46563637061793E-17,5.67162995353388E-17,
1.));
#11231=DIRECTION('ref_axis',(-0.990654937187061,0.136392065117072,1.66902952191831E-17));
#11232=DIRECTION('center_axis',(-2.46563637061793E-17,-5.67162995353388E-17,
-1.));
#11233=DIRECTION('ref_axis',(-0.99065493718706,0.136392065117079,1.66902952191827E-17));
#11234=DIRECTION('',(0.916721549040254,0.399526721916365,-4.52626971630091E-17));
#11235=DIRECTION('center_axis',(-2.46563637061793E-17,-5.67162995353388E-17,
-1.));
#11236=DIRECTION('ref_axis',(-0.99065493718706,0.136392065117079,1.66902952191826E-17));
#11237=DIRECTION('center_axis',(2.46563637061793E-17,5.67162995353388E-17,
1.));
#11238=DIRECTION('ref_axis',(-0.99065493718706,0.136392065117079,1.66902952191827E-17));
#11239=DIRECTION('center_axis',(2.46563637061793E-17,5.67162995353388E-17,
1.));
#11240=DIRECTION('ref_axis',(-0.99065493718706,0.136392065117079,1.66902952191827E-17));
#11241=DIRECTION('center_axis',(-2.46563637061793E-17,-5.67162995353388E-17,
-1.));
#11242=DIRECTION('ref_axis',(-0.99065493718706,0.136392065117079,1.66902952191827E-17));
#11243=DIRECTION('center_axis',(2.46563637061793E-17,5.67162995353388E-17,
1.));
#11244=DIRECTION('ref_axis',(-0.99065493718706,0.136392065117079,1.66902952191827E-17));
#11245=DIRECTION('center_axis',(-2.46563637061793E-17,-5.67162995353388E-17,
-1.));
#11246=DIRECTION('ref_axis',(-0.99065493718706,0.136392065117079,1.66902952191827E-17));
#11247=DIRECTION('center_axis',(-2.46563637061793E-17,-5.67162995353388E-17,
-1.));
#11248=DIRECTION('ref_axis',(-0.99065493718706,0.136392065117079,1.66902952191827E-17));
#11249=DIRECTION('center_axis',(2.46563637061793E-17,5.67162995353388E-17,
1.));
#11250=DIRECTION('ref_axis',(-0.990654937187061,0.136392065117077,1.66902952191828E-17));
#11251=DIRECTION('',(-0.916721549040254,-0.399526721916365,4.52626971630091E-17));
#11252=DIRECTION('center_axis',(2.46563637061793E-17,5.67162995353388E-17,
1.));
#11253=DIRECTION('ref_axis',(-0.990654937187061,0.136392065117077,1.66902952191828E-17));
#11254=DIRECTION('center_axis',(-2.46563637061793E-17,-5.67162995353388E-17,
-1.));
#11255=DIRECTION('ref_axis',(-0.99065493718706,0.136392065117079,1.66902952191827E-17));
#11256=DIRECTION('center_axis',(2.46563637061793E-17,5.67162995353388E-17,
1.));
#11257=DIRECTION('ref_axis',(-0.99065493718706,0.136392065117079,1.66902952191827E-17));
#11258=DIRECTION('center_axis',(2.46563637061793E-17,5.67162995353388E-17,
1.));
#11259=DIRECTION('ref_axis',(-0.99065493718706,0.136392065117078,1.66902952191827E-17));
#11260=DIRECTION('center_axis',(2.46563637061793E-17,5.67162995353388E-17,
1.));
#11261=DIRECTION('ref_axis',(-0.99065493718706,0.13639206511708,1.66902952191826E-17));
#11262=DIRECTION('center_axis',(-0.399526721916365,0.916721549040254,-4.21421777999594E-17));
#11263=DIRECTION('ref_axis',(-0.916721549040254,-0.399526721916365,4.52626971630091E-17));
#11264=DIRECTION('',(0.916721549040254,0.399526721916365,-4.52626971630091E-17));
#11265=DIRECTION('',(-0.916721549040254,-0.399526721916365,4.52626971630091E-17));
#11266=DIRECTION('',(-2.46563637061793E-17,-5.67162995353388E-17,-1.));
#11267=DIRECTION('',(-0.916721549040254,-0.399526721916365,4.52626971630091E-17));
#11268=DIRECTION('',(2.46563637061793E-17,5.67162995353388E-17,1.));
#11269=DIRECTION('',(-0.916721549040254,-0.399526721916365,4.52626971630091E-17));
#11270=DIRECTION('center_axis',(-2.46563637061793E-17,-5.67162995353388E-17,
-1.));
#11271=DIRECTION('ref_axis',(-0.99065493718706,0.136392065117079,1.66902952191827E-17));
#11272=DIRECTION('center_axis',(2.46563637061793E-17,5.67162995353388E-17,
1.));
#11273=DIRECTION('ref_axis',(-0.99065493718706,0.136392065117079,1.66902952191827E-17));
#11274=DIRECTION('',(2.46563637061793E-17,5.67162995353388E-17,1.));
#11275=DIRECTION('center_axis',(-2.46563637061793E-17,-5.67162995353388E-17,
-1.));
#11276=DIRECTION('ref_axis',(-0.99065493718706,0.136392065117079,1.66902952191827E-17));
#11277=DIRECTION('',(-2.46563637061793E-17,-5.67162995353388E-17,-1.));
#11278=DIRECTION('center_axis',(2.46563637061793E-17,5.67162995353388E-17,
1.));
#11279=DIRECTION('ref_axis',(0.99065493718706,-0.136392065117079,-1.66902952191827E-17));
#11280=DIRECTION('',(2.46563637061793E-17,5.67162995353388E-17,1.));
#11281=DIRECTION('center_axis',(2.46563637061793E-17,5.67162995353388E-17,
1.));
#11282=DIRECTION('ref_axis',(0.99065493718706,-0.136392065117079,-1.66902952191827E-17));
#11283=DIRECTION('center_axis',(-2.46563637061793E-17,-5.67162995353388E-17,
-1.));
#11284=DIRECTION('ref_axis',(0.960627000032841,-0.277841261888699,-7.92744046622962E-18));
#11285=DIRECTION('',(-2.46563637061793E-17,-5.67162995353388E-17,-1.));
#11286=DIRECTION('center_axis',(-2.46563637061793E-17,-5.67162995353388E-17,
-1.));
#11287=DIRECTION('ref_axis',(-0.99065493718706,0.136392065117079,1.66902952191827E-17));
#11288=DIRECTION('',(-2.46563637061793E-17,-5.67162995353388E-17,-1.));
#11289=DIRECTION('center_axis',(2.46563637061793E-17,5.67162995353388E-17,
1.));
#11290=DIRECTION('ref_axis',(-0.99065493718706,0.136392065117079,1.66902952191827E-17));
#11291=DIRECTION('center_axis',(-2.46563637061793E-17,-5.67162995353388E-17,
-1.));
#11292=DIRECTION('ref_axis',(-0.99065493718706,0.136392065117079,1.66902952191827E-17));
#11293=DIRECTION('center_axis',(2.46563637061793E-17,5.67162995353388E-17,
1.));
#11294=DIRECTION('ref_axis',(-0.99065493718706,0.136392065117079,1.66902952191827E-17));
#11295=DIRECTION('center_axis',(-2.46563637061793E-17,-5.67162995353388E-17,
-1.));
#11296=DIRECTION('ref_axis',(-0.99065493718706,0.136392065117079,1.66902952191827E-17));
#11297=DIRECTION('center_axis',(-0.136392065117079,-0.99065493718706,5.95492145178271E-17));
#11298=DIRECTION('ref_axis',(-2.46563637061793E-17,-5.67162995353388E-17,
-1.));
#11299=DIRECTION('',(-0.99065493718706,0.136392065117079,1.66902952191827E-17));
#11300=DIRECTION('',(-2.46563637061793E-17,-5.67162995353388E-17,-1.));
#11301=DIRECTION('',(-0.99065493718706,0.136392065117079,1.66902952191827E-17));
#11302=DIRECTION('center_axis',(-2.46563637061793E-17,-5.67162995353388E-17,
-1.));
#11303=DIRECTION('ref_axis',(-0.99065493718706,0.136392065117079,1.66902952191827E-17));
#11304=DIRECTION('center_axis',(0.494699854607087,-0.71082491082636,0.500000000000425));
#11305=DIRECTION('ref_axis',(0.285615094283029,-0.410394953572923,-0.866025403784193));
#11306=DIRECTION('center_axis',(2.46563637061793E-17,5.67162995353388E-17,
1.));
#11307=DIRECTION('ref_axis',(-0.990654937187061,0.136392065117072,1.66902952191831E-17));
#11308=DIRECTION('',(-2.46563637061793E-17,-5.67162995353388E-17,-1.));
#11309=DIRECTION('center_axis',(-2.46563637061793E-17,-5.67162995353388E-17,
-1.));
#11310=DIRECTION('ref_axis',(-0.99065493718706,0.136392065117079,1.66902952191827E-17));
#11311=DIRECTION('center_axis',(-0.494699854607571,0.710824910827106,0.499999999998885));
#11312=DIRECTION('ref_axis',(0.285615094167233,-0.410394953651635,0.866025403785083));
#11313=DIRECTION('center_axis',(-2.46563637061793E-17,-5.67162995353388E-17,
-1.));
#11314=DIRECTION('ref_axis',(-0.99065493718706,0.136392065117079,1.66902952191827E-17));
#11315=DIRECTION('center_axis',(2.46563637061793E-17,5.67162995353388E-17,
1.));
#11316=DIRECTION('ref_axis',(-0.990654937187061,0.136392065117077,1.66902952191828E-17));
#11317=DIRECTION('center_axis',(-2.46563637061793E-17,-5.67162995353388E-17,
-1.));
#11318=DIRECTION('ref_axis',(-0.99065493718706,0.136392065117079,1.66902952191827E-17));
#11319=DIRECTION('center_axis',(2.46563637061793E-17,5.67162995353388E-17,
1.));
#11320=DIRECTION('ref_axis',(0.99065493718706,-0.136392065117079,-1.66902952191827E-17));
#11321=DIRECTION('center_axis',(-2.46563637061793E-17,-5.67162995353388E-17,
-1.));
#11322=DIRECTION('ref_axis',(0.99065493718706,-0.136392065117079,-1.66902952191827E-17));
#11323=DIRECTION('center_axis',(2.46563637061793E-17,5.67162995353388E-17,
1.));
#11324=DIRECTION('ref_axis',(0.99065493718706,-0.136392065117079,-1.66902952191827E-17));
#11325=DIRECTION('center_axis',(2.46563637061793E-17,5.67162995353388E-17,
1.));
#11326=DIRECTION('ref_axis',(0.99065493718706,-0.136392065117079,-1.66902952191827E-17));
#11327=DIRECTION('',(-0.820789907224822,-0.57123018845109,5.26357569507164E-17));
#11328=DIRECTION('',(-0.78773404285246,-0.616015484976895,5.43607758286658E-17));
#11329=DIRECTION('',(0.616015484976899,-0.787734042852457,2.94886580823745E-17));
#11330=DIRECTION('',(-0.78773404285246,-0.616015484976895,5.43607758286658E-17));
#11331=DIRECTION('',(0.616015484976899,-0.787734042852457,2.94886580823745E-17));
#11332=DIRECTION('',(-0.78773404285246,-0.616015484976895,5.43607758286658E-17));
#11333=DIRECTION('',(0.616015484976899,-0.787734042852457,2.94886580823745E-17));
#11334=DIRECTION('',(-0.78773404285246,-0.616015484976895,5.43607758286658E-17));
#11335=DIRECTION('',(0.616015484976899,-0.787734042852457,2.94886580823745E-17));
#11336=DIRECTION('',(-0.78773404285246,-0.616015484976895,5.43607758286658E-17));
#11337=DIRECTION('',(0.616015484976899,-0.787734042852457,2.94886580823745E-17));
#11338=DIRECTION('',(-0.78773404285246,-0.616015484976895,5.43607758286658E-17));
#11339=DIRECTION('',(0.616015484976899,-0.787734042852457,2.94886580823745E-17));
#11340=DIRECTION('',(-0.78773404285246,-0.616015484976895,5.43607758286658E-17));
#11341=DIRECTION('',(0.616015484976899,-0.787734042852457,2.94886580823745E-17));
#11342=DIRECTION('',(-0.78773404285246,-0.616015484976895,5.43607758286658E-17));
#11343=DIRECTION('',(0.616015484976899,-0.787734042852457,2.94886580823745E-17));
#11344=DIRECTION('',(-0.78773404285246,-0.616015484976895,5.43607758286658E-17));
#11345=DIRECTION('',(0.616015484976899,-0.787734042852457,2.94886580823745E-17));
#11346=DIRECTION('center_axis',(2.46563637061793E-17,5.67162995353388E-17,
1.));
#11347=DIRECTION('ref_axis',(0.99065493718706,-0.136392065117079,-1.66902952191827E-17));
#11348=DIRECTION('',(0.499271281878494,0.026984941938175,-0.866025403784438));
#11349=DIRECTION('center_axis',(-2.46563637061793E-17,-5.67162995353388E-17,
-1.));
#11350=DIRECTION('ref_axis',(-0.99065493718706,0.136392065117079,1.66902952191827E-17));
#11351=DIRECTION('',(0.498008733493835,-0.0445791584024184,-0.866025403784438));
#11352=DIRECTION('center_axis',(2.46563637061793E-17,5.67162995353388E-17,
1.));
#11353=DIRECTION('ref_axis',(-0.96497141127135,0.262355056038528,8.91287813947976E-18));
#11354=DIRECTION('center_axis',(-0.494699854607216,0.710824910826568,-0.500000000000001));
#11355=DIRECTION('ref_axis',(-0.820789907224822,-0.57123018845109,2.73331257345188E-17));
#11356=DIRECTION('center_axis',(2.46563637061793E-17,5.67162995353388E-17,
1.));
#11357=DIRECTION('ref_axis',(0.99065493718706,-0.136392065117079,-1.66902952191827E-17));
#11358=DIRECTION('center_axis',(-0.457286527460412,0.756141387770446,0.468123096528875));
#11359=DIRECTION('ref_axis',(-0.887435897002915,-0.422223938468998,-0.184890439164279));
#11360=DIRECTION('center_axis',(-2.46563637061793E-17,-5.67162995353388E-17,
-1.));
#11361=DIRECTION('ref_axis',(0.990654937187061,-0.136392065117078,-1.66902952191827E-17));
#11362=DIRECTION('center_axis',(-2.46563637061793E-17,-5.67162995353388E-17,
-1.));
#11363=DIRECTION('ref_axis',(0.99065493718706,-0.136392065117079,-1.66902952191827E-17));
#11364=DIRECTION('center_axis',(2.46563637061793E-17,5.67162995353388E-17,
1.));
#11365=DIRECTION('ref_axis',(0.990654937187061,-0.136392065117078,-1.66902952191827E-17));
#11366=DIRECTION('center_axis',(-0.457286527428201,0.756141387785753,-0.468123096535616));
#11367=DIRECTION('ref_axis',(-0.887545517051143,-0.421261555860625,0.186552021474719));
#11368=DIRECTION('center_axis',(-2.46563637061793E-17,-5.67162995353388E-17,
-1.));
#11369=DIRECTION('ref_axis',(0.990654937187061,-0.136392065117077,-1.66902952191827E-17));
#11370=DIRECTION('',(-0.499271281878494,-0.0269849419381751,-0.866025403784438));
#11371=DIRECTION('center_axis',(-0.494699854607216,0.710824910826568,0.500000000000001));
#11372=DIRECTION('ref_axis',(-0.820789907224822,-0.57123018845109,4.76302227498196E-17));
#11373=DIRECTION('',(-0.820789907224822,-0.57123018845109,5.26357569507164E-17));
#11374=DIRECTION('center_axis',(-2.46563637061793E-17,-5.67162995353388E-17,
-1.));
#11375=DIRECTION('ref_axis',(-0.964971411271351,0.262355056038526,8.91287813947992E-18));
#11376=DIRECTION('center_axis',(2.46563637061793E-17,5.67162995353388E-17,
1.));
#11377=DIRECTION('ref_axis',(0.99065493718706,-0.136392065117079,-1.66902952191827E-17));
#11378=DIRECTION('',(-0.498008733493835,0.0445791584024182,-0.866025403784438));
#11379=DIRECTION('center_axis',(-2.46563637061793E-17,-5.67162995353388E-17,
-1.));
#11380=DIRECTION('ref_axis',(0.99065493718706,-0.136392065117079,-1.66902952191827E-17));
#11381=DIRECTION('center_axis',(2.46563637061793E-17,5.67162995353388E-17,
1.));
#11382=DIRECTION('ref_axis',(-0.99065493718706,0.136392065117079,1.66902952191827E-17));
#11383=DIRECTION('center_axis',(2.46563637061793E-17,5.67162995353388E-17,
1.));
#11384=DIRECTION('ref_axis',(0.99065493718706,-0.136392065117079,-1.66902952191827E-17));
#11385=DIRECTION('center_axis',(2.46563637061793E-17,5.67162995353388E-17,
1.));
#11386=DIRECTION('ref_axis',(0.99065493718706,-0.136392065117079,-1.66902952191827E-17));
#11387=DIRECTION('',(0.616015484976889,-0.787734042852464,2.94886580823751E-17));
#11388=DIRECTION('',(-0.787734042852462,-0.616015484976892,5.43607758286657E-17));
#11389=DIRECTION('',(0.616015484976889,-0.787734042852464,2.94886580823751E-17));
#11390=DIRECTION('',(-0.787734042852462,-0.616015484976892,5.43607758286657E-17));
#11391=DIRECTION('',(0.616015484976889,-0.787734042852464,2.94886580823751E-17));
#11392=DIRECTION('',(-0.787734042852462,-0.616015484976892,5.43607758286657E-17));
#11393=DIRECTION('',(0.616015484976889,-0.787734042852464,2.94886580823751E-17));
#11394=DIRECTION('',(-0.787734042852462,-0.616015484976892,5.43607758286657E-17));
#11395=DIRECTION('',(0.616015484976889,-0.787734042852464,2.94886580823751E-17));
#11396=DIRECTION('',(-0.787734042852462,-0.616015484976892,5.43607758286657E-17));
#11397=DIRECTION('',(0.616015484976889,-0.787734042852464,2.94886580823751E-17));
#11398=DIRECTION('',(-0.787734042852462,-0.616015484976892,5.43607758286657E-17));
#11399=DIRECTION('',(0.616015484976889,-0.787734042852464,2.94886580823751E-17));
#11400=DIRECTION('',(-0.787734042852462,-0.616015484976892,5.43607758286657E-17));
#11401=DIRECTION('',(0.616015484976889,-0.787734042852464,2.94886580823751E-17));
#11402=DIRECTION('',(-0.787734042852462,-0.616015484976892,5.43607758286657E-17));
#11403=DIRECTION('',(0.616015484976889,-0.787734042852464,2.94886580823751E-17));
#11404=DIRECTION('',(-0.787734042852462,-0.616015484976892,5.43607758286657E-17));
#11405=DIRECTION('center_axis',(-2.46563637061793E-17,-5.67162995353388E-17,
-1.));
#11406=DIRECTION('ref_axis',(-0.99065493718706,0.136392065117079,0.));
#11407=DIRECTION('center_axis',(0.0539698838763491,-0.998542563756985,5.53029380587908E-17));
#11408=DIRECTION('ref_axis',(0.998542563756985,0.0539698838763491,-5.40660864842981E-32));
#11409=DIRECTION('center_axis',(-2.46563637061793E-17,-5.67162995353388E-17,
-1.));
#11410=DIRECTION('ref_axis',(-0.99065493718706,0.136392065117079,0.));
#11411=DIRECTION('center_axis',(-2.46563637061793E-17,-5.67162995353388E-17,
-1.));
#11412=DIRECTION('ref_axis',(-0.99065493718706,0.136392065117079,0.));
#11413=DIRECTION('center_axis',(0.0539698838763491,-0.998542563756986,5.53029380587908E-17));
#11414=DIRECTION('ref_axis',(0.998542563756985,0.0539698838763491,-5.4506213724986E-32));
#11415=DIRECTION('center_axis',(-2.46563637061793E-17,-5.67162995353388E-17,
-1.));
#11416=DIRECTION('ref_axis',(-0.99065493718706,0.136392065117079,0.));
#11417=DIRECTION('center_axis',(-2.46563637061793E-17,-5.67162995353388E-17,
-1.));
#11418=DIRECTION('ref_axis',(-0.99065493718706,0.136392065117079,1.66902952191827E-17));
#11419=DIRECTION('center_axis',(2.46563637061793E-17,5.67162995353388E-17,
1.));
#11420=DIRECTION('ref_axis',(-0.99065493718706,0.13639206511708,1.66902952191826E-17));
#11421=DIRECTION('center_axis',(-2.46563637061793E-17,-5.67162995353388E-17,
-1.));
#11422=DIRECTION('ref_axis',(0.990654937187061,-0.136392065117077,-1.66902952191828E-17));
#11423=DIRECTION('center_axis',(-0.99065493718706,0.136392065117079,1.66902952191827E-17));
#11424=DIRECTION('ref_axis',(-0.136392065117079,-0.99065493718706,5.95492145178272E-17));
#11425=DIRECTION('',(0.136392065117079,0.99065493718706,-5.95492145178271E-17));
#11426=DIRECTION('',(0.136392065117079,0.99065493718706,-5.95492145178271E-17));
#11427=DIRECTION('',(-2.46563637061793E-17,-5.67162995353388E-17,-1.));
#11428=DIRECTION('center_axis',(2.46563637061793E-17,5.67162995353388E-17,
1.));
#11429=DIRECTION('ref_axis',(0.99065493718706,-0.136392065117079,-1.66902952191827E-17));
#11430=DIRECTION('',(0.663255030075764,-0.748393456063852,2.60926501729039E-17));
#11431=DIRECTION('center_axis',(2.46563637061793E-17,5.67162995353388E-17,
1.));
#11432=DIRECTION('ref_axis',(0.99065493718706,-0.136392065117079,-1.66902952191827E-17));
#11433=DIRECTION('center_axis',(2.46563637061793E-17,5.67162995353388E-17,
1.));
#11434=DIRECTION('ref_axis',(0.99065493718706,-0.136392065117079,-1.66902952191827E-17));
#11435=DIRECTION('center_axis',(2.46563637061793E-17,5.67162995353388E-17,
1.));
#11436=DIRECTION('ref_axis',(0.99065493718706,-0.136392065117079,-1.66902952191827E-17));
#11437=DIRECTION('',(0.663255030075764,-0.748393456063852,2.60926501729039E-17));
#11438=DIRECTION('center_axis',(-2.46563637061793E-17,-5.67162995353388E-17,
-1.));
#11439=DIRECTION('ref_axis',(-0.99065493718706,0.136392065117079,1.66902952191827E-17));
#11440=DIRECTION('',(-2.46563637061793E-17,-5.67162995353388E-17,-1.));
#11441=DIRECTION('center_axis',(0.748393456063852,0.663255030075765,-5.6070032202132E-17));
#11442=DIRECTION('ref_axis',(-0.663255030075765,0.748393456063852,-2.60926501729039E-17));
#11443=DIRECTION('center_axis',(-0.787734042852464,-0.61601548497689,5.43607758286656E-17));
#11444=DIRECTION('ref_axis',(0.61601548497689,-0.787734042852464,2.94886580823751E-17));
#11445=DIRECTION('',(-2.46563637061793E-17,-5.67162995353388E-17,-1.));
#11446=DIRECTION('',(2.46563637061793E-17,5.67162995353388E-17,1.));
#11447=DIRECTION('center_axis',(-0.616015484976892,0.787734042852462,-2.9488658082375E-17));
#11448=DIRECTION('ref_axis',(-0.787734042852462,-0.616015484976892,5.43607758286657E-17));
#11449=DIRECTION('center_axis',(-0.616015484976892,0.787734042852462,-2.9488658082375E-17));
#11450=DIRECTION('ref_axis',(-0.787734042852462,-0.616015484976892,5.43607758286657E-17));
#11451=DIRECTION('',(2.46563637061793E-17,5.67162995353388E-17,1.));
#11452=DIRECTION('center_axis',(-0.616015484976892,0.787734042852462,-2.9488658082375E-17));
#11453=DIRECTION('ref_axis',(-0.787734042852462,-0.616015484976892,5.43607758286657E-17));
#11454=DIRECTION('',(2.46563637061793E-17,5.67162995353388E-17,1.));
#11455=DIRECTION('',(-2.46563637061793E-17,-5.67162995353388E-17,-1.));
#11456=DIRECTION('center_axis',(-0.616015484976892,0.787734042852462,-2.9488658082375E-17));
#11457=DIRECTION('ref_axis',(-0.787734042852462,-0.616015484976892,5.43607758286657E-17));
#11458=DIRECTION('',(2.46563637061793E-17,5.67162995353388E-17,1.));
#11459=DIRECTION('',(-2.46563637061793E-17,-5.67162995353388E-17,-1.));
#11460=DIRECTION('center_axis',(-0.616015484976892,0.787734042852462,-2.9488658082375E-17));
#11461=DIRECTION('ref_axis',(-0.787734042852462,-0.616015484976892,5.43607758286657E-17));
#11462=DIRECTION('',(2.46563637061793E-17,5.67162995353388E-17,1.));
#11463=DIRECTION('',(-2.46563637061793E-17,-5.67162995353388E-17,-1.));
#11464=DIRECTION('center_axis',(-0.616015484976892,0.787734042852462,-2.9488658082375E-17));
#11465=DIRECTION('ref_axis',(-0.787734042852462,-0.616015484976892,5.43607758286657E-17));
#11466=DIRECTION('',(2.46563637061793E-17,5.67162995353388E-17,1.));
#11467=DIRECTION('',(-2.46563637061793E-17,-5.67162995353388E-17,-1.));
#11468=DIRECTION('center_axis',(-0.616015484976892,0.787734042852462,-2.9488658082375E-17));
#11469=DIRECTION('ref_axis',(-0.787734042852462,-0.616015484976892,5.43607758286657E-17));
#11470=DIRECTION('',(2.46563637061793E-17,5.67162995353388E-17,1.));
#11471=DIRECTION('',(-2.46563637061793E-17,-5.67162995353388E-17,-1.));
#11472=DIRECTION('center_axis',(-0.787734042852464,-0.61601548497689,5.43607758286656E-17));
#11473=DIRECTION('ref_axis',(0.61601548497689,-0.787734042852464,2.94886580823751E-17));
#11474=DIRECTION('center_axis',(-0.787734042852464,-0.61601548497689,5.43607758286656E-17));
#11475=DIRECTION('ref_axis',(0.61601548497689,-0.787734042852464,2.94886580823751E-17));
#11476=DIRECTION('center_axis',(-0.787734042852464,-0.61601548497689,5.43607758286656E-17));
#11477=DIRECTION('ref_axis',(0.61601548497689,-0.787734042852464,2.94886580823751E-17));
#11478=DIRECTION('center_axis',(-0.787734042852464,-0.61601548497689,5.43607758286656E-17));
#11479=DIRECTION('ref_axis',(0.61601548497689,-0.787734042852464,2.94886580823751E-17));
#11480=DIRECTION('center_axis',(-0.787734042852464,-0.61601548497689,5.43607758286656E-17));
#11481=DIRECTION('ref_axis',(0.61601548497689,-0.787734042852464,2.94886580823751E-17));
#11482=DIRECTION('center_axis',(-0.787734042852464,-0.61601548497689,5.43607758286656E-17));
#11483=DIRECTION('ref_axis',(0.61601548497689,-0.787734042852464,2.94886580823751E-17));
#11484=DIRECTION('center_axis',(-0.616015484976892,0.787734042852462,-2.9488658082375E-17));
#11485=DIRECTION('ref_axis',(-0.787734042852462,-0.616015484976892,5.43607758286657E-17));
#11486=DIRECTION('',(2.46563637061793E-17,5.67162995353388E-17,1.));
#11487=DIRECTION('center_axis',(-0.787734042852464,-0.61601548497689,5.43607758286656E-17));
#11488=DIRECTION('ref_axis',(0.61601548497689,-0.787734042852464,2.94886580823751E-17));
#11489=DIRECTION('center_axis',(-0.787734042852464,-0.61601548497689,5.43607758286656E-17));
#11490=DIRECTION('ref_axis',(0.61601548497689,-0.787734042852464,2.94886580823751E-17));
#11491=DIRECTION('',(2.46563637061793E-17,5.67162995353388E-17,1.));
#11492=DIRECTION('center_axis',(-0.616015484976892,0.787734042852462,-2.9488658082375E-17));
#11493=DIRECTION('ref_axis',(-0.787734042852462,-0.616015484976892,5.43607758286657E-17));
#11494=DIRECTION('center_axis',(-2.46563637061793E-17,-5.67162995353388E-17,
-1.));
#11495=DIRECTION('ref_axis',(-0.99065493718706,0.136392065117079,0.));
#11496=DIRECTION('center_axis',(-0.989544138268184,0.144230365800956,1.62183475475996E-17));
#11497=DIRECTION('ref_axis',(-0.144230365800956,-0.989544138268184,2.55261967089169E-32));
#11498=DIRECTION('center_axis',(-0.368026070136058,0.929815471854609,-4.36615081756679E-17));
#11499=DIRECTION('ref_axis',(-0.929815471854609,-0.368026070136058,5.79450330564664E-32));
#11500=DIRECTION('center_axis',(-2.46563637061793E-17,-5.67162995353388E-17,
-1.));
#11501=DIRECTION('ref_axis',(-0.99065493718706,0.136392065117079,0.));
#11502=DIRECTION('center_axis',(-0.916721549040254,-0.399526721916366,4.52626971630092E-17));
#11503=DIRECTION('ref_axis',(0.399526721916366,-0.916721549040254,2.21817733744602E-31));
#11504=DIRECTION('center_axis',(-0.916721549040254,-0.399526721916365,4.52626971630091E-17));
#11505=DIRECTION('ref_axis',(0.399526721916365,-0.916721549040254,2.67901058084089E-31));
#11506=DIRECTION('center_axis',(-2.46563637061793E-17,-5.67162995353388E-17,
-1.));
#11507=DIRECTION('ref_axis',(-0.99065493718706,0.136392065117079,0.));
#11508=DIRECTION('center_axis',(0.157680228170735,0.98749022559417,-5.98946124780692E-17));
#11509=DIRECTION('ref_axis',(-0.98749022559417,0.157680228170735,2.28905066400457E-31));
#11510=DIRECTION('center_axis',(-2.46563637061793E-17,-5.67162995353388E-17,
-1.));
#11511=DIRECTION('ref_axis',(-0.99065493718706,0.136392065117079,0.));
#11512=DIRECTION('center_axis',(0.708008807113558,0.706203603112896,-5.75101777424565E-17));
#11513=DIRECTION('ref_axis',(-0.706203603112896,0.708008807113558,-2.20184166772643E-31));
#11514=DIRECTION('center_axis',(0.585101922340639,0.486005175527197,-0.649195432696555));
#11515=DIRECTION('ref_axis',(0.103177631811544,0.749408921066127,0.654018841716556));
#11516=DIRECTION('center_axis',(-2.46563637061793E-17,-5.67162995353388E-17,
-1.));
#11517=DIRECTION('ref_axis',(-0.99065493718706,0.136392065117079,0.));
#11518=DIRECTION('center_axis',(-0.989544138268184,0.144230365800956,1.62183475475996E-17));
#11519=DIRECTION('ref_axis',(-0.144230365800956,-0.989544138268184,2.55261967089169E-32));
#11520=DIRECTION('center_axis',(-0.368026070136058,0.929815471854609,-4.36615081756679E-17));
#11521=DIRECTION('ref_axis',(-0.929815471854609,-0.368026070136058,5.79450330564664E-32));
#11522=DIRECTION('center_axis',(-2.46563637061793E-17,-5.67162995353388E-17,
-1.));
#11523=DIRECTION('ref_axis',(-0.99065493718706,0.136392065117079,0.));
#11524=DIRECTION('center_axis',(-0.916721549040254,-0.399526721916366,4.52626971630092E-17));
#11525=DIRECTION('ref_axis',(0.399526721916366,-0.916721549040254,2.21817733744602E-31));
#11526=DIRECTION('center_axis',(0.916721549040254,0.399526721916365,-4.52626971630091E-17));
#11527=DIRECTION('ref_axis',(-0.399526721916365,0.916721549040254,-2.67901058084089E-31));
#11528=DIRECTION('center_axis',(-2.46563637061793E-17,-5.67162995353388E-17,
-1.));
#11529=DIRECTION('ref_axis',(-0.99065493718706,0.136392065117079,0.));
#11530=DIRECTION('center_axis',(0.157680228170735,0.98749022559417,-5.98946124780692E-17));
#11531=DIRECTION('ref_axis',(-0.98749022559417,0.157680228170735,2.28905066400457E-31));
#11532=DIRECTION('center_axis',(-2.46563637061793E-17,-5.67162995353388E-17,
-1.));
#11533=DIRECTION('ref_axis',(-0.99065493718706,0.136392065117079,0.));
#11534=DIRECTION('center_axis',(0.708008807113593,0.70620360311286,-1.88773974627704E-13));
#11535=DIRECTION('ref_axis',(-0.70620360311286,0.708008807113593,9.97021596630967E-28));
#11536=DIRECTION('center_axis',(0.585101922340452,0.486005175526929,0.649195432696924));
#11537=DIRECTION('ref_axis',(-0.103177631811576,-0.749408921066484,0.654018841716142));
#11538=DIRECTION('center_axis',(0.0527382027779713,-0.500066547561434,0.864379621449822));
#11539=DIRECTION('ref_axis',(-0.118759166955581,-0.862582108275705,-0.491780811690185));
#11540=DIRECTION('center_axis',(0.117812303642623,-0.993035881079037,5.34164974729424E-17));
#11541=DIRECTION('ref_axis',(0.993035881079037,0.117812303642623,-1.38256563133947E-31));
#11542=DIRECTION('center_axis',(-2.46563637061793E-17,-5.67162995353388E-17,
-1.));
#11543=DIRECTION('ref_axis',(-0.99065493718706,0.136392065117079,0.));
#11544=DIRECTION('center_axis',(0.231338519431928,-0.972873316227269,4.94738077387215E-17));
#11545=DIRECTION('ref_axis',(0.972873316227269,0.231338519431928,-7.26928861059308E-32));
#11546=DIRECTION('center_axis',(-2.46563637061793E-17,-5.67162995353388E-17,
-1.));
#11547=DIRECTION('ref_axis',(-0.99065493718706,0.136392065117079,0.));
#11548=DIRECTION('center_axis',(0.910390173593427,-0.413750808850605,1.01950357310838E-18));
#11549=DIRECTION('ref_axis',(0.413750808850605,0.910390173593427,3.00458402755694E-33));
#11550=DIRECTION('center_axis',(-2.46563637061793E-17,-5.67162995353388E-17,
-1.));
#11551=DIRECTION('ref_axis',(0.960627000032841,-0.2778412618887,0.));
#11552=DIRECTION('center_axis',(-0.990695324577823,0.136098397711516,1.67079467539161E-17));
#11553=DIRECTION('ref_axis',(-0.136098397711516,-0.990695324577823,-3.08356560958003E-32));
#11554=DIRECTION('center_axis',(0.,0.,1.));
#11555=DIRECTION('ref_axis',(-0.990695324577823,0.136098397711516,0.));
#11556=DIRECTION('center_axis',(2.46563637061793E-17,5.67162995353388E-17,
1.));
#11557=DIRECTION('ref_axis',(0.99065493718706,-0.136392065117079,-1.66902952191826E-17));
#11558=DIRECTION('center_axis',(-2.46563637061793E-17,-5.67162995353388E-17,
-1.));
#11559=DIRECTION('ref_axis',(-0.99065493718706,0.13639206511708,1.66902952191826E-17));
#11560=DIRECTION('center_axis',(2.46563637061793E-17,5.67162995353388E-17,
1.));
#11561=DIRECTION('ref_axis',(0.99065493718706,-0.136392065117079,-1.66902952191826E-17));
#11562=DIRECTION('center_axis',(0.,0.,1.));
#11563=DIRECTION('ref_axis',(-0.990695324577823,0.136098397711516,0.));
#11564=DIRECTION('center_axis',(0.990695324577823,-0.136098397711516,-1.67079467539161E-17));
#11565=DIRECTION('ref_axis',(0.136098397711516,0.990695324577823,3.19570144840529E-32));
#11566=DIRECTION('center_axis',(-2.46563637061793E-17,-5.67162995353388E-17,
-1.));
#11567=DIRECTION('ref_axis',(0.960627000032841,-0.2778412618887,0.));
#11568=DIRECTION('center_axis',(-0.910390173593428,0.413750808850603,-1.01950357310826E-18));
#11569=DIRECTION('ref_axis',(-0.413750808850603,-0.910390173593428,-1.1114346208305E-33));
#11570=DIRECTION('center_axis',(-2.46563637061793E-17,-5.67162995353388E-17,
-1.));
#11571=DIRECTION('ref_axis',(-0.99065493718706,0.136392065117079,0.));
#11572=DIRECTION('center_axis',(-0.231338519431928,0.972873316227269,-4.94738077387215E-17));
#11573=DIRECTION('ref_axis',(-0.972873316227269,-0.231338519431928,7.26928861059308E-32));
#11574=DIRECTION('center_axis',(-2.46563637061793E-17,-5.67162995353388E-17,
-1.));
#11575=DIRECTION('ref_axis',(-0.99065493718706,0.136392065117079,0.));
#11576=DIRECTION('center_axis',(-0.117812303642623,0.993035881079037,-5.34164974729424E-17));
#11577=DIRECTION('ref_axis',(-0.993035881079037,-0.117812303642623,1.38256563133947E-31));
#11578=DIRECTION('center_axis',(-0.0527382027779737,0.500066547561435,0.864379621449822));
#11579=DIRECTION('ref_axis',(-0.118759166955581,-0.862582108275704,0.491780811690186));
#11580=DIRECTION('axis',(0.,0.,1.));
#11581=DIRECTION('refdir',(1.,0.,0.));
#11582=DIRECTION('center_axis',(4.00113358033595E-18,-1.90170940755474E-18,
-1.));
#11583=DIRECTION('ref_axis',(-0.925927934137781,0.377700226083253,0.));
#11584=DIRECTION('center_axis',(-4.00113358033595E-18,1.90170940755474E-18,
1.));
#11585=DIRECTION('ref_axis',(-0.925927934137781,0.377700226083253,-4.42303742342784E-18));
#11586=DIRECTION('center_axis',(4.00113358033595E-18,-1.90170940755474E-18,
-1.));
#11587=DIRECTION('ref_axis',(-0.925927934137781,0.377700226083253,-4.42303742342784E-18));
#11588=DIRECTION('center_axis',(4.00113358033595E-18,-1.90170940755474E-18,
-1.));
#11589=DIRECTION('ref_axis',(-0.925927934137781,0.377700226083253,0.));
#11590=DIRECTION('center_axis',(-4.00113358033595E-18,1.90170940755474E-18,
1.));
#11591=DIRECTION('ref_axis',(-0.925927934137781,0.377700226083253,-4.42303742342784E-18));
#11592=DIRECTION('center_axis',(4.00113358033595E-18,-1.90170940755474E-18,
-1.));
#11593=DIRECTION('ref_axis',(-0.925927934137781,0.377700226083253,-4.42303742342784E-18));
#11594=DIRECTION('center_axis',(4.00113358033595E-18,-1.90170940755474E-18,
-1.));
#11595=DIRECTION('ref_axis',(-0.925927934137781,0.377700226083253,0.));
#11596=DIRECTION('center_axis',(-4.00113358033595E-18,1.90170940755474E-18,
1.));
#11597=DIRECTION('ref_axis',(-0.925927934137781,0.377700226083253,-4.42303742342784E-18));
#11598=DIRECTION('center_axis',(4.00113358033595E-18,-1.90170940755474E-18,
-1.));
#11599=DIRECTION('ref_axis',(-0.925927934137781,0.377700226083253,-4.42303742342784E-18));
#11600=DIRECTION('center_axis',(4.00113358033595E-18,-1.90170940755474E-18,
-1.));
#11601=DIRECTION('ref_axis',(-0.925927934137781,0.377700226083253,0.));
#11602=DIRECTION('center_axis',(-4.00113358033595E-18,1.90170940755474E-18,
1.));
#11603=DIRECTION('ref_axis',(-0.925927934137781,0.377700226083253,-4.42303742342784E-18));
#11604=DIRECTION('center_axis',(4.00113358033595E-18,-1.90170940755474E-18,
-1.));
#11605=DIRECTION('ref_axis',(-0.925927934137781,0.377700226083253,-4.42303742342784E-18));
#11606=DIRECTION('center_axis',(4.00113358033595E-18,-1.90170940755474E-18,
-1.));
#11607=DIRECTION('ref_axis',(-0.925927934137781,0.377700226083253,-4.42303742342784E-18));
#11608=DIRECTION('center_axis',(-4.00113358033595E-18,1.90170940755474E-18,
1.));
#11609=DIRECTION('ref_axis',(-0.925927934137761,0.377700226083302,-4.42303742342785E-18));
#11610=DIRECTION('',(-4.00113358033595E-18,1.90170940755474E-18,1.));
#11611=DIRECTION('center_axis',(-4.00113358033595E-18,1.90170940755474E-18,
1.));
#11612=DIRECTION('ref_axis',(-0.925927934137761,0.377700226083302,-4.42303742342785E-18));
#11613=DIRECTION('',(4.00113358033595E-18,-1.90170940755474E-18,-1.));
#11614=DIRECTION('center_axis',(-4.00113358033595E-18,1.90170940755474E-18,
1.));
#11615=DIRECTION('ref_axis',(0.925927934137781,-0.377700226083254,4.42303742342784E-18));
#11616=DIRECTION('center_axis',(4.00113358033595E-18,-1.90170940755474E-18,
-1.));
#11617=DIRECTION('ref_axis',(-0.925927934137781,0.377700226083254,-4.42303742342784E-18));
#11618=DIRECTION('',(-4.00113358033595E-18,1.90170940755474E-18,1.));
#11619=DIRECTION('center_axis',(4.00113358033595E-18,-1.90170940755474E-18,
-1.));
#11620=DIRECTION('ref_axis',(-0.925927934137781,0.377700226083254,-4.42303742342784E-18));
#11621=DIRECTION('center_axis',(4.00113358033595E-18,-1.90170940755474E-18,
-1.));
#11622=DIRECTION('ref_axis',(-0.925927934137781,0.377700226083254,-4.42303742342784E-18));
#11623=DIRECTION('center_axis',(-4.00113358033595E-18,1.90170940755474E-18,
1.));
#11624=DIRECTION('ref_axis',(0.925927934137781,-0.377700226083254,4.42303742342784E-18));
#11625=DIRECTION('',(4.00113358033595E-18,-1.90170940755474E-18,-1.));
#11626=DIRECTION('center_axis',(-8.58733520598719E-17,-1.9880713026183E-16,
1.));
#11627=DIRECTION('ref_axis',(-0.377700226083251,-0.925927934137782,-2.16515459902737E-16));
#11628=DIRECTION('center_axis',(4.00113358033595E-18,-1.90170940755474E-18,
-1.));
#11629=DIRECTION('ref_axis',(-0.925927934137783,0.377700226083249,-4.42303742342784E-18));
#11630=DIRECTION('center_axis',(-4.00113358033595E-18,1.90170940755474E-18,
1.));
#11631=DIRECTION('ref_axis',(0.925927934137783,-0.377700226083249,4.42303742342784E-18));
#11632=DIRECTION('',(4.00113358033595E-18,-1.90170940755474E-18,-1.));
#11633=DIRECTION('center_axis',(-4.00113358033595E-18,1.90170940755474E-18,
1.));
#11634=DIRECTION('ref_axis',(-0.925927934137783,0.377700226083249,-4.42303742342784E-18));
#11635=DIRECTION('center_axis',(4.00113358033595E-18,-1.90170940755474E-18,
-1.));
#11636=DIRECTION('ref_axis',(-0.925927934137781,0.377700226083253,-4.42303742342784E-18));
#11637=DIRECTION('',(4.00113358033595E-18,-1.90170940755474E-18,-1.));
#11638=DIRECTION('center_axis',(4.00113358033595E-18,-1.90170940755474E-18,
-1.));
#11639=DIRECTION('ref_axis',(-0.925927934137781,0.377700226083253,-4.42303742342784E-18));
#11640=DIRECTION('',(4.00113358033595E-18,-1.90170940755474E-18,-1.));
#11641=DIRECTION('center_axis',(-4.00113358033595E-18,1.90170940755474E-18,
1.));
#11642=DIRECTION('ref_axis',(0.925927934137781,-0.377700226083254,4.42303742342784E-18));
#11643=DIRECTION('center_axis',(4.00113358033595E-18,-1.90170940755474E-18,
-1.));
#11644=DIRECTION('ref_axis',(-0.925927934137781,0.377700226083254,-4.42303742342784E-18));
#11645=DIRECTION('',(-4.00113358033595E-18,1.90170940755474E-18,1.));
#11646=DIRECTION('center_axis',(4.00113358033595E-18,-1.90170940755474E-18,
-1.));
#11647=DIRECTION('ref_axis',(-0.925927934137781,0.377700226083254,-4.42303742342784E-18));
#11648=DIRECTION('center_axis',(4.00113358033595E-18,-1.90170940755474E-18,
-1.));
#11649=DIRECTION('ref_axis',(-0.925927934137781,0.377700226083254,-4.42303742342784E-18));
#11650=DIRECTION('center_axis',(5.31244646680575E-17,1.18523594394076E-16,
-1.));
#11651=DIRECTION('ref_axis',(0.377700226083251,0.925927934137782,1.29809429219568E-16));
#11652=DIRECTION('',(4.00113358033595E-18,-1.90170940755474E-18,-1.));
#11653=DIRECTION('center_axis',(-4.00113358033595E-18,1.90170940755474E-18,
1.));
#11654=DIRECTION('ref_axis',(0.925927934137781,-0.377700226083254,4.42303742342784E-18));
#11655=DIRECTION('center_axis',(4.00113358033595E-18,-1.90170940755474E-18,
-1.));
#11656=DIRECTION('ref_axis',(-0.925927934137783,0.377700226083249,-4.42303742342784E-18));
#11657=DIRECTION('center_axis',(-4.00113358033595E-18,1.90170940755474E-18,
1.));
#11658=DIRECTION('ref_axis',(-0.925927934137783,0.377700226083249,-4.42303742342784E-18));
#11659=DIRECTION('',(4.00113358033595E-18,-1.90170940755474E-18,-1.));
#11660=DIRECTION('center_axis',(-4.00113358033595E-18,1.90170940755474E-18,
1.));
#11661=DIRECTION('ref_axis',(0.925927934137783,-0.377700226083249,4.42303742342784E-18));
#11662=DIRECTION('center_axis',(4.00113358033595E-18,-1.90170940755474E-18,
-1.));
#11663=DIRECTION('ref_axis',(-0.925927934137781,0.377700226083253,-4.42303742342784E-18));
#11664=DIRECTION('center_axis',(4.00113358033595E-18,-1.90170940755474E-18,
-1.));
#11665=DIRECTION('ref_axis',(-0.925927934137781,0.377700226083253,-4.42303742342784E-18));
#11666=DIRECTION('',(4.00113358033595E-18,-1.90170940755474E-18,-1.));
#11667=DIRECTION('',(4.00113358033595E-18,-1.90170940755474E-18,-1.));
#11668=DIRECTION('center_axis',(4.00113358033595E-18,-1.90170940755474E-18,
-1.));
#11669=DIRECTION('ref_axis',(-0.925927934137781,0.377700226083253,-4.42303742342784E-18));
#11670=DIRECTION('',(4.00113358033595E-18,-1.90170940755474E-18,-1.));
#11671=DIRECTION('',(4.00113358033595E-18,-1.90170940755474E-18,-1.));
#11672=DIRECTION('center_axis',(-0.925927934137781,0.377700226083253,-4.42303742342784E-18));
#11673=DIRECTION('ref_axis',(-4.00113358033595E-18,1.90170940755474E-18,
1.));
#11674=DIRECTION('',(4.00113358033595E-18,-1.90170940755474E-18,-1.));
#11675=DIRECTION('',(0.377700226083253,0.925927934137781,-2.49616805185364E-19));
#11676=DIRECTION('center_axis',(-0.925927934137781,0.377700226083253,-4.42303742342784E-18));
#11677=DIRECTION('ref_axis',(-4.00113358033595E-18,1.90170940755474E-18,
1.));
#11678=DIRECTION('',(4.00113358033595E-18,-1.90170940755474E-18,-1.));
#11679=DIRECTION('',(0.377700226083253,0.925927934137781,-2.49616805185364E-19));
#11680=DIRECTION('center_axis',(-0.925927934137781,0.377700226083253,-4.42303742342784E-18));
#11681=DIRECTION('ref_axis',(-0.377700226083253,-0.925927934137781,2.49616805185365E-19));
#11682=DIRECTION('',(0.377700226083253,0.925927934137781,-2.49616805185365E-19));
#11683=DIRECTION('',(4.00113358033595E-18,-1.90170940755474E-18,-1.));
#11684=DIRECTION('',(0.377700226083253,0.925927934137781,-2.49616805185365E-19));
#11685=DIRECTION('center_axis',(-0.999957006340362,0.00927283510161242,
-4.01859579470807E-18));
#11686=DIRECTION('ref_axis',(-0.00927283510161242,-0.999957006340362,1.86452579419776E-18));
#11687=DIRECTION('',(0.00927283510161242,0.999957006340362,-1.86452579419776E-18));
#11688=DIRECTION('',(-4.00113358033595E-18,1.90170940755474E-18,1.));
#11689=DIRECTION('',(0.00927283510161242,0.999957006340362,-1.86452579419776E-18));
#11690=DIRECTION('',(0.0087838870263115,0.947230192127013,-0.320433778574812));
#11691=DIRECTION('',(0.00927283510161242,0.999957006340362,-1.86452579419776E-18));
#11692=DIRECTION('center_axis',(0.999957006340363,-0.00927283510148195,
5.80621970068864E-14));
#11693=DIRECTION('ref_axis',(0.00927283510148195,0.999957006340363,-4.86701529800751E-12));
#11694=DIRECTION('center_axis',(4.00113358033595E-18,-1.90170940755474E-18,
-1.));
#11695=DIRECTION('ref_axis',(-0.925927934137781,0.377700226083253,-4.42303742342784E-18));
#11696=DIRECTION('center_axis',(-4.00113358033595E-18,1.90170940755474E-18,
1.));
#11697=DIRECTION('ref_axis',(-0.925927934137789,0.377700226083235,-4.42303742342784E-18));
#11698=DIRECTION('',(0.377700226083253,0.925927934137781,-2.49616805185365E-19));
#11699=DIRECTION('',(0.00927283510161242,0.999957006340362,-1.86452579419776E-18));
#11700=DIRECTION('',(-0.925927934137781,0.377700226083253,-4.42303742342784E-18));
#11701=DIRECTION('',(0.204644651309627,-0.978836332943542,2.68027284920621E-18));
#11702=DIRECTION('',(-0.377700226083253,-0.925927934137781,2.49616805185365E-19));
#11703=DIRECTION('center_axis',(4.00113358033595E-18,-1.90170940755474E-18,
-1.));
#11704=DIRECTION('ref_axis',(-0.925927934137781,0.377700226083253,-4.42303742342784E-18));
#11705=DIRECTION('',(-0.377700226083253,-0.925927934137781,2.49616805185364E-19));
#11706=DIRECTION('center_axis',(4.00113358033595E-18,-1.90170940755474E-18,
-1.));
#11707=DIRECTION('ref_axis',(-0.925927934137781,0.377700226083253,-4.42303742342784E-18));
#11708=DIRECTION('center_axis',(-4.00113358033595E-18,1.90170940755474E-18,
1.));
#11709=DIRECTION('ref_axis',(-0.925927934137781,0.377700226083255,-4.42303742342784E-18));
#11710=DIRECTION('',(0.377700226083253,0.925927934137781,-2.49616805185364E-19));
#11711=DIRECTION('center_axis',(-4.00113358033595E-18,1.90170940755474E-18,
1.));
#11712=DIRECTION('ref_axis',(-0.925927934137781,0.377700226083253,-4.42303742342784E-18));
#11713=DIRECTION('',(0.377700226083253,0.925927934137781,-2.49616805185365E-19));
#11714=DIRECTION('',(-0.204644651309627,0.978836332943542,-2.68027284920621E-18));
#11715=DIRECTION('',(-0.925927934137781,0.377700226083253,-4.42303742342784E-18));
#11716=DIRECTION('',(-0.00927283510161242,-0.999957006340362,1.86452579419776E-18));
#11717=DIRECTION('',(-0.377700226083253,-0.925927934137781,2.49616805185365E-19));
#11718=DIRECTION('center_axis',(0.925927934137782,-0.377700226083253,4.42303742342784E-18));
#11719=DIRECTION('ref_axis',(0.377700226083253,0.925927934137782,-2.49616805185365E-19));
#11720=DIRECTION('',(4.00113358033595E-18,-1.90170940755474E-18,-1.));
#11721=DIRECTION('',(-0.377700226083253,-0.925927934137781,2.49616805185365E-19));
#11722=DIRECTION('',(4.00113358033595E-18,-1.90170940755474E-18,-1.));
#11723=DIRECTION('',(0.377700226083253,0.925927934137781,-2.49616805185365E-19));
#11724=DIRECTION('center_axis',(4.00113358033595E-18,-1.90170940755474E-18,
-1.));
#11725=DIRECTION('ref_axis',(0.976179814676794,-0.216963060029996,4.31842652930035E-18));
#11726=DIRECTION('center_axis',(4.00113358033595E-18,-1.90170940755474E-18,
-1.));
#11727=DIRECTION('ref_axis',(-0.925927934137781,0.377700226083253,-4.42303742342784E-18));
#11728=DIRECTION('',(4.00113358033595E-18,-1.90170940755474E-18,-1.));
#11729=DIRECTION('center_axis',(-4.00113358033595E-18,1.90170940755474E-18,
1.));
#11730=DIRECTION('ref_axis',(-0.92592793413778,0.377700226083256,-4.42303742342784E-18));
#11731=DIRECTION('center_axis',(0.925927934137781,-0.377700226083253,4.42303742342784E-18));
#11732=DIRECTION('ref_axis',(0.377700226083253,0.925927934137781,-2.49616805185363E-19));
#11733=DIRECTION('',(-0.377700226083253,-0.925927934137781,2.49616805185364E-19));
#11734=DIRECTION('',(0.377700226083253,0.925927934137781,-2.49616805185364E-19));
#11735=DIRECTION('center_axis',(-0.925927934137781,0.377700226083253,-4.42303742342784E-18));
#11736=DIRECTION('ref_axis',(-0.377700226083253,-0.925927934137781,2.49616805185365E-19));
#11737=DIRECTION('',(4.00113358033595E-18,-1.90170940755474E-18,-1.));
#11738=DIRECTION('',(-0.377700226083253,-0.925927934137781,2.49616805185365E-19));
#11739=DIRECTION('',(0.377700226083253,0.925927934137781,-2.49616805185365E-19));
#11740=DIRECTION('center_axis',(-0.999957006340362,0.00927283510161242,
-4.01859579470807E-18));
#11741=DIRECTION('ref_axis',(-0.00927283510161242,-0.999957006340362,1.86452579419776E-18));
#11742=DIRECTION('',(0.00927283510161242,0.999957006340362,-1.86452579419776E-18));
#11743=DIRECTION('',(-4.00113358033595E-18,1.90170940755474E-18,1.));
#11744=DIRECTION('',(-0.00927283510161242,-0.999957006340362,1.86452579419776E-18));
#11745=DIRECTION('center_axis',(0.999957006340363,-0.00927283510148229,
-5.79011228582622E-14));
#11746=DIRECTION('ref_axis',(0.00927283510148229,0.999957006340363,-1.18393654034962E-11));
#11747=DIRECTION('',(0.00927283510161242,0.999957006340362,-1.86452579419776E-18));
#11748=DIRECTION('',(-0.0087838870263115,-0.947230192127013,-0.320433778574812));
#11749=DIRECTION('center_axis',(-0.129181085459131,-0.316686004743042,-0.939692620785909));
#11750=DIRECTION('ref_axis',(0.354922115319603,0.870087647088815,-0.342020143325666));
#11751=DIRECTION('',(0.925927934137781,-0.377700226083253,4.42303742342784E-18));
#11752=DIRECTION('center_axis',(-0.129181085459303,-0.316686004743113,-0.939692620785862));
#11753=DIRECTION('ref_axis',(-0.0335289983800865,0.948485905659743,-0.315040145112406));
#11754=DIRECTION('center_axis',(-0.129181085459041,-0.31668600474309,-0.939692620785906));
#11755=DIRECTION('ref_axis',(-0.251599743391323,0.927090266008532,-0.277851053259925));
#11756=DIRECTION('center_axis',(-4.00113358033595E-18,1.90170940755474E-18,
1.));
#11757=DIRECTION('ref_axis',(0.925927934137781,-0.377700226083253,4.42303742342784E-18));
#11758=DIRECTION('',(0.925927934137781,-0.377700226083253,4.42303742342784E-18));
#11759=DIRECTION('',(0.00927283510161242,0.999957006340362,-1.86452579419776E-18));
#11760=DIRECTION('center_axis',(-4.00113358033595E-18,1.90170940755474E-18,
1.));
#11761=DIRECTION('ref_axis',(0.925927934137781,-0.377700226083253,4.42303742342784E-18));
#11762=DIRECTION('',(0.204644651309627,-0.978836332943542,2.68027284920621E-18));
#11763=DIRECTION('center_axis',(-4.00113358033595E-18,1.90170940755474E-18,
1.));
#11764=DIRECTION('ref_axis',(0.925927934137781,-0.377700226083253,4.42303742342784E-18));
#11765=DIRECTION('center_axis',(4.00113358033595E-18,-1.90170940755474E-18,
-1.));
#11766=DIRECTION('ref_axis',(0.925927934137782,-0.377700226083252,4.42303742342784E-18));
#11767=DIRECTION('',(-0.00927283510161242,-0.999957006340362,1.86452579419776E-18));
#11768=DIRECTION('',(-0.204644651309627,0.978836332943542,-2.68027284920621E-18));
#11769=DIRECTION('center_axis',(-0.129181085459131,-0.316686004743042,0.939692620785909));
#11770=DIRECTION('ref_axis',(-0.354922115319603,-0.870087647088815,-0.342020143325666));
#11771=DIRECTION('center_axis',(-0.129181085458924,-0.316686004742943,0.939692620785971));
#11772=DIRECTION('ref_axis',(0.0335289983807529,-0.948485905659807,-0.315040145112141));
#11773=DIRECTION('center_axis',(-0.129181085459094,-0.316686004743076,0.939692620785903));
#11774=DIRECTION('ref_axis',(0.251599743391407,-0.927090266008522,-0.277851053259883));
#11775=DIRECTION('center_axis',(0.978836332943542,0.204644651309627,3.52728026279203E-18));
#11776=DIRECTION('ref_axis',(-0.204644651309627,0.978836332943542,-2.68027284920621E-18));
#11777=DIRECTION('',(-0.204644651309627,0.978836332943542,-2.68027284920621E-18));
#11778=DIRECTION('',(4.00113358033595E-18,-1.90170940755474E-18,-1.));
#11779=DIRECTION('',(0.204644651309627,-0.978836332943542,2.68027284920621E-18));
#11780=DIRECTION('center_axis',(0.978836332943539,0.204644651309642,-1.5115104670406E-14));
#11781=DIRECTION('ref_axis',(0.204644651309642,-0.978836332943539,-3.3090080010939E-12));
#11782=DIRECTION('center_axis',(0.978836332943534,0.204644651309665,3.08136968372797E-14));
#11783=DIRECTION('ref_axis',(0.204644651309665,-0.978836332943534,2.52482791984225E-12));
#11784=DIRECTION('center_axis',(4.00113358033595E-18,-1.90170940755474E-18,
-1.));
#11785=DIRECTION('ref_axis',(-0.925927934137781,0.377700226083253,-4.42303742342784E-18));
#11786=DIRECTION('center_axis',(-4.00113358033595E-18,1.90170940755474E-18,
1.));
#11787=DIRECTION('ref_axis',(-0.925927934137783,0.377700226083249,-4.42303742342784E-18));
#11788=DIRECTION('',(-0.377700226083253,-0.925927934137781,2.49616805185364E-19));
#11789=DIRECTION('center_axis',(4.00113358033595E-18,-1.90170940755474E-18,
-1.));
#11790=DIRECTION('ref_axis',(-0.925927934137781,0.377700226083253,-4.42303742342784E-18));
#11791=DIRECTION('',(-0.377700226083253,-0.925927934137781,2.49616805185365E-19));
#11792=DIRECTION('',(-0.925927934137781,0.377700226083253,-4.42303742342784E-18));
#11793=DIRECTION('center_axis',(4.00113358033595E-18,-1.90170940755474E-18,
-1.));
#11794=DIRECTION('ref_axis',(-0.925927934137781,0.377700226083253,-4.42303742342784E-18));
#11795=DIRECTION('center_axis',(-4.00113358033595E-18,1.90170940755474E-18,
1.));
#11796=DIRECTION('ref_axis',(-0.925927934137783,0.377700226083249,-4.42303742342784E-18));
#11797=DIRECTION('',(-0.925927934137781,0.377700226083253,-4.42303742342784E-18));
#11798=DIRECTION('',(-0.377700226083253,-0.925927934137781,2.49616805185365E-19));
#11799=DIRECTION('center_axis',(4.00113358033595E-18,-1.90170940755474E-18,
-1.));
#11800=DIRECTION('ref_axis',(-0.925927934137781,0.377700226083253,-4.42303742342784E-18));
#11801=DIRECTION('',(-0.377700226083253,-0.925927934137781,2.49616805185364E-19));
#11802=DIRECTION('center_axis',(0.925927934137782,-0.377700226083253,4.42303742342784E-18));
#11803=DIRECTION('ref_axis',(0.377700226083253,0.925927934137782,-2.49616805185365E-19));
#11804=DIRECTION('',(0.354922115319602,0.870087647088815,-0.342020143325666));
#11805=DIRECTION('',(-0.377700226083253,-0.925927934137781,2.49616805185365E-19));
#11806=DIRECTION('',(4.00113358033595E-18,-1.90170940755474E-18,-1.));
#11807=DIRECTION('',(-0.377700226083253,-0.925927934137781,2.49616805185365E-19));
#11808=DIRECTION('',(-0.354922115319602,-0.870087647088815,-0.342020143325666));
#11809=DIRECTION('',(4.00113358033595E-18,-1.90170940755474E-18,-1.));
#11810=DIRECTION('center_axis',(4.00113358033595E-18,-1.90170940755474E-18,
-1.));
#11811=DIRECTION('ref_axis',(0.975866572214553,-0.218367656108268,4.31984433794175E-18));
#11812=DIRECTION('',(4.00113358033595E-18,-1.90170940755474E-18,-1.));
#11813=DIRECTION('center_axis',(0.925927934137781,-0.377700226083253,4.42303742342784E-18));
#11814=DIRECTION('ref_axis',(0.377700226083253,0.925927934137781,-2.49616805185363E-19));
#11815=DIRECTION('center_axis',(-0.129181085459131,-0.316686004743042,-0.939692620785909));
#11816=DIRECTION('ref_axis',(0.354922115319603,0.870087647088815,-0.342020143325666));
#11817=DIRECTION('',(0.925927934137781,-0.377700226083253,4.42303742342784E-18));
#11818=DIRECTION('center_axis',(-4.00113358033595E-18,1.90170940755474E-18,
1.));
#11819=DIRECTION('ref_axis',(0.925927934137781,-0.377700226083253,4.42303742342784E-18));
#11820=DIRECTION('',(0.204644651309627,-0.978836332943542,2.68027284920621E-18));
#11821=DIRECTION('',(0.925927934137781,-0.377700226083253,4.42303742342784E-18));
#11822=DIRECTION('',(0.925927934137781,-0.377700226083253,4.42303742342784E-18));
#11823=DIRECTION('center_axis',(-4.00113358033595E-18,1.90170940755474E-18,
1.));
#11824=DIRECTION('ref_axis',(0.925927934137781,-0.377700226083253,4.42303742342784E-18));
#11825=DIRECTION('',(0.925927934137781,-0.377700226083253,4.42303742342784E-18));
#11826=DIRECTION('',(0.204644651309627,-0.978836332943542,2.68027284920621E-18));
#11827=DIRECTION('center_axis',(-0.129181085459131,-0.316686004743042,0.939692620785909));
#11828=DIRECTION('ref_axis',(-0.354922115319603,-0.870087647088815,-0.342020143325666));
#11829=DIRECTION('center_axis',(0.978836332943542,0.204644651309627,3.52728026279203E-18));
#11830=DIRECTION('ref_axis',(-0.204644651309627,0.978836332943542,-2.68027284920621E-18));
#11831=DIRECTION('',(4.00113358033595E-18,-1.90170940755474E-18,-1.));
#11832=DIRECTION('center_axis',(4.00113358033595E-18,-1.90170940755474E-18,
-1.));
#11833=DIRECTION('ref_axis',(0.976179814676794,-0.216963060029996,0.));
#11834=DIRECTION('center_axis',(0.377700226083253,0.925927934137781,-2.49616805185365E-19));
#11835=DIRECTION('ref_axis',(-0.925927934137782,0.377700226083253,-1.80221867215748E-34));
#11836=DIRECTION('center_axis',(4.00113358033595E-18,-1.90170940755474E-18,
-1.));
#11837=DIRECTION('ref_axis',(0.976179814676794,-0.216963060029996,0.));
#11838=DIRECTION('center_axis',(-0.377700226083253,-0.925927934137781,2.49616805185365E-19));
#11839=DIRECTION('ref_axis',(0.925927934137782,-0.377700226083253,4.55848320526634E-35));
#11840=DIRECTION('center_axis',(0.377700226083253,0.925927934137781,-2.49616805185364E-19));
#11841=DIRECTION('ref_axis',(-0.925927934137781,0.377700226083253,-1.53241463292932E-34));
#11842=DIRECTION('center_axis',(-0.377700226083253,-0.925927934137781,2.49616805185364E-19));
#11843=DIRECTION('ref_axis',(0.925927934137781,-0.377700226083253,1.53241463292932E-34));
#11844=DIRECTION('center_axis',(0.204644651309627,-0.978836332943542,2.68027284920621E-18));
#11845=DIRECTION('ref_axis',(0.978836332943542,0.204644651309627,-3.8498424257767E-34));
#11846=DIRECTION('',(0.204644651309627,-0.978836332943542,2.68027284920621E-18));
#11847=DIRECTION('center_axis',(-0.204644651309626,0.978836332943543,-2.68027284920621E-18));
#11848=DIRECTION('ref_axis',(-0.978836332943543,-0.204644651309626,2.50909234811124E-33));
#11849=DIRECTION('center_axis',(-0.377700226083253,-0.925927934137781,2.49616805185365E-19));
#11850=DIRECTION('ref_axis',(0.925927934137781,-0.377700226083253,-3.31576666279908E-34));
#11851=DIRECTION('center_axis',(-4.00113358033595E-18,1.90170940755474E-18,
1.));
#11852=DIRECTION('ref_axis',(-0.0982550627361708,0.99516126464343,0.));
#11853=DIRECTION('center_axis',(-4.00113358033595E-18,1.90170940755474E-18,
1.));
#11854=DIRECTION('ref_axis',(0.925927934137781,-0.377700226083253,4.42303742342784E-18));
#11855=DIRECTION('center_axis',(-0.00927283510160954,-0.999957006340362,
1.86452579419778E-18));
#11856=DIRECTION('ref_axis',(0.999957006340362,-0.00927283510160953,2.50052584644563E-34));
#11857=DIRECTION('center_axis',(0.00927283510161242,0.999957006340362,-1.86452579419776E-18));
#11858=DIRECTION('ref_axis',(-0.999957006340362,0.00927283510161242,-2.38242583230871E-34));
#11859=DIRECTION('',(0.00927283510161242,0.999957006340362,-1.86452579419776E-18));
#11860=DIRECTION('center_axis',(-0.204644651309627,0.978836332943542,-2.68027284920621E-18));
#11861=DIRECTION('ref_axis',(-0.978836332943542,-0.204644651309627,3.8498424257767E-34));
#11862=DIRECTION('center_axis',(-0.204644651309626,0.978836332943543,-2.68027284920621E-18));
#11863=DIRECTION('ref_axis',(-0.978836332943543,-0.204644651309626,2.50909234811124E-33));
#11864=DIRECTION('',(-0.204644651309627,0.978836332943542,-2.68027284920621E-18));
#11865=DIRECTION('center_axis',(0.377700226083253,0.925927934137781,-2.49616805185365E-19));
#11866=DIRECTION('ref_axis',(-0.925927934137781,0.377700226083253,3.31576666279908E-34));
#11867=DIRECTION('center_axis',(-4.00113358033595E-18,1.90170940755474E-18,
1.));
#11868=DIRECTION('ref_axis',(-0.0982550627361708,0.99516126464343,0.));
#11869=DIRECTION('center_axis',(-0.0092728351016097,-0.999957006340362,
-2.115631353514E-16));
#11870=DIRECTION('ref_axis',(0.999957006340362,-0.0092728351016097,-6.33219768041088E-32));
#11871=DIRECTION('center_axis',(4.00113358033595E-18,-1.90170940755474E-18,
-1.));
#11872=DIRECTION('ref_axis',(0.925927934137781,-0.377700226083253,4.42303742342784E-18));
#11873=DIRECTION('center_axis',(-0.00927283510161242,-0.999957006340362,
1.86452579419776E-18));
#11874=DIRECTION('ref_axis',(0.999957006340362,-0.00927283510161242,-8.42037297766392E-34));
#11875=DIRECTION('',(-0.00927283510161242,-0.999957006340362,1.86452579419776E-18));
#11876=DIRECTION('center_axis',(4.00113358033595E-18,-1.90170940755474E-18,
-1.));
#11877=DIRECTION('ref_axis',(-0.925927934137781,0.377700226083255,-4.42303742342784E-18));
#11878=DIRECTION('center_axis',(-0.377700226083253,-0.925927934137781,2.49616805185364E-19));
#11879=DIRECTION('ref_axis',(4.00113358033594E-18,-1.90170940755474E-18,
-1.));
#11880=DIRECTION('',(0.925927934137781,-0.377700226083253,4.42303742342784E-18));
#11881=DIRECTION('',(0.925927934137781,-0.377700226083253,4.42303742342784E-18));
#11882=DIRECTION('center_axis',(5.31244646680575E-17,1.18523594394076E-16,
-1.));
#11883=DIRECTION('ref_axis',(0.377700226083253,0.925927934137781,1.29809429219568E-16));
#11884=DIRECTION('center_axis',(-8.58733520598719E-17,-1.98807130261829E-16,
1.));
#11885=DIRECTION('ref_axis',(-0.377700226083253,-0.925927934137781,-2.16515459902737E-16));
#11886=DIRECTION('axis',(0.,0.,1.));
#11887=DIRECTION('refdir',(1.,0.,0.));
#11888=DIRECTION('center_axis',(0.,0.,1.));
#11889=DIRECTION('ref_axis',(1.,0.,0.));
#11890=DIRECTION('center_axis',(0.,0.,1.));
#11891=DIRECTION('ref_axis',(1.,0.,0.));
#11892=DIRECTION('center_axis',(0.,-1.,0.));
#11893=DIRECTION('ref_axis',(-1.,0.,0.));
#11894=DIRECTION('center_axis',(0.,0.,1.));
#11895=DIRECTION('ref_axis',(1.,0.,0.));
#11896=DIRECTION('center_axis',(0.,0.,1.));
#11897=DIRECTION('ref_axis',(1.,0.,0.));
#11898=DIRECTION('center_axis',(0.,-1.,0.));
#11899=DIRECTION('ref_axis',(-1.,0.,0.));
#11900=DIRECTION('center_axis',(0.,0.,-1.));
#11901=DIRECTION('ref_axis',(-1.,0.,0.));
#11902=DIRECTION('center_axis',(0.,0.,-1.));
#11903=DIRECTION('ref_axis',(-1.,0.,0.));
#11904=DIRECTION('',(0.,0.,1.));
#11905=DIRECTION('center_axis',(0.,0.,1.));
#11906=DIRECTION('ref_axis',(1.,0.,0.));
#11907=DIRECTION('center_axis',(0.,0.,1.));
#11908=DIRECTION('ref_axis',(1.,0.,0.));
#11909=DIRECTION('center_axis',(0.,0.,-1.));
#11910=DIRECTION('ref_axis',(1.,0.,0.));
#11911=DIRECTION('axis',(0.,0.,1.));
#11912=DIRECTION('refdir',(1.,0.,0.));
#11913=DIRECTION('center_axis',(0.00483401456277122,-0.999988316083346,
0.));
#11914=DIRECTION('ref_axis',(0.999988316083346,0.00483401456277122,0.));
#11915=DIRECTION('center_axis',(2.50063434304146E-17,1.27632226958495E-16,
1.));
#11916=DIRECTION('ref_axis',(0.00483401456277147,-0.999988316083347,1.27509854685889E-16));
#11917=DIRECTION('center_axis',(2.50063434304146E-17,1.27632226958495E-16,
1.));
#11918=DIRECTION('ref_axis',(0.00483401456276983,-0.999988316083346,1.27509854685889E-16));
#11919=DIRECTION('center_axis',(2.50063434304146E-17,1.27632226958495E-16,
1.));
#11920=DIRECTION('ref_axis',(0.00483401456276983,-0.999988316083346,1.27509854685889E-16));
#11921=DIRECTION('',(-2.50063434304146E-17,-1.27632226958495E-16,-1.));
#11922=DIRECTION('center_axis',(2.50063434304146E-17,1.27632226958495E-16,
1.));
#11923=DIRECTION('ref_axis',(0.00483401456276983,-0.999988316083346,1.27509854685889E-16));
#11924=DIRECTION('center_axis',(-0.00483401456277122,0.999988316083346,
0.));
#11925=DIRECTION('ref_axis',(0.999988316083346,0.00483401456277122,0.));
#11926=DIRECTION('center_axis',(2.50063434304146E-17,1.27632226958495E-16,
1.));
#11927=DIRECTION('ref_axis',(0.00483401456277147,-0.999988316083347,1.27509854685889E-16));
#11928=DIRECTION('center_axis',(2.50063434304146E-17,1.27632226958495E-16,
1.));
#11929=DIRECTION('ref_axis',(0.00483401456277099,-0.999988316083347,1.27509854685889E-16));
#11930=DIRECTION('center_axis',(-2.50063434304146E-17,-1.27632226958495E-16,
-1.));
#11931=DIRECTION('ref_axis',(0.00483401456277099,-0.999988316083347,1.27509854685889E-16));
#11932=DIRECTION('axis',(0.,0.,1.));
#11933=DIRECTION('refdir',(1.,0.,0.));
#11934=DIRECTION('center_axis',(4.00051694051949E-18,-1.90113600208472E-18,
-1.));
#11935=DIRECTION('ref_axis',(-0.348963627142735,-0.937136269136664,3.85588598105426E-19));
#11936=DIRECTION('center_axis',(-4.00051694051949E-18,1.90113600208472E-18,
1.));
#11937=DIRECTION('ref_axis',(0.348963627142735,0.937136269136664,-3.85588598105426E-19));
#11938=DIRECTION('',(4.00051694051949E-18,-1.90113600208472E-18,-1.));
#11939=DIRECTION('center_axis',(-4.00051694051949E-18,1.90113600208472E-18,
1.));
#11940=DIRECTION('ref_axis',(-0.348963627142721,-0.93713626913667,3.85588598105494E-19));
#11941=DIRECTION('center_axis',(-4.00051694051949E-18,1.90113600208472E-18,
1.));
#11942=DIRECTION('ref_axis',(-0.348963627142735,-0.937136269136664,3.85588598105426E-19));
#11943=DIRECTION('center_axis',(-4.00051694051949E-18,1.90113600208472E-18,
1.));
#11944=DIRECTION('ref_axis',(-0.348963627142721,-0.93713626913667,3.85588598105494E-19));
#11945=DIRECTION('center_axis',(4.00051694051949E-18,-1.90113600208472E-18,
-1.));
#11946=DIRECTION('ref_axis',(-0.587778313469371,0.809022035679562,-3.88947801881448E-18));
#11947=DIRECTION('center_axis',(-4.00051694051949E-18,1.90113600208472E-18,
1.));
#11948=DIRECTION('ref_axis',(-0.348963627142725,-0.937136269136668,3.85588598105472E-19));
#11949=DIRECTION('',(4.0005169405195E-18,-1.90113600208472E-18,-1.));
#11950=DIRECTION('',(0.,0.,-1.));
#11951=DIRECTION('',(4.0005169405195E-18,-1.90113600208472E-18,-1.));
#11952=DIRECTION('center_axis',(-4.00051694051949E-18,1.90113600208472E-18,
1.));
#11953=DIRECTION('ref_axis',(-0.348963627142725,-0.937136269136668,3.85588598105472E-19));
#11954=DIRECTION('',(4.0005169405195E-18,-1.90113600208472E-18,-1.));
#11955=DIRECTION('center_axis',(4.00051694051949E-18,-1.90113600208472E-18,
-1.));
#11956=DIRECTION('ref_axis',(-0.348963627142735,-0.937136269136664,3.85588598105426E-19));
#11957=DIRECTION('center_axis',(-4.00051694051949E-18,1.90113600208472E-18,
1.));
#11958=DIRECTION('ref_axis',(-0.348963627142721,-0.93713626913667,3.85588598105494E-19));
#11959=DIRECTION('',(4.00051694051949E-18,-1.90113600208472E-18,-1.));
#11960=DIRECTION('center_axis',(-4.00051694051949E-18,1.90113600208472E-18,
1.));
#11961=DIRECTION('ref_axis',(0.348963627142735,0.937136269136664,-3.85588598105426E-19));
#11962=DIRECTION('center_axis',(-4.00051694051949E-18,1.90113600208472E-18,
1.));
#11963=DIRECTION('ref_axis',(-0.348963627142721,-0.93713626913667,3.85588598105494E-19));
#11964=DIRECTION('center_axis',(-4.00051694051949E-18,1.90113600208472E-18,
1.));
#11965=DIRECTION('ref_axis',(-0.348963627142735,-0.937136269136664,3.85588598105426E-19));
#11966=DIRECTION('center_axis',(0.348963627142731,0.937136269136666,-3.85588598105444E-19));
#11967=DIRECTION('ref_axis',(4.00051694051949E-18,-1.90113600208472E-18,
-1.));
#11968=DIRECTION('',(4.0005169405195E-18,-1.90113600208472E-18,-1.));
#11969=DIRECTION('',(0.937136269136666,-0.348963627142731,4.41245683523558E-18));
#11970=DIRECTION('',(-4.0005169405195E-18,1.90113600208472E-18,1.));
#11971=DIRECTION('',(-0.937136269136666,0.348963627142731,-4.41245683523558E-18));
#11972=DIRECTION('',(4.0005169405195E-18,-1.90113600208472E-18,-1.));
#11973=DIRECTION('',(4.0005169405195E-18,-1.90113600208472E-18,-1.));
#11974=DIRECTION('center_axis',(4.00051694051949E-18,-1.90113600208472E-18,
-1.));
#11975=DIRECTION('ref_axis',(-0.348963627142731,-0.937136269136666,3.85588598105444E-19));
#11976=DIRECTION('center_axis',(4.00051694051949E-18,-1.90113600208472E-18,
-1.));
#11977=DIRECTION('ref_axis',(-0.348963627142731,-0.937136269136666,3.85588598105444E-19));
#11978=DIRECTION('center_axis',(4.00051694051949E-18,-1.90113600208472E-18,
-1.));
#11979=DIRECTION('ref_axis',(-0.348963627142731,-0.937136269136666,3.85588598105444E-19));
#11980=DIRECTION('center_axis',(4.00051694051949E-18,-1.90113600208472E-18,
-1.));
#11981=DIRECTION('ref_axis',(-0.348963627142731,-0.937136269136666,3.85588598105444E-19));
#11982=DIRECTION('',(0.937136269136666,-0.348963627142731,4.41245683523558E-18));
#11983=DIRECTION('center_axis',(-4.00051694051949E-18,1.90113600208472E-18,
1.));
#11984=DIRECTION('ref_axis',(-0.348963627142846,-0.937136269136623,3.85588598104903E-19));
#11985=DIRECTION('center_axis',(4.00051694051949E-18,-1.90113600208472E-18,
-1.));
#11986=DIRECTION('ref_axis',(-0.348963627142731,-0.937136269136666,3.85588598105444E-19));
#11987=DIRECTION('center_axis',(4.00051694051949E-18,-1.90113600208472E-18,
-1.));
#11988=DIRECTION('ref_axis',(-0.348963627142731,-0.937136269136666,3.85588598105444E-19));
#11989=DIRECTION('center_axis',(4.00051694051949E-18,-1.90113600208472E-18,
-1.));
#11990=DIRECTION('ref_axis',(-0.348963627142735,-0.937136269136664,3.85588598105426E-19));
#11991=DIRECTION('',(-0.937136269136666,0.348963627142731,-4.41245683523558E-18));
#11992=DIRECTION('',(4.0005169405195E-18,-1.90113600208472E-18,-1.));
#11993=DIRECTION('',(4.0005169405195E-18,-1.90113600208472E-18,-1.));
#11994=DIRECTION('center_axis',(4.00051694051949E-18,-1.90113600208472E-18,
-1.));
#11995=DIRECTION('ref_axis',(-0.348963627142731,-0.937136269136666,3.85588598105444E-19));
#11996=DIRECTION('center_axis',(4.00051694051949E-18,-1.90113600208472E-18,
-1.));
#11997=DIRECTION('ref_axis',(-0.348963627142731,-0.937136269136666,3.85588598105444E-19));
#11998=DIRECTION('center_axis',(4.00051694051949E-18,-1.90113600208472E-18,
-1.));
#11999=DIRECTION('ref_axis',(-0.348963627142731,-0.937136269136666,3.85588598105444E-19));
#12000=DIRECTION('center_axis',(4.00051694051949E-18,-1.90113600208472E-18,
-1.));
#12001=DIRECTION('ref_axis',(-0.348963627142731,-0.937136269136666,3.85588598105444E-19));
#12002=DIRECTION('',(4.0005169405195E-18,-1.90113600208472E-18,-1.));
#12003=DIRECTION('center_axis',(0.,0.,-1.));
#12004=DIRECTION('ref_axis',(-0.125309381306763,0.992117714264046,0.));
#12005=DIRECTION('center_axis',(-0.937136269136666,0.348963627142731,-4.41245683523558E-18));
#12006=DIRECTION('ref_axis',(-4.13507333629925E-18,1.53978694183454E-18,
1.));
#12007=DIRECTION('center_axis',(0.662655410802406,-0.246754547140085,0.707106781186538));
#12008=DIRECTION('ref_axis',(0.66265541080291,-0.246754547138675,-0.707106781186557));
#12009=DIRECTION('center_axis',(0.937136269136666,-0.348963627142731,4.41245683523558E-18));
#12010=DIRECTION('ref_axis',(4.13507333629925E-18,-1.53978694183454E-18,
-1.));
#12011=DIRECTION('center_axis',(0.662655410802405,-0.246754547140073,-0.707106781186543));
#12012=DIRECTION('ref_axis',(0.662655410801971,-0.246754547141213,0.707106781186552));
#12013=DIRECTION('center_axis',(4.00051694051949E-18,-1.90113600208472E-18,
-1.));
#12014=DIRECTION('ref_axis',(-0.348963627142735,-0.937136269136664,3.85588598105426E-19));
#12015=DIRECTION('center_axis',(-0.352532537381825,-0.935799556575623,3.68769839860518E-19));
#12016=DIRECTION('ref_axis',(0.935799556575623,-0.352532537381825,6.00067969352728E-34));
#12017=DIRECTION('center_axis',(-0.362140169981158,-0.932123649139972,2.90655021385084E-12));
#12018=DIRECTION('ref_axis',(0.932123649139972,-0.362140169981158,-2.43759966809478E-27));
#12019=DIRECTION('center_axis',(-0.352532537381905,-0.935799556575593,3.46813776064964E-15));
#12020=DIRECTION('ref_axis',(0.935799556575593,-0.352532537381904,-3.73856855277001E-30));
#12021=DIRECTION('center_axis',(-0.362140169981175,-0.932123649139966,-2.71107876657752E-13));
#12022=DIRECTION('ref_axis',(0.932123649139966,-0.362140169981175,-1.23386467665282E-27));
#12023=DIRECTION('axis',(0.,0.,1.));
#12024=DIRECTION('refdir',(1.,0.,0.));
#12025=DIRECTION('center_axis',(1.69724645484627E-17,2.39104395366563E-16,
-1.));
#12026=DIRECTION('ref_axis',(0.306109702391973,-0.951996244793801,0.));
#12027=DIRECTION('center_axis',(1.69724645484627E-17,2.39104395366563E-16,
-1.));
#12028=DIRECTION('ref_axis',(0.306109702391977,-0.951996244793799,-2.22431050430871E-16));
#12029=DIRECTION('center_axis',(0.9519962447938,0.306109702391975,8.9349897821304E-17));
#12030=DIRECTION('ref_axis',(-0.306109702391975,0.9519962447938,0.));
#12031=DIRECTION('center_axis',(-1.69724645484627E-17,-2.39104395366563E-16,
1.));
#12032=DIRECTION('ref_axis',(0.306109702391977,-0.951996244793799,-2.22431050430871E-16));
#12033=DIRECTION('center_axis',(1.69724645484627E-17,2.39104395366563E-16,
-1.));
#12034=DIRECTION('ref_axis',(0.306109702391976,-0.9519962447938,0.));
#12035=DIRECTION('center_axis',(-1.69724645484627E-17,-2.39104395366563E-16,
1.));
#12036=DIRECTION('ref_axis',(0.306109702391976,-0.9519962447938,-2.22431050430871E-16));
#12037=DIRECTION('center_axis',(0.306109702391976,-0.9519962447938,-2.22431050430871E-16));
#12038=DIRECTION('ref_axis',(6.80883026501286E-17,-2.1175352473573E-16,
1.));
#12039=DIRECTION('center_axis',(1.69724645484627E-17,2.39104395366563E-16,
-1.));
#12040=DIRECTION('ref_axis',(0.306109702391976,-0.9519962447938,-2.22431050430871E-16));
#12041=DIRECTION('center_axis',(-0.306109702391976,0.9519962447938,2.22431050430871E-16));
#12042=DIRECTION('ref_axis',(-6.80883026501286E-17,2.1175352473573E-16,
-1.));
#12043=DIRECTION('center_axis',(1.69724645484627E-17,2.39104395366563E-16,
-1.));
#12044=DIRECTION('ref_axis',(0.306109702391978,-0.951996244793799,0.));
#12045=DIRECTION('center_axis',(1.69724645484627E-17,2.39104395366563E-16,
-1.));
#12046=DIRECTION('ref_axis',(0.306109702391978,-0.951996244793799,-2.22431050430871E-16));
#12047=DIRECTION('center_axis',(0.951996244793799,0.306109702391978,8.93498978213047E-17));
#12048=DIRECTION('ref_axis',(-0.306109702391978,0.951996244793799,0.));
#12049=DIRECTION('center_axis',(-1.69724645484627E-17,-2.39104395366563E-16,
1.));
#12050=DIRECTION('ref_axis',(0.306109702391974,-0.9519962447938,-2.22431050430872E-16));
#12051=DIRECTION('center_axis',(1.69724645484627E-17,2.39104395366563E-16,
-1.));
#12052=DIRECTION('ref_axis',(0.306109702391976,-0.9519962447938,0.));
#12053=DIRECTION('center_axis',(-1.69724645484627E-17,-2.39104395366563E-16,
1.));
#12054=DIRECTION('ref_axis',(0.306109702391976,-0.9519962447938,-2.22431050430871E-16));
#12055=DIRECTION('center_axis',(-0.306109702391976,0.9519962447938,2.22431050430871E-16));
#12056=DIRECTION('ref_axis',(-6.80883026501286E-17,2.1175352473573E-16,
-1.));
#12057=DIRECTION('center_axis',(1.69724645484627E-17,2.39104395366563E-16,
-1.));
#12058=DIRECTION('ref_axis',(0.306109702391976,-0.9519962447938,-2.22431050430871E-16));
#12059=DIRECTION('center_axis',(0.306109702391976,-0.9519962447938,-2.22431050430871E-16));
#12060=DIRECTION('ref_axis',(6.80883026501286E-17,-2.1175352473573E-16,
1.));
#12061=DIRECTION('center_axis',(1.69724645484627E-17,2.39104395366563E-16,
-1.));
#12062=DIRECTION('ref_axis',(0.306109702391973,-0.951996244793801,0.));
#12063=DIRECTION('center_axis',(1.69724645484627E-17,2.39104395366563E-16,
-1.));
#12064=DIRECTION('ref_axis',(0.306109702391977,-0.951996244793799,-2.22431050430871E-16));
#12065=DIRECTION('center_axis',(0.9519962447938,0.306109702391975,8.9349897821304E-17));
#12066=DIRECTION('ref_axis',(-0.306109702391975,0.9519962447938,0.));
#12067=DIRECTION('center_axis',(-1.69724645484627E-17,-2.39104395366563E-16,
1.));
#12068=DIRECTION('ref_axis',(0.306109702391977,-0.951996244793799,-2.22431050430871E-16));
#12069=DIRECTION('center_axis',(1.69724645484627E-17,2.39104395366563E-16,
-1.));
#12070=DIRECTION('ref_axis',(0.306109702391978,-0.951996244793799,0.));
#12071=DIRECTION('center_axis',(1.69724645484627E-17,2.39104395366563E-16,
-1.));
#12072=DIRECTION('ref_axis',(0.306109702391977,-0.951996244793799,-2.22431050430871E-16));
#12073=DIRECTION('center_axis',(0.951996244793799,0.306109702391978,8.93498978213047E-17));
#12074=DIRECTION('ref_axis',(-0.306109702391978,0.951996244793799,0.));
#12075=DIRECTION('center_axis',(-1.69724645484627E-17,-2.39104395366563E-16,
1.));
#12076=DIRECTION('ref_axis',(0.306109702391972,-0.951996244793801,-2.22431050430872E-16));
#12077=DIRECTION('center_axis',(1.69724645484627E-17,2.39104395366563E-16,
-1.));
#12078=DIRECTION('ref_axis',(0.306109702391978,-0.951996244793799,-2.22431050430871E-16));
#12079=DIRECTION('',(1.69724645484627E-17,2.39104395366563E-16,-1.));
#12080=DIRECTION('center_axis',(1.69724645484627E-17,2.39104395366563E-16,
-1.));
#12081=DIRECTION('ref_axis',(0.306109702391977,-0.951996244793799,-2.22431050430871E-16));
#12082=DIRECTION('',(1.69724645484627E-17,2.39104395366563E-16,-1.));
#12083=DIRECTION('center_axis',(1.69724645484627E-17,2.39104395366563E-16,
-1.));
#12084=DIRECTION('ref_axis',(0.306109702391976,-0.9519962447938,-2.22431050430871E-16));
#12085=DIRECTION('',(1.69724645484627E-17,2.39104395366563E-16,-1.));
#12086=DIRECTION('',(1.69724645484627E-17,2.39104395366563E-16,-1.));
#12087=DIRECTION('center_axis',(1.69724645484627E-17,2.39104395366563E-16,
-1.));
#12088=DIRECTION('ref_axis',(0.306109702391976,-0.9519962447938,-2.22431050430872E-16));
#12089=DIRECTION('center_axis',(-1.69724645484627E-17,-2.39104395366563E-16,
1.));
#12090=DIRECTION('ref_axis',(0.306109702391974,-0.9519962447938,-2.22431050430872E-16));
#12091=DIRECTION('center_axis',(1.69724645484627E-17,2.39104395366563E-16,
-1.));
#12092=DIRECTION('ref_axis',(0.306109702391976,-0.9519962447938,-2.22431050430871E-16));
#12093=DIRECTION('',(-0.306109702391976,0.9519962447938,2.22431050430871E-16));
#12094=DIRECTION('center_axis',(1.69724645484627E-17,2.39104395366563E-16,
-1.));
#12095=DIRECTION('ref_axis',(0.306109702391976,-0.9519962447938,-2.22431050430871E-16));
#12096=DIRECTION('',(-0.306109702391976,0.9519962447938,2.22431050430871E-16));
#12097=DIRECTION('center_axis',(-1.69724645484627E-17,-2.39104395366563E-16,
1.));
#12098=DIRECTION('ref_axis',(0.306109702391974,-0.9519962447938,-2.22431050430872E-16));
#12099=DIRECTION('',(0.010034405174207,-0.999949654089045,-2.3892204885188E-16));
#12100=DIRECTION('center_axis',(1.69724645484627E-17,2.39104395366563E-16,
-1.));
#12101=DIRECTION('ref_axis',(0.306109702391976,-0.9519962447938,-2.22431050430872E-16));
#12102=DIRECTION('center_axis',(-1.69724645484627E-17,-2.39104395366563E-16,
1.));
#12103=DIRECTION('ref_axis',(0.306109702391978,-0.951996244793799,-2.22431050430871E-16));
#12104=DIRECTION('',(0.306109702391976,-0.9519962447938,-2.22431050430871E-16));
#12105=DIRECTION('center_axis',(-1.69724645484627E-17,-2.39104395366563E-16,
1.));
#12106=DIRECTION('ref_axis',(0.306109702391976,-0.9519962447938,-2.22431050430871E-16));
#12107=DIRECTION('center_axis',(1.69724645484627E-17,2.39104395366563E-16,
-1.));
#12108=DIRECTION('ref_axis',(0.306109702391976,-0.9519962447938,-2.22431050430872E-16));
#12109=DIRECTION('',(-0.010034405174207,0.999949654089045,2.3892204885188E-16));
#12110=DIRECTION('center_axis',(1.69724645484627E-17,2.39104395366563E-16,
-1.));
#12111=DIRECTION('ref_axis',(0.306109702391974,-0.9519962447938,-2.22431050430872E-16));
#12112=DIRECTION('',(0.306109702391976,-0.9519962447938,-2.22431050430871E-16));
#12113=DIRECTION('center_axis',(-0.9519962447938,-0.306109702391976,-8.93498978213041E-17));
#12114=DIRECTION('ref_axis',(-1.69724645484627E-17,-2.39104395366563E-16,
1.));
#12115=DIRECTION('',(1.69724645484627E-17,2.39104395366563E-16,-1.));
#12116=DIRECTION('',(0.306109702391976,-0.9519962447938,-2.22431050430871E-16));
#12117=DIRECTION('',(-0.306109702391976,0.9519962447938,2.22431050430871E-16));
#12118=DIRECTION('center_axis',(1.69724645484627E-17,2.39104395366563E-16,
-1.));
#12119=DIRECTION('ref_axis',(0.306109702391976,-0.9519962447938,-2.22431050430871E-16));
#12120=DIRECTION('',(1.69724645484627E-17,2.39104395366563E-16,-1.));
#12121=DIRECTION('center_axis',(-1.69724645484627E-17,-2.39104395366563E-16,
1.));
#12122=DIRECTION('ref_axis',(0.306109702391974,-0.9519962447938,-2.22431050430872E-16));
#12123=DIRECTION('center_axis',(1.69724645484627E-17,2.39104395366563E-16,
-1.));
#12124=DIRECTION('ref_axis',(0.306109702391976,-0.9519962447938,-2.22431050430871E-16));
#12125=DIRECTION('center_axis',(-0.9519962447938,-0.306109702391976,-8.93498978213041E-17));
#12126=DIRECTION('ref_axis',(-1.69724645484627E-17,-2.39104395366563E-16,
1.));
#12127=DIRECTION('',(1.69724645484627E-17,2.39104395366563E-16,-1.));
#12128=DIRECTION('',(0.306109702391976,-0.9519962447938,-2.22431050430871E-16));
#12129=DIRECTION('',(-0.306109702391976,0.9519962447938,2.22431050430871E-16));
#12130=DIRECTION('center_axis',(1.69724645484627E-17,2.39104395366563E-16,
-1.));
#12131=DIRECTION('ref_axis',(-0.306109702391977,0.951996244793799,2.22431050430871E-16));
#12132=DIRECTION('',(1.69724645484627E-17,2.39104395366563E-16,-1.));
#12133=DIRECTION('center_axis',(1.69724645484627E-17,2.39104395366563E-16,
-1.));
#12134=DIRECTION('ref_axis',(0.306109702391974,-0.9519962447938,-2.22431050430872E-16));
#12135=DIRECTION('center_axis',(-1.69724645484627E-17,-2.39104395366563E-16,
1.));
#12136=DIRECTION('ref_axis',(0.306109702391974,-0.9519962447938,-2.22431050430872E-16));
#12137=DIRECTION('center_axis',(0.999949654089045,0.010034405174207,1.93708804363157E-17));
#12138=DIRECTION('ref_axis',(-0.010034405174207,0.999949654089045,2.3892204885188E-16));
#12139=DIRECTION('',(1.69724645484627E-17,2.39104395366563E-16,-1.));
#12140=DIRECTION('',(-0.010034405174207,0.999949654089045,2.3892204885188E-16));
#12141=DIRECTION('',(0.010034405174207,-0.999949654089045,-2.3892204885188E-16));
#12142=DIRECTION('center_axis',(1.69724645484627E-17,2.39104395366563E-16,
-1.));
#12143=DIRECTION('ref_axis',(0.306109702391976,-0.9519962447938,-2.22431050430872E-16));
#12144=DIRECTION('',(1.69724645484627E-17,2.39104395366563E-16,-1.));
#12145=DIRECTION('center_axis',(1.69724645484627E-17,2.39104395366563E-16,
-1.));
#12146=DIRECTION('ref_axis',(0.306109702391976,-0.9519962447938,-2.22431050430872E-16));
#12147=DIRECTION('center_axis',(-1.69724645484627E-17,-2.39104395366563E-16,
1.));
#12148=DIRECTION('ref_axis',(0.306109702391976,-0.9519962447938,-2.22431050430872E-16));
#12149=DIRECTION('center_axis',(1.69724645484627E-17,2.39104395366563E-16,
-1.));
#12150=DIRECTION('ref_axis',(0.306109702391976,-0.9519962447938,-2.22431050430871E-16));
#12151=DIRECTION('center_axis',(-1.69724645484627E-17,-2.39104395366563E-16,
1.));
#12152=DIRECTION('ref_axis',(0.306109702391976,-0.9519962447938,-2.22431050430871E-16));
#12153=DIRECTION('center_axis',(1.69724645484627E-17,2.39104395366563E-16,
-1.));
#12154=DIRECTION('ref_axis',(0.306109702391976,-0.9519962447938,-2.22431050430871E-16));
#12155=DIRECTION('center_axis',(-0.306109702391976,0.9519962447938,2.22431050430871E-16));
#12156=DIRECTION('ref_axis',(-6.80883026501286E-17,2.1175352473573E-16,
-1.));
#12157=DIRECTION('center_axis',(-0.306109702391976,0.9519962447938,2.22431050430871E-16));
#12158=DIRECTION('ref_axis',(-6.80883026501286E-17,2.1175352473573E-16,
-1.));
#12159=DIRECTION('center_axis',(1.69724645484627E-17,2.39104395366563E-16,
-1.));
#12160=DIRECTION('ref_axis',(-0.310393882940736,0.950608035645067,0.));
#12161=DIRECTION('center_axis',(1.69724645484627E-17,2.39104395366563E-16,
-1.));
#12162=DIRECTION('ref_axis',(0.306109702391976,-0.9519962447938,0.));
#12163=DIRECTION('center_axis',(0.010034405174207,-0.999949654089045,-2.3892204885188E-16));
#12164=DIRECTION('ref_axis',(0.999949654089045,0.010034405174207,-2.9722020788518E-30));
#12165=DIRECTION('center_axis',(-0.306109702391976,0.9519962447938,2.22431050430871E-16));
#12166=DIRECTION('ref_axis',(-6.80883026501286E-17,2.1175352473573E-16,
-1.));
#12167=DIRECTION('center_axis',(1.69724645484627E-17,2.39104395366563E-16,
-1.));
#12168=DIRECTION('ref_axis',(0.306109702391976,-0.9519962447938,0.));
#12169=DIRECTION('center_axis',(0.873111609447877,-0.487520376443219,-1.0174940900013E-16));
#12170=DIRECTION('ref_axis',(0.487520376443219,0.873111609447877,1.56063105332704E-30));
#12171=DIRECTION('center_axis',(1.69724645484627E-17,2.39104395366563E-16,
-1.));
#12172=DIRECTION('ref_axis',(0.306109702391975,-0.9519962447938,0.));
#12173=DIRECTION('center_axis',(-0.010034405174207,0.999949654089045,2.3892204885188E-16));
#12174=DIRECTION('ref_axis',(-0.999949654089045,-0.010034405174207,2.9722020788518E-30));
#12175=DIRECTION('center_axis',(1.69724645484627E-17,2.39104395366563E-16,
-1.));
#12176=DIRECTION('ref_axis',(0.306109702391976,-0.9519962447938,0.));
#12177=DIRECTION('center_axis',(0.873111609447875,-0.487520376443223,-1.01749409000131E-16));
#12178=DIRECTION('ref_axis',(0.487520376443223,0.873111609447875,1.07581134523358E-30));
#12179=DIRECTION('center_axis',(1.69724645484627E-17,2.39104395366563E-16,
-1.));
#12180=DIRECTION('ref_axis',(-0.310393882940736,0.950608035645067,0.));
#12181=DIRECTION('center_axis',(0.306109702391976,-0.9519962447938,-2.22431050430871E-16));
#12182=DIRECTION('ref_axis',(6.80883026501286E-17,-2.1175352473573E-16,
1.));
#12183=DIRECTION('center_axis',(1.69724645484627E-17,2.39104395366563E-16,
-1.));
#12184=DIRECTION('ref_axis',(0.306109702391975,-0.9519962447938,0.));
#12185=DIRECTION('center_axis',(0.306109702391976,-0.9519962447938,-2.22431050430871E-16));
#12186=DIRECTION('ref_axis',(6.80883026501286E-17,-2.1175352473573E-16,
1.));
#12187=DIRECTION('center_axis',(1.69724645484627E-17,2.39104395366563E-16,
-1.));
#12188=DIRECTION('ref_axis',(0.306109702391976,-0.9519962447938,0.));
#12189=DIRECTION('center_axis',(0.306109702391976,-0.9519962447938,-2.22431050430871E-16));
#12190=DIRECTION('ref_axis',(6.80883026501286E-17,-2.1175352473573E-16,
1.));
#12191=DIRECTION('',(0.,0.,1.));
#12192=DIRECTION('',(1.,0.,0.));
#12193=DIRECTION('',(0.,0.,1.));
#12194=DIRECTION('',(1.,0.,0.));
#12195=DIRECTION('',(0.,0.,1.));
#12196=DIRECTION('',(1.,0.,0.));
#12197=DIRECTION('',(0.,0.,1.));
#12198=DIRECTION('',(1.,0.,0.));
#12199=DIRECTION('',(0.,0.,1.));
#12200=DIRECTION('',(1.,0.,0.));
#12201=DIRECTION('',(0.,0.,1.));
#12202=DIRECTION('',(1.,0.,0.));
#12203=DIRECTION('',(0.,0.,1.));
#12204=DIRECTION('',(1.,0.,0.));
#12205=DIRECTION('',(0.,0.,1.));
#12206=DIRECTION('',(1.,0.,0.));
#12207=DIRECTION('',(0.,0.,1.));
#12208=DIRECTION('',(1.,0.,0.));
#12209=DIRECTION('',(0.,0.,1.));
#12210=DIRECTION('',(1.,0.,0.));
#12211=DIRECTION('',(0.,0.,1.));
#12212=DIRECTION('',(1.,0.,0.));
#12213=DIRECTION('',(0.,0.,1.));
#12214=DIRECTION('',(1.,0.,0.));
#12215=CARTESIAN_POINT('',(0.,0.,0.));
#12216=CARTESIAN_POINT('',(0.,0.,0.));
#12217=CARTESIAN_POINT('Origin',(-69.9391102914976,14.1820463536523,178.735485069079));
#12218=CARTESIAN_POINT('',(-73.2462994303283,14.1820463536523,180.985485069079));
#12219=CARTESIAN_POINT('Origin',(-69.9391102914976,14.1820463536523,180.985485069079));
#12220=CARTESIAN_POINT('Origin',(-69.9391102914976,14.1820463536523,175.985485069079));
#12221=CARTESIAN_POINT('',(-69.9391102914976,16.1820463536523,180.985485069079));
#12222=CARTESIAN_POINT('Origin',(-69.9391102914976,14.1820463536523,180.985485069079));
#12223=CARTESIAN_POINT('',(-69.9391102914976,16.1820463536523,170.985485069079));
#12224=CARTESIAN_POINT('',(-69.9391102914976,16.1820463536523,175.985485069079));
#12225=CARTESIAN_POINT('Origin',(-69.9391102914976,14.1820463536523,170.985485069079));
#12226=CARTESIAN_POINT('Origin',(-69.9391102914976,14.1820463536523,173.235485069079));
#12227=CARTESIAN_POINT('',(-73.2462994303283,14.1820463536523,170.985485069079));
#12228=CARTESIAN_POINT('Origin',(-69.9391102914976,14.1820463536523,170.985485069079));
#12229=CARTESIAN_POINT('Origin',(-67.9391102914976,14.1820463536523,170.985485069079));
#12230=CARTESIAN_POINT('Origin',(-67.9391102914976,14.1820463536523,180.985485069079));
#12231=CARTESIAN_POINT('',(0.,0.,0.));
#12232=CARTESIAN_POINT('Origin',(-54.1881478197433,0.967499828069326,177.985485069079));
#12233=CARTESIAN_POINT('',(-54.4457518203465,2.3033512062679,177.143379805922));
#12234=CARTESIAN_POINT('',(-54.5745538206481,2.97127689536718,176.722327174343));
#12235=CARTESIAN_POINT('Origin',(-54.5101528204973,2.63731405081754,176.932853490132));
#12236=CARTESIAN_POINT('Origin',(-54.5101528204973,2.63731405081754,176.932853490132));
#12237=CARTESIAN_POINT('',(-54.1881478197433,0.967499828069329,176.385485069079));
#12238=CARTESIAN_POINT('Origin',(-54.1881478197433,0.967499828069326,177.985485069079));
#12239=CARTESIAN_POINT('',(-54.5809116610057,0.891759713223694,175.985485069079));
#12240=CARTESIAN_POINT('Origin',(-54.1881478197433,0.967499828069329,175.985485069079));
#12241=CARTESIAN_POINT('Origin',(-54.1881478197433,0.967499828069329,175.985485069079));
#12242=CARTESIAN_POINT('Origin',(-47.8413342697331,-31.9450310646891,173.985485069079));
#12243=CARTESIAN_POINT('',(-47.8413342697331,-31.9450310646891,175.585485069079));
#12244=CARTESIAN_POINT('Origin',(-47.8413342697331,-31.9450310646891,175.985485069079));
#12245=CARTESIAN_POINT('',(-47.5837302691299,-33.2808824428876,174.827590332237));
#12246=CARTESIAN_POINT('Origin',(-47.8413342697331,-31.9450310646891,173.985485069079));
#12247=CARTESIAN_POINT('',(-47.4549282688283,-33.9488081319869,175.248642963816));
#12248=CARTESIAN_POINT('Origin',(-47.5193292689791,-33.6148452874373,175.038116648027));
#12249=CARTESIAN_POINT('Origin',(-47.5193292689791,-33.6148452874373,175.038116648027));
#12250=CARTESIAN_POINT('Origin',(-47.2295247683005,-35.1176780879106,175.985485069079));
#12251=CARTESIAN_POINT('',(-47.4169719891537,-34.1456371734454,176.975434562741));
#12252=CARTESIAN_POINT('Origin',(-47.2295247683005,-35.1176780879106,175.985485069079));
#12253=CARTESIAN_POINT('Origin',(-47.4705283379689,-33.8679111978839,177.258277275215));
#12254=CARTESIAN_POINT('Origin',(-54.7999573211759,4.14014685129092,175.985485069079));
#12255=CARTESIAN_POINT('',(-54.6125101003227,3.16810593682568,174.995535575418));
#12256=CARTESIAN_POINT('Origin',(-54.5589537515075,2.89037996126418,174.712692862944));
#12257=CARTESIAN_POINT('Origin',(-54.7999573211759,4.14014685129092,175.985485069079));
#12258=CARTESIAN_POINT('Origin',(-54.1408102479648,0.722022427280349,175.985485069079));
#12259=CARTESIAN_POINT('',(-54.5335740892272,0.646282312434711,175.985485069079));
#12260=CARTESIAN_POINT('',(-54.5335740892272,0.646282312434712,175.985485069079));
#12261=CARTESIAN_POINT('',(-54.2726708967805,0.696594575640996,176.362269083675));
#12262=CARTESIAN_POINT('Origin',(-54.1408102479648,0.722022427280349,175.985485069079));
#12263=CARTESIAN_POINT('',(-54.0089495991491,0.747450278919701,175.608701054484));
#12264=CARTESIAN_POINT('Origin',(-54.1408102479648,0.722022427280349,175.985485069079));
#12265=CARTESIAN_POINT('Origin',(-54.1408102479648,0.722022427280349,175.985485069079));
#12266=CARTESIAN_POINT('Ctrl Pts',(-55.1161897096451,-2.27071607222657,
177.448351373365));
#12267=CARTESIAN_POINT('Ctrl Pts',(-55.0544324803005,-2.24407445661358,
177.516574922684));
#12268=CARTESIAN_POINT('Ctrl Pts',(-55.0031840696463,-2.2159075942787,177.564829510218));
#12269=CARTESIAN_POINT('Ctrl Pts',(-54.8981614763103,-2.14735807337978,
177.649345866972));
#12270=CARTESIAN_POINT('Ctrl Pts',(-54.848196955649,-2.10845499517373,177.68122338125));
#12271=CARTESIAN_POINT('Ctrl Pts',(-54.7062455015458,-1.97869616397794,
177.747598981208));
#12272=CARTESIAN_POINT('Ctrl Pts',(-54.6230552819493,-1.87505607340526,
177.751980177594));
#12273=CARTESIAN_POINT('Ctrl Pts',(-54.4781164600507,-1.64599936204779,
177.704020550018));
#12274=CARTESIAN_POINT('Ctrl Pts',(-54.4161687409529,-1.52036398038793,
177.652507519121));
#12275=CARTESIAN_POINT('Ctrl Pts',(-54.3240884061122,-1.31623292778147,
177.552502738263));
#12276=CARTESIAN_POINT('Ctrl Pts',(-54.2900300114527,-1.2450809441322,177.5168693343));
#12277=CARTESIAN_POINT('Ctrl Pts',(-54.2388806708887,-1.10092476185966,
177.429650782512));
#12278=CARTESIAN_POINT('Ctrl Pts',(-54.2230625419579,-1.02814126447079,
177.378422455576));
#12279=CARTESIAN_POINT('Ctrl Pts',(-54.1687570862725,-0.661100958902222,
177.107656526019));
#12280=CARTESIAN_POINT('Ctrl Pts',(-54.1632550913909,-0.344986943697024,
176.855601626641));
#12281=CARTESIAN_POINT('Ctrl Pts',(-54.1894883174704,0.100428951784895,
176.57062132681));
#12282=CARTESIAN_POINT('Ctrl Pts',(-54.2038650968969,0.243821813285216,
176.491645489995));
#12283=CARTESIAN_POINT('Ctrl Pts',(-54.2289503028814,0.435912884592043,
176.413053638658));
#12284=CARTESIAN_POINT('Ctrl Pts',(-54.2378694870404,0.495988408430007,
176.393461416067));
#12285=CARTESIAN_POINT('Ctrl Pts',(-54.2511575637744,0.57777536525398,176.374426535183));
#12286=CARTESIAN_POINT('Ctrl Pts',(-54.2555861991508,0.603644576350343,
176.369782059628));
#12287=CARTESIAN_POINT('Ctrl Pts',(-54.2642818917577,0.652365455860021,
176.363705099944));
#12288=CARTESIAN_POINT('Ctrl Pts',(-54.2669281652524,0.666814619551347,
176.362269083675));
#12289=CARTESIAN_POINT('Ctrl Pts',(-54.2726708967805,0.696594575640996,
176.362269083675));
#12290=CARTESIAN_POINT('Ctrl Pts',(-54.9611536226478,-1.61438316700751,
177.018013216499));
#12291=CARTESIAN_POINT('Ctrl Pts',(-54.9292844549615,-1.59689979741686,
177.061501366048));
#12292=CARTESIAN_POINT('Ctrl Pts',(-54.9347169869457,-1.59513306644644,
177.059466012753));
#12293=CARTESIAN_POINT('Ctrl Pts',(-54.9393829236175,-1.59207559169288,
177.070205982371));
#12294=CARTESIAN_POINT('Ctrl Pts',(-54.9521671405265,-1.59794122115585,
177.067981920184));
#12295=CARTESIAN_POINT('Ctrl Pts',(-55.0007420885566,-1.63157855374127,
177.067321317852));
#12296=CARTESIAN_POINT('Ctrl Pts',(-55.035179086296,-1.66960295600012,177.085015349648));
#12297=CARTESIAN_POINT('Ctrl Pts',(-55.0396054390644,-1.63669166623166,
177.119603765033));
#12298=CARTESIAN_POINT('Ctrl Pts',(-55.0210115508064,-1.57122240422777,
177.125346825549));
#12299=CARTESIAN_POINT('Ctrl Pts',(-54.9916258301057,-1.40601129473046,
177.119012727072));
#12300=CARTESIAN_POINT('Ctrl Pts',(-54.9808143890584,-1.33515491542406,
177.122292216748));
#12301=CARTESIAN_POINT('Ctrl Pts',(-54.95716312305,-1.20146912437994,177.090609934045));
#12302=CARTESIAN_POINT('Ctrl Pts',(-54.9459301778233,-1.14025139494389,
177.054154311007));
#12303=CARTESIAN_POINT('Ctrl Pts',(-54.9010485418089,-0.837221085805294,
176.830475957374));
#12304=CARTESIAN_POINT('Ctrl Pts',(-54.8933924651384,-0.543523047070829,
176.59567568837));
#12305=CARTESIAN_POINT('Ctrl Pts',(-54.9188659939004,-0.109419407590943,
176.317655840143));
#12306=CARTESIAN_POINT('Ctrl Pts',(-54.9330773739472,0.0346181647599921,
176.23753447689));
#12307=CARTESIAN_POINT('Ctrl Pts',(-54.9598081399055,0.239682185419695,
176.153510553493));
#12308=CARTESIAN_POINT('Ctrl Pts',(-54.9696067027056,0.306181698359097,
176.131488679163));
#12309=CARTESIAN_POINT('Ctrl Pts',(-54.985167831776,0.402075433542801,176.109129772912));
#12310=CARTESIAN_POINT('Ctrl Pts',(-54.9905018003277,0.433390482627809,
176.103410426781));
#12311=CARTESIAN_POINT('Ctrl Pts',(-55.0013966992521,0.494658609580997,
176.095691012754));
#12312=CARTESIAN_POINT('Ctrl Pts',(-55.0061011366799,0.520171112552638,
176.093689066957));
#12313=CARTESIAN_POINT('Ctrl Pts',(-55.012606581275,0.553906252953576,176.093689066957));
#12314=CARTESIAN_POINT('Ctrl Pts',(-54.3738267566562,-2.00237092626598,
176.637865020199));
#12315=CARTESIAN_POINT('Ctrl Pts',(-54.3525463517218,-1.98561856641678,
176.665739674622));
#12316=CARTESIAN_POINT('Ctrl Pts',(-54.3544769039845,-1.9794317280201,176.664843524849));
#12317=CARTESIAN_POINT('Ctrl Pts',(-54.3701639946021,-1.97656111293176,
176.660021126843));
#12318=CARTESIAN_POINT('Ctrl Pts',(-54.3898340629218,-1.98406009722412,
176.649873028566));
#12319=CARTESIAN_POINT('Ctrl Pts',(-54.4615150878692,-2.02680400188237,
176.627416363355));
#12320=CARTESIAN_POINT('Ctrl Pts',(-54.5129888400511,-2.0757703324506,176.634526145744));
#12321=CARTESIAN_POINT('Ctrl Pts',(-54.5552784049148,-2.06122690211322,
176.64442773024));
#12322=CARTESIAN_POINT('Ctrl Pts',(-54.5578076149692,-2.0038135240127,176.634785085717));
#12323=CARTESIAN_POINT('Ctrl Pts',(-54.5892177302657,-1.85411233048761,
176.591889300217));
#12324=CARTESIAN_POINT('Ctrl Pts',(-54.610530702465,-1.78996529622254,176.577740776828));
#12325=CARTESIAN_POINT('Ctrl Pts',(-54.6268123436843,-1.66507238716025,
176.528080652247));
#12326=CARTESIAN_POINT('Ctrl Pts',(-54.6208424301061,-1.60549754243094,
176.490359176158));
#12327=CARTESIAN_POINT('Ctrl Pts',(-54.5752745689856,-1.29850461246565,
176.263815183543));
#12328=CARTESIAN_POINT('Ctrl Pts',(-54.5643152196599,-0.983878310891091,
176.010083812441));
#12329=CARTESIAN_POINT('Ctrl Pts',(-54.5948528025329,-0.459382509277473,
175.674365954678));
#12330=CARTESIAN_POINT('Ctrl Pts',(-54.6123879900288,-0.274694122222572,
175.56925971577));
#12331=CARTESIAN_POINT('Ctrl Pts',(-54.6518354905867,0.0289042342998165,
175.444989413561));
#12332=CARTESIAN_POINT('Ctrl Pts',(-54.6672255747517,0.134792609497288,
175.409177545969));
#12333=CARTESIAN_POINT('Ctrl Pts',(-54.6945480274656,0.303452837912914,
175.369907772329));
#12334=CARTESIAN_POINT('Ctrl Pts',(-54.7043366789371,0.361315642399545,
175.359237745269));
#12335=CARTESIAN_POINT('Ctrl Pts',(-54.7254408307236,0.480524258303587,
175.344341053851));
#12336=CARTESIAN_POINT('Ctrl Pts',(-54.7391421008419,0.554236948300629,
175.340121037765));
#12337=CARTESIAN_POINT('Ctrl Pts',(-54.7488852836436,0.604761956232279,
175.340121037765));
#12338=CARTESIAN_POINT('Ctrl Pts',(-54.5288628436534,-2.65870383148503,
177.068203177065));
#12339=CARTESIAN_POINT('Ctrl Pts',(-54.4776943770608,-2.6327932256135,177.120813231257));
#12340=CARTESIAN_POINT('Ctrl Pts',(-54.4229439866851,-2.60020625585236,
177.170207022314));
#12341=CARTESIAN_POINT('Ctrl Pts',(-54.3289425472948,-2.53184359461866,
177.239161011444));
#12342=CARTESIAN_POINT('Ctrl Pts',(-54.2858638780443,-2.494573871242,177.263114489632));
#12343=CARTESIAN_POINT('Ctrl Pts',(-54.1670185008584,-2.37392161211904,
177.307694026711));
#12344=CARTESIAN_POINT('Ctrl Pts',(-54.1008650357044,-2.28122344985573,
177.30149097369));
#12345=CARTESIAN_POINT('Ctrl Pts',(-53.9937894259011,-2.07053459792936,
177.228844515225));
#12346=CARTESIAN_POINT('Ctrl Pts',(-53.9529648051158,-1.95295510017287,
177.161945779289));
#12347=CARTESIAN_POINT('Ctrl Pts',(-53.9216803062721,-1.76433396353862,
177.025379311408));
#12348=CARTESIAN_POINT('Ctrl Pts',(-53.9197463248593,-1.6998913249307,176.97231789438));
#12349=CARTESIAN_POINT('Ctrl Pts',(-53.9085298915231,-1.56452802463996,
176.867121500714));
#12350=CARTESIAN_POINT('Ctrl Pts',(-53.8979747942407,-1.4933874119578,176.814627320727));
#12351=CARTESIAN_POINT('Ctrl Pts',(-53.8429831134493,-1.12238448556273,
176.540995752188));
#12352=CARTESIAN_POINT('Ctrl Pts',(-53.8341778459125,-0.785342207517119,
176.270009750712));
#12353=CARTESIAN_POINT('Ctrl Pts',(-53.8654751261029,-0.249534149901716,
175.927331441344));
#12354=CARTESIAN_POINT('Ctrl Pts',(-53.8831757129786,-0.0654904736973553,
175.823370728875));
#12355=CARTESIAN_POINT('Ctrl Pts',(-53.9209776535626,0.225134933472168,
175.704532498726));
#12356=CARTESIAN_POINT('Ctrl Pts',(-53.9354883590865,0.324599319568198,
175.671150282872));
#12357=CARTESIAN_POINT('Ctrl Pts',(-53.960537759464,0.479152769624093,175.6352045346));
#12358=CARTESIAN_POINT('Ctrl Pts',(-53.9694210777602,0.531569736122078,
175.625609378116));
#12359=CARTESIAN_POINT('Ctrl Pts',(-53.9883260232292,0.638231104582612,
175.612355141042));
#12360=CARTESIAN_POINT('Ctrl Pts',(-53.9999691294144,0.700880455299337,
175.608701054484));
#12361=CARTESIAN_POINT('Ctrl Pts',(-54.0089495991491,0.747450278919698,
175.608701054484));
#12362=CARTESIAN_POINT('Ctrl Pts',(-54.6838989306507,-3.31503673670408,
177.498541333932));
#12363=CARTESIAN_POINT('Ctrl Pts',(-54.6028424023999,-3.27996788481022,
177.575886787893));
#12364=CARTESIAN_POINT('Ctrl Pts',(-54.4914110693857,-3.22098078368462,
177.675570519779));
#12365=CARTESIAN_POINT('Ctrl Pts',(-54.2877210999876,-3.08712607630556,
177.818300896045));
#12366=CARTESIAN_POINT('Ctrl Pts',(-54.1818936931668,-3.00508764525988,
177.876355950698));
#12367=CARTESIAN_POINT('Ctrl Pts',(-53.8725219138475,-2.7210392223557,177.987971690067));
#12368=CARTESIAN_POINT('Ctrl Pts',(-53.6887412313577,-2.48667656726087,
177.968455801636));
#12369=CARTESIAN_POINT('Ctrl Pts',(-53.4323004468874,-2.07984229374549,
177.81326130021));
#12370=CARTESIAN_POINT('Ctrl Pts',(-53.3481219952623,-1.90209667633303,
177.689106472861));
#12371=CARTESIAN_POINT('Ctrl Pts',(-53.2541428822785,-1.67455559658963,
177.4588693226));
#12372=CARTESIAN_POINT('Ctrl Pts',(-53.2289619472537,-1.60981735363885,
177.366895011932));
#12373=CARTESIAN_POINT('Ctrl Pts',(-53.1902474393619,-1.46398366211967,
177.206162349181));
#12374=CARTESIAN_POINT('Ctrl Pts',(-53.1751071583752,-1.38127728148465,
177.138895465296));
#12375=CARTESIAN_POINT('Ctrl Pts',(-53.1106916579129,-0.946264358659819,
176.818176320833));
#12376=CARTESIAN_POINT('Ctrl Pts',(-53.104040472165,-0.586806104143147,
176.529935688984));
#12377=CARTESIAN_POINT('Ctrl Pts',(-53.1360974496729,-0.0396857905259603,
176.18029692801));
#12378=CARTESIAN_POINT('Ctrl Pts',(-53.1539634359283,0.143713174827862,
176.077481741979));
#12379=CARTESIAN_POINT('Ctrl Pts',(-53.1901198165385,0.421365632644519,
175.964075583891));
#12380=CARTESIAN_POINT('Ctrl Pts',(-53.2037511434212,0.514406029639107,
175.933123019776));
#12381=CARTESIAN_POINT('Ctrl Pts',(-53.2265274914624,0.654852701335273,
175.900501296871));
#12382=CARTESIAN_POINT('Ctrl Pts',(-53.2345054765832,0.701823829844612,
175.891981010963));
#12383=CARTESIAN_POINT('Ctrl Pts',(-53.2512112157347,0.795937950861637,
175.880369228233));
#12384=CARTESIAN_POINT('Ctrl Pts',(-53.2607961579869,0.847523962298047,
175.877281071202));
#12385=CARTESIAN_POINT('Ctrl Pts',(-53.2690139146546,0.890138601607118,
175.877281071202));
#12386=CARTESIAN_POINT('Ctrl Pts',(-55.2712257966423,-2.92704897744562,
177.878689530232));
#12387=CARTESIAN_POINT('Ctrl Pts',(-55.1795805056396,-2.8912491158103,177.971648479319));
#12388=CARTESIAN_POINT('Ctrl Pts',(-55.071651152347,-2.83668212211097,178.070193007683));
#12389=CARTESIAN_POINT('Ctrl Pts',(-54.8569400290031,-2.70264055506668,
178.228485751573));
#12390=CARTESIAN_POINT('Ctrl Pts',(-54.7442267707714,-2.61896876919161,
178.294464842316));
#12391=CARTESIAN_POINT('Ctrl Pts',(-54.411748914535,-2.3258137742146,178.427876644564));
#12392=CARTESIAN_POINT('Ctrl Pts',(-54.2109314776027,-2.08050919081039,
178.41894500554));
#12393=CARTESIAN_POINT('Ctrl Pts',(-53.916627481037,-1.65530705786393,178.288437335003));
#12394=CARTESIAN_POINT('Ctrl Pts',(-53.8113259310995,-1.4695055565481,178.179668212693));
#12395=CARTESIAN_POINT('Ctrl Pts',(-53.6565509821185,-1.22645456083248,
177.985992749455));
#12396=CARTESIAN_POINT('Ctrl Pts',(-53.5992456338471,-1.15500697284035,
177.911446451852));
#12397=CARTESIAN_POINT('Ctrl Pts',(-53.5205982187275,-1.00038039933938,
177.768691630978));
#12398=CARTESIAN_POINT('Ctrl Pts',(-53.5001949060925,-0.916031133997679,
177.702690600146));
#12399=CARTESIAN_POINT('Ctrl Pts',(-53.4364656307362,-0.484980831999149,
177.384837094664));
#12400=CARTESIAN_POINT('Ctrl Pts',(-53.4331177176434,-0.146450840323217,
177.115527564913));
#12401=CARTESIAN_POINT('Ctrl Pts',(-53.4601106410404,0.310277311160734,
176.823586813476));
#12402=CARTESIAN_POINT('Ctrl Pts',(-53.4746528198466,0.453025461810439,
176.745756503099));
#12403=CARTESIAN_POINT('Ctrl Pts',(-53.4980924658573,0.632143583764391,
176.672596723823));
#12404=CARTESIAN_POINT('Ctrl Pts',(-53.5061322713752,0.685795118500917,
176.65543415297));
#12405=CARTESIAN_POINT('Ctrl Pts',(-53.5171472957729,0.75347529696516,176.639723297454));
#12406=CARTESIAN_POINT('Ctrl Pts',(-53.5206705979738,0.773898670072877,
176.636153692475));
#12407=CARTESIAN_POINT('Ctrl Pts',(-53.5271670842632,0.810072302139046,
176.631719187135));
#12408=CARTESIAN_POINT('Ctrl Pts',(-53.5277551938249,0.813458126550056,
176.630849100393));
#12409=CARTESIAN_POINT('Ctrl Pts',(-53.532735212286,0.839282898328416,176.630849100393));
#12410=CARTESIAN_POINT('Ctrl Pts',(-55.1161897096451,-2.27071607222657,
177.448351373365));
#12411=CARTESIAN_POINT('Ctrl Pts',(-55.0544324803005,-2.24407445661358,
177.516574922684));
#12412=CARTESIAN_POINT('Ctrl Pts',(-55.0031840696463,-2.2159075942787,177.564829510218));
#12413=CARTESIAN_POINT('Ctrl Pts',(-54.8981614763103,-2.14735807337978,
177.649345866972));
#12414=CARTESIAN_POINT('Ctrl Pts',(-54.848196955649,-2.10845499517373,177.68122338125));
#12415=CARTESIAN_POINT('Ctrl Pts',(-54.7062455015458,-1.97869616397794,
177.747598981208));
#12416=CARTESIAN_POINT('Ctrl Pts',(-54.6230552819493,-1.87505607340526,
177.751980177594));
#12417=CARTESIAN_POINT('Ctrl Pts',(-54.4781164600507,-1.64599936204779,
177.704020550018));
#12418=CARTESIAN_POINT('Ctrl Pts',(-54.4161687409529,-1.52036398038793,
177.652507519121));
#12419=CARTESIAN_POINT('Ctrl Pts',(-54.3240884061122,-1.31623292778147,
177.552502738263));
#12420=CARTESIAN_POINT('Ctrl Pts',(-54.2900300114527,-1.2450809441322,177.5168693343));
#12421=CARTESIAN_POINT('Ctrl Pts',(-54.2388806708887,-1.10092476185966,
177.429650782512));
#12422=CARTESIAN_POINT('Ctrl Pts',(-54.2230625419579,-1.02814126447079,
177.378422455576));
#12423=CARTESIAN_POINT('Ctrl Pts',(-54.1687570862725,-0.661100958902222,
177.107656526019));
#12424=CARTESIAN_POINT('Ctrl Pts',(-54.1632550913909,-0.344986943697024,
176.855601626641));
#12425=CARTESIAN_POINT('Ctrl Pts',(-54.1894883174704,0.100428951784895,
176.57062132681));
#12426=CARTESIAN_POINT('Ctrl Pts',(-54.2038650968969,0.243821813285216,
176.491645489995));
#12427=CARTESIAN_POINT('Ctrl Pts',(-54.2289503028814,0.435912884592043,
176.413053638658));
#12428=CARTESIAN_POINT('Ctrl Pts',(-54.2378694870404,0.495988408430007,
176.393461416067));
#12429=CARTESIAN_POINT('Ctrl Pts',(-54.2511575637744,0.57777536525398,176.374426535183));
#12430=CARTESIAN_POINT('Ctrl Pts',(-54.2555861991508,0.603644576350343,
176.369782059628));
#12431=CARTESIAN_POINT('Ctrl Pts',(-54.2642818917577,0.652365455860021,
176.363705099944));
#12432=CARTESIAN_POINT('Ctrl Pts',(-54.2669281652524,0.666814619551347,
176.362269083675));
#12433=CARTESIAN_POINT('Ctrl Pts',(-54.2726708967805,0.696594575640996,
176.362269083675));
#12434=CARTESIAN_POINT('',(-54.5288628436534,-2.65870383148502,177.068203177065));
#12435=CARTESIAN_POINT('',(-55.1161897096451,-2.27071607222657,177.448351373365));
#12436=CARTESIAN_POINT('Origin',(-54.8225262766493,-2.4647099518558,177.258277275215));
#12437=CARTESIAN_POINT('Ctrl Pts',(-54.5288628436534,-2.65870383148502,
177.068203177065));
#12438=CARTESIAN_POINT('Ctrl Pts',(-54.4776943770608,-2.6327932256135,177.120813231257));
#12439=CARTESIAN_POINT('Ctrl Pts',(-54.4229439866851,-2.60020625585236,
177.170207022314));
#12440=CARTESIAN_POINT('Ctrl Pts',(-54.3289425472948,-2.53184359461866,
177.239161011444));
#12441=CARTESIAN_POINT('Ctrl Pts',(-54.2858638780443,-2.494573871242,177.263114489632));
#12442=CARTESIAN_POINT('Ctrl Pts',(-54.1670185008584,-2.37392161211904,
177.307694026711));
#12443=CARTESIAN_POINT('Ctrl Pts',(-54.1008650357044,-2.28122344985573,
177.30149097369));
#12444=CARTESIAN_POINT('Ctrl Pts',(-53.9937894259011,-2.07053459792936,
177.228844515225));
#12445=CARTESIAN_POINT('Ctrl Pts',(-53.9529648051158,-1.95295510017287,
177.161945779289));
#12446=CARTESIAN_POINT('Ctrl Pts',(-53.9216803062721,-1.76433396353862,
177.025379311408));
#12447=CARTESIAN_POINT('Ctrl Pts',(-53.9197463248593,-1.6998913249307,176.97231789438));
#12448=CARTESIAN_POINT('Ctrl Pts',(-53.9085298915231,-1.56452802463996,
176.867121500714));
#12449=CARTESIAN_POINT('Ctrl Pts',(-53.8979747942407,-1.4933874119578,176.814627320727));
#12450=CARTESIAN_POINT('Ctrl Pts',(-53.8429831134493,-1.12238448556273,
176.540995752188));
#12451=CARTESIAN_POINT('Ctrl Pts',(-53.8341778459125,-0.785342207517119,
176.270009750712));
#12452=CARTESIAN_POINT('Ctrl Pts',(-53.8654751261029,-0.249534149901716,
175.927331441344));
#12453=CARTESIAN_POINT('Ctrl Pts',(-53.8831757129786,-0.0654904736973553,
175.823370728875));
#12454=CARTESIAN_POINT('Ctrl Pts',(-53.9209776535626,0.225134933472168,
175.704532498726));
#12455=CARTESIAN_POINT('Ctrl Pts',(-53.9354883590865,0.324599319568198,
175.671150282872));
#12456=CARTESIAN_POINT('Ctrl Pts',(-53.960537759464,0.479152769624093,175.6352045346));
#12457=CARTESIAN_POINT('Ctrl Pts',(-53.9694210777602,0.531569736122078,
175.625609378116));
#12458=CARTESIAN_POINT('Ctrl Pts',(-53.9883260232292,0.638231104582612,
175.612355141042));
#12459=CARTESIAN_POINT('Ctrl Pts',(-53.9999691294144,0.700880455299337,
175.608701054484));
#12460=CARTESIAN_POINT('Ctrl Pts',(-54.0089495991491,0.747450278919701,
175.608701054484));
#12461=CARTESIAN_POINT('Ctrl Pts',(-55.1161897096451,-2.27071607222657,
177.448351373365));
#12462=CARTESIAN_POINT('Ctrl Pts',(-55.0544324803005,-2.24407445661358,
177.516574922684));
#12463=CARTESIAN_POINT('Ctrl Pts',(-55.0031840696463,-2.2159075942787,177.564829510218));
#12464=CARTESIAN_POINT('Ctrl Pts',(-54.8981614763103,-2.14735807337978,
177.649345866972));
#12465=CARTESIAN_POINT('Ctrl Pts',(-54.848196955649,-2.10845499517373,177.68122338125));
#12466=CARTESIAN_POINT('Ctrl Pts',(-54.7062455015458,-1.97869616397794,
177.747598981208));
#12467=CARTESIAN_POINT('Ctrl Pts',(-54.6230552819493,-1.87505607340526,
177.751980177594));
#12468=CARTESIAN_POINT('Ctrl Pts',(-54.4781164600507,-1.64599936204779,
177.704020550018));
#12469=CARTESIAN_POINT('Ctrl Pts',(-54.4161687409529,-1.52036398038793,
177.652507519121));
#12470=CARTESIAN_POINT('Ctrl Pts',(-54.3240884061122,-1.31623292778147,
177.552502738263));
#12471=CARTESIAN_POINT('Ctrl Pts',(-54.2900300114527,-1.2450809441322,177.5168693343));
#12472=CARTESIAN_POINT('Ctrl Pts',(-54.2388806708887,-1.10092476185966,
177.429650782512));
#12473=CARTESIAN_POINT('Ctrl Pts',(-54.2230625419579,-1.02814126447079,
177.378422455576));
#12474=CARTESIAN_POINT('Ctrl Pts',(-54.1687570862725,-0.661100958902222,
177.107656526019));
#12475=CARTESIAN_POINT('Ctrl Pts',(-54.1632550913909,-0.344986943697024,
176.855601626641));
#12476=CARTESIAN_POINT('Ctrl Pts',(-54.1894883174704,0.100428951784895,
176.57062132681));
#12477=CARTESIAN_POINT('Ctrl Pts',(-54.2038650968969,0.243821813285216,
176.491645489995));
#12478=CARTESIAN_POINT('Ctrl Pts',(-54.2289503028814,0.435912884592043,
176.413053638658));
#12479=CARTESIAN_POINT('Ctrl Pts',(-54.2378694870404,0.495988408430007,
176.393461416067));
#12480=CARTESIAN_POINT('Ctrl Pts',(-54.2511575637744,0.57777536525398,176.374426535183));
#12481=CARTESIAN_POINT('Ctrl Pts',(-54.2555861991508,0.603644576350343,
176.369782059628));
#12482=CARTESIAN_POINT('Ctrl Pts',(-54.2642818917577,0.652365455860021,
176.363705099944));
#12483=CARTESIAN_POINT('Ctrl Pts',(-54.2669281652524,0.666814619551347,
176.362269083675));
#12484=CARTESIAN_POINT('Ctrl Pts',(-54.2726708967805,0.696594575640996,
176.362269083675));
#12485=CARTESIAN_POINT('Ctrl Pts',(-50.193114320713,-27.8005016688432,177.448440461337));
#12486=CARTESIAN_POINT('Ctrl Pts',(-50.1356777281885,-27.7780416249781,
177.514251363723));
#12487=CARTESIAN_POINT('Ctrl Pts',(-50.0768656935625,-27.751543311514,177.569181845458));
#12488=CARTESIAN_POINT('Ctrl Pts',(-49.9502510673185,-27.7006718917524,
177.678131488152));
#12489=CARTESIAN_POINT('Ctrl Pts',(-49.8836384545372,-27.6746069642733,
177.728584647058));
#12490=CARTESIAN_POINT('Ctrl Pts',(-49.6751767137455,-27.5945945456976,
177.866776279515));
#12491=CARTESIAN_POINT('Ctrl Pts',(-49.5241175159801,-27.5384622401806,
177.941191651987));
#12492=CARTESIAN_POINT('Ctrl Pts',(-49.052722448706,-27.3677108924734,178.102046365205));
#12493=CARTESIAN_POINT('Ctrl Pts',(-48.713006227557,-27.2491092781452,178.126053652285));
#12494=CARTESIAN_POINT('Ctrl Pts',(-47.7382795874562,-26.9019657740439,
177.942209528285));
#12495=CARTESIAN_POINT('Ctrl Pts',(-47.1597470877608,-26.6842880122364,
177.461567693823));
#12496=CARTESIAN_POINT('Ctrl Pts',(-46.658904710499,-26.3725604903201,176.179580952166));
#12497=CARTESIAN_POINT('Ctrl Pts',(-46.744016732095,-26.2835354545934,175.410971277798));
#12498=CARTESIAN_POINT('Ctrl Pts',(-47.5354179070377,-26.2224078706935,
174.242909311213));
#12499=CARTESIAN_POINT('Ctrl Pts',(-48.2245449656354,-26.2493771368743,
173.87343933243));
#12500=CARTESIAN_POINT('Ctrl Pts',(-49.6317089464608,-26.3060463238627,
173.871895146128));
#12501=CARTESIAN_POINT('Ctrl Pts',(-50.3230600395606,-26.332977077053,174.238655026377));
#12502=CARTESIAN_POINT('Ctrl Pts',(-51.1153496063116,-26.2743348509258,
175.387691644257));
#12503=CARTESIAN_POINT('Ctrl Pts',(-51.2096393582444,-26.1855070701005,
176.164686974611));
#12504=CARTESIAN_POINT('Ctrl Pts',(-50.7213268039385,-25.8775623946772,
177.442968877094));
#12505=CARTESIAN_POINT('Ctrl Pts',(-50.1473617008829,-25.6602454668112,
177.932812658479));
#12506=CARTESIAN_POINT('Ctrl Pts',(-48.8451246534299,-25.1962898596545,
178.190564242377));
#12507=CARTESIAN_POINT('Ctrl Pts',(-48.1356293396501,-24.9529458243571,
177.955714348281));
#12508=CARTESIAN_POINT('Ctrl Pts',(-47.2268076672755,-24.5631416907191,
176.954286183848));
#12509=CARTESIAN_POINT('Ctrl Pts',(-47.0395646158613,-24.4209960169422,
176.20954077848));
#12510=CARTESIAN_POINT('Ctrl Pts',(-47.370313215787,-24.2726666068476,174.855768290097));
#12511=CARTESIAN_POINT('Ctrl Pts',(-47.8845545017147,-24.265674947158,174.26583855031));
#12512=CARTESIAN_POINT('Ctrl Pts',(-49.1994460468846,-24.3046603227726,
173.764180115318));
#12513=CARTESIAN_POINT('Ctrl Pts',(-49.9762257647407,-24.3480555327739,
173.861039734223));
#12514=CARTESIAN_POINT('Ctrl Pts',(-51.1285193941288,-24.3574791486806,
174.66646218052));
#12515=CARTESIAN_POINT('Ctrl Pts',(-51.4882290443068,-24.3203491702665,
175.364132112564));
#12516=CARTESIAN_POINT('Ctrl Pts',(-51.4777341832408,-24.1036300286494,
176.755680066459));
#12517=CARTESIAN_POINT('Ctrl Pts',(-51.1141102527119,-23.9275319100486,
177.423612084264));
#12518=CARTESIAN_POINT('Ctrl Pts',(-49.9940329966114,-23.4994535030053,
178.148719290634));
#12519=CARTESIAN_POINT('Ctrl Pts',(-49.2531996565364,-23.2503850964097,
178.195074921104));
#12520=CARTESIAN_POINT('Ctrl Pts',(-48.0540724826088,-22.804580182732,177.607487959387));
#12521=CARTESIAN_POINT('Ctrl Pts',(-47.6174629086983,-22.6140260251447,
176.985139741962));
#12522=CARTESIAN_POINT('Ctrl Pts',(-47.4549919432363,-22.3698803060775,
175.609945370482));
#12523=CARTESIAN_POINT('Ctrl Pts',(-47.7329522193418,-22.3169255939418,
174.876470615888));
#12524=CARTESIAN_POINT('Ctrl Pts',(-48.8440385240951,-22.3059754149369,
173.902867041218));
#12525=CARTESIAN_POINT('Ctrl Pts',(-49.7035599970344,-22.3554674780819,
173.739637329099));
#12526=CARTESIAN_POINT('Ctrl Pts',(-51.1531706356154,-22.4011313967338,
174.265066374312));
#12527=CARTESIAN_POINT('Ctrl Pts',(-51.7115054154064,-22.3910761212842,
174.945624054023));
#12528=CARTESIAN_POINT('Ctrl Pts',(-51.9563259347572,-22.2045289991918,
176.459132103654));
#12529=CARTESIAN_POINT('Ctrl Pts',(-51.63765119649,-22.0251559400258,177.262331468575));
#12530=CARTESIAN_POINT('Ctrl Pts',(-50.4571461815608,-21.5627984935069,
178.149907937338));
#12531=CARTESIAN_POINT('Ctrl Pts',(-49.6222512854117,-21.2849471395443,
178.217719280236));
#12532=CARTESIAN_POINT('Ctrl Pts',(-48.3256452005116,-20.7988977065915,
177.525255091295));
#12533=CARTESIAN_POINT('Ctrl Pts',(-47.8935170509031,-20.5993012814682,
176.78942555283));
#12534=CARTESIAN_POINT('Ctrl Pts',(-47.9069259765589,-20.3679964193449,
175.264267840625));
#12535=CARTESIAN_POINT('Ctrl Pts',(-48.3565963500671,-20.33698501403,174.508050023486));
#12536=CARTESIAN_POINT('Ctrl Pts',(-49.7115395236169,-20.3645147337819,
173.767258025586));
#12537=CARTESIAN_POINT('Ctrl Pts',(-50.5919963646361,-20.4163759449694,
173.798730113887));
#12538=CARTESIAN_POINT('Ctrl Pts',(-51.8921615926268,-20.4324111199544,
174.637786957993));
#12539=CARTESIAN_POINT('Ctrl Pts',(-52.2870845316673,-20.391715494119,175.425932171935));
#12540=CARTESIAN_POINT('Ctrl Pts',(-52.1845249551972,-20.1359343420921,
176.949348485014));
#12541=CARTESIAN_POINT('Ctrl Pts',(-51.6978717551623,-19.9258306519252,
177.647217385389));
#12542=CARTESIAN_POINT('Ctrl Pts',(-50.3567743114224,-19.4332812849397,
178.229888643815));
#12543=CARTESIAN_POINT('Ctrl Pts',(-49.531482093434,-19.1564117811874,178.098575810452));
#12544=CARTESIAN_POINT('Ctrl Pts',(-48.4209526978951,-18.7085233315365,
177.123331466978));
#12545=CARTESIAN_POINT('Ctrl Pts',(-48.1597795720535,-18.5402167412103,
176.29718764283));
#12546=CARTESIAN_POINT('Ctrl Pts',(-48.5145782694716,-18.3739619700934,
174.800216258582));
#12547=CARTESIAN_POINT('Ctrl Pts',(-49.1216168980297,-18.3741927637648,
174.159897255644));
#12548=CARTESIAN_POINT('Ctrl Pts',(-50.6124880467131,-18.4256628314289,
173.74530968569));
#12549=CARTESIAN_POINT('Ctrl Pts',(-51.4570089590119,-18.472296203581,173.973986288395));
#12550=CARTESIAN_POINT('Ctrl Pts',(-52.5367755134872,-18.4465314340497,
175.076321400051));
#12551=CARTESIAN_POINT('Ctrl Pts',(-52.7461464663159,-18.3691716102472,
175.928004990245));
#12552=CARTESIAN_POINT('Ctrl Pts',(-52.3166330239091,-18.0526500335514,
177.376965544067));
#12553=CARTESIAN_POINT('Ctrl Pts',(-51.6857211698905,-17.8130496454,177.945754508989));
#12554=CARTESIAN_POINT('Ctrl Pts',(-50.2465394893753,-17.3007990625156,
178.194297846636));
#12555=CARTESIAN_POINT('Ctrl Pts',(-49.4703000985441,-17.0343670318334,
177.871754882023));
#12556=CARTESIAN_POINT('Ctrl Pts',(-48.6088763818932,-16.6321365971318,
176.648991214725));
#12557=CARTESIAN_POINT('Ctrl Pts',(-48.5409020769561,-16.5028432711256,
175.78526591443));
#12558=CARTESIAN_POINT('Ctrl Pts',(-49.2164515058916,-16.3991203888251,
174.401518908745));
#12559=CARTESIAN_POINT('Ctrl Pts',(-49.9496118192587,-16.4227354715302,
173.914202886417));
#12560=CARTESIAN_POINT('Ctrl Pts',(-51.4902606534728,-16.4861638259448,
173.836744887307));
#12561=CARTESIAN_POINT('Ctrl Pts',(-52.2697075969923,-16.5185243960147,
174.249627738192));
#12562=CARTESIAN_POINT('Ctrl Pts',(-53.0792623986938,-16.4399376212412,
175.566241461313));
#12563=CARTESIAN_POINT('Ctrl Pts',(-53.0958608617722,-16.3264383488088,
176.440260240546));
#12564=CARTESIAN_POINT('Ctrl Pts',(-52.3498924896565,-15.9464100326616,
177.743856795072));
#12565=CARTESIAN_POINT('Ctrl Pts',(-51.6136771994172,-15.6882407493956,
178.142477224647));
#12566=CARTESIAN_POINT('Ctrl Pts',(-50.1619939854693,-15.1743526813971,
178.045393567771));
#12567=CARTESIAN_POINT('Ctrl Pts',(-49.479535393056,-14.9249532161513,177.547481856475));
#12568=CARTESIAN_POINT('Ctrl Pts',(-48.9083003859244,-14.5811172796918,
176.154888290848));
#12569=CARTESIAN_POINT('Ctrl Pts',(-49.032687325759,-14.4872017268269,175.286386043965));
#12570=CARTESIAN_POINT('Ctrl Pts',(-50.002899927607,-14.4395306566209,174.08106638639));
#12571=CARTESIAN_POINT('Ctrl Pts',(-50.8258619899905,-14.4815667576624,
173.768688449528));
#12572=CARTESIAN_POINT('Ctrl Pts',(-52.3490472247602,-14.5391579602322,
174.044477097964));
#12573=CARTESIAN_POINT('Ctrl Pts',(-53.0108480437211,-14.5505369630929,
174.618897762295));
#12574=CARTESIAN_POINT('Ctrl Pts',(-53.508606726061,-14.41258118913,176.072854784516));
#12575=CARTESIAN_POINT('Ctrl Pts',(-53.3308496256547,-14.2605010523332,
176.92211652172));
#12576=CARTESIAN_POINT('Ctrl Pts',(-52.3234046589676,-13.8325238003689,
178.011250192421));
#12577=CARTESIAN_POINT('Ctrl Pts',(-51.5138129382755,-13.5585438056648,
178.229366209696));
#12578=CARTESIAN_POINT('Ctrl Pts',(-50.1182607249297,-13.0546721198729,
177.788098654291));
#12579=CARTESIAN_POINT('Ctrl Pts',(-49.5630188185408,-12.8308644828691,
177.140857971114));
#12580=CARTESIAN_POINT('Ctrl Pts',(-49.3219040202974,-12.5483689245281,
175.637957478437));
#12581=CARTESIAN_POINT('Ctrl Pts',(-49.6365594730894,-12.4926951709364,
174.821179942866));
#12582=CARTESIAN_POINT('Ctrl Pts',(-50.8450351424658,-12.4918253386163,
173.862170041067));
#12583=CARTESIAN_POINT('Ctrl Pts',(-51.7160671936879,-12.5420406725331,
173.742988789581));
#12584=CARTESIAN_POINT('Ctrl Pts',(-53.1380531234061,-12.5824907099911,
174.344563971126));
#12585=CARTESIAN_POINT('Ctrl Pts',(-53.661497991413,-12.565516429584,175.054752397452));
#12586=CARTESIAN_POINT('Ctrl Pts',(-53.8242077932451,-12.3622912981454,
176.579637740953));
#12587=CARTESIAN_POINT('Ctrl Pts',(-53.4635573374974,-12.1759538811977,
177.362604506387));
#12588=CARTESIAN_POINT('Ctrl Pts',(-52.2358756182636,-11.7031645393402,
178.179207046235));
#12589=CARTESIAN_POINT('Ctrl Pts',(-51.404471480006,-11.4266005921062,178.198059647233));
#12590=CARTESIAN_POINT('Ctrl Pts',(-50.1465877134854,-10.9499764840513,
177.440684540534));
#12591=CARTESIAN_POINT('Ctrl Pts',(-49.7512566691313,-10.7559713173261,
176.677961727673));
#12592=CARTESIAN_POINT('Ctrl Pts',(-49.8442980389787,-10.5402489724976,
175.152069846099));
#12593=CARTESIAN_POINT('Ctrl Pts',(-50.3336227209985,-10.5166703329192,
174.417963751365));
#12594=CARTESIAN_POINT('Ctrl Pts',(-51.729412313951,-10.5511670115394,173.750914008412));
#12595=CARTESIAN_POINT('Ctrl Pts',(-52.6055357660183,-10.6034581645062,
173.829125569603));
#12596=CARTESIAN_POINT('Ctrl Pts',(-53.8591972775733,-10.6090268187652,
174.739479897504));
#12597=CARTESIAN_POINT('Ctrl Pts',(-54.2075655427863,-10.559958422732,175.542285446703));
#12598=CARTESIAN_POINT('Ctrl Pts',(-54.0309723767407,-10.2919570312328,
177.05153449857));
#12599=CARTESIAN_POINT('Ctrl Pts',(-53.5065211660476,-10.0729835636969,
177.724885949439));
#12600=CARTESIAN_POINT('Ctrl Pts',(-52.1359327706082,-9.57501150980407,
178.231990439602));
#12601=CARTESIAN_POINT('Ctrl Pts',(-51.3168725161042,-9.29919601638729,
178.055337178134));
#12602=CARTESIAN_POINT('Ctrl Pts',(-50.258716477129,-8.86039345968628,177.014257444883));
#12603=CARTESIAN_POINT('Ctrl Pts',(-50.0419858596938,-8.70190296068798,
176.174822144773));
#12604=CARTESIAN_POINT('Ctrl Pts',(-50.4788136762356,-8.55014763089762,
174.697436550109));
#12605=CARTESIAN_POINT('Ctrl Pts',(-51.1165600370436,-8.55674976323144,
174.095019459488));
#12606=CARTESIAN_POINT('Ctrl Pts',(-52.6206590619166,-8.6128620697194,173.755704628284));
#12607=CARTESIAN_POINT('Ctrl Pts',(-53.456626592603,-8.65630954771657,174.029197443714));
#12608=CARTESIAN_POINT('Ctrl Pts',(-54.4781193003427,-8.6195332279715,175.187078119489));
#12609=CARTESIAN_POINT('Ctrl Pts',(-54.643602443466,-8.53353572012608,176.04949882023));
#12610=CARTESIAN_POINT('Ctrl Pts',(-54.1354947853707,-8.20096498746117,
177.472181687833));
#12611=CARTESIAN_POINT('Ctrl Pts',(-53.4760203027823,-7.95706608118669,
178.003825172765));
#12612=CARTESIAN_POINT('Ctrl Pts',(-52.0249165538012,-7.441132564782,178.167825277993));
#12613=CARTESIAN_POINT('Ctrl Pts',(-51.2723007652614,-7.17976116760829,
177.802466009854));
#12614=CARTESIAN_POINT('Ctrl Pts',(-50.4742318046734,-6.79179686888332,
176.539214575509));
#12615=CARTESIAN_POINT('Ctrl Pts',(-50.4508393849021,-6.66952799804251,
175.667365550039));
#12616=CARTESIAN_POINT('Ctrl Pts',(-51.1982775200671,-6.57992894303025,
174.318931761547));
#12617=CARTESIAN_POINT('Ctrl Pts',(-51.9567203354133,-6.60831910752051,
173.869388776842));
#12618=CARTESIAN_POINT('Ctrl Pts',(-53.5030461170827,-6.67180659392302,
173.876188814802));
#12619=CARTESIAN_POINT('Ctrl Pts',(-54.2579318048227,-6.70074853854407,
174.329266762268));
#12620=CARTESIAN_POINT('Ctrl Pts',(-54.9950541895712,-6.6067812144727,175.688231083653));
#12621=CARTESIAN_POINT('Ctrl Pts',(-54.9633937640365,-6.48434226598442,
176.556150922255));
#12622=CARTESIAN_POINT('Ctrl Pts',(-54.1573516980127,-6.0949735677162,177.812809342709));
#12623=CARTESIAN_POINT('Ctrl Pts',(-53.3979887985791,-5.83073710308303,
178.172806822259));
#12624=CARTESIAN_POINT('Ctrl Pts',(-51.9519097716579,-5.31810666795101,
177.994568269632));
#12625=CARTESIAN_POINT('Ctrl Pts',(-51.2952074816856,-5.0735953089356,177.458800517348));
#12626=CARTESIAN_POINT('Ctrl Pts',(-50.7993635736617,-4.74342220821161,
176.031468409862));
#12627=CARTESIAN_POINT('Ctrl Pts',(-50.9692613848378,-4.65940397939939,
175.170313217647));
#12628=CARTESIAN_POINT('Ctrl Pts',(-52.0040245669764,-4.62293999106357,
174.01934301833));
#12629=CARTESIAN_POINT('Ctrl Pts',(-52.8385688131003,-4.66759138415716,
173.754231358386));
#12630=CARTESIAN_POINT('Ctrl Pts',(-54.3414847379305,-4.72329909029368,
174.103969484305));
#12631=CARTESIAN_POINT('Ctrl Pts',(-54.9761466933045,-4.72791014175074,
174.714716972292));
#12632=CARTESIAN_POINT('Ctrl Pts',(-55.3975165431988,-4.57549651155636,
176.192173272167));
#12633=CARTESIAN_POINT('Ctrl Pts',(-55.1760506072609,-4.4148786220368,177.03103539143));
#12634=CARTESIAN_POINT('Ctrl Pts',(-54.1093043232961,-3.97451188101218,
178.061753391873));
#12635=CARTESIAN_POINT('Ctrl Pts',(-53.2902925544343,-3.69995792969149,
178.233822626392));
#12636=CARTESIAN_POINT('Ctrl Pts',(-51.9203920380846,-3.19963469730891,
177.711493690972));
#12637=CARTESIAN_POINT('Ctrl Pts',(-51.4044324721558,-2.98383265912278,
177.036002564632));
#12638=CARTESIAN_POINT('Ctrl Pts',(-51.237949425703,-2.71774512370317,175.525044339462));
#12639=CARTESIAN_POINT('Ctrl Pts',(-51.5957499271559,-2.66894330374766,
174.721509320474));
#12640=CARTESIAN_POINT('Ctrl Pts',(-52.8541051305037,-2.67783999801612,
173.825937213487));
#12641=CARTESIAN_POINT('Ctrl Pts',(-53.7315999697276,-2.7292086653859,173.7525048498));
#12642=CARTESIAN_POINT('Ctrl Pts',(-55.1208667949195,-2.76252327401043,
174.431246184642));
#12643=CARTESIAN_POINT('Ctrl Pts',(-55.6054709668258,-2.73893798071373,
175.167402226862));
#12644=CARTESIAN_POINT('Ctrl Pts',(-55.6603171863937,-2.58869274068622,
176.211840888345));
#12645=CARTESIAN_POINT('Ctrl Pts',(-55.6210463302226,-2.5392081864434,176.490448482462));
#12646=CARTESIAN_POINT('Ctrl Pts',(-55.4836397365907,-2.4479441182576,176.880586390838));
#12647=CARTESIAN_POINT('Ctrl Pts',(-55.4253285390117,-2.41535251334816,
177.005027857449));
#12648=CARTESIAN_POINT('Ctrl Pts',(-55.321414213033,-2.36345060131236,177.180440236558));
#12649=CARTESIAN_POINT('Ctrl Pts',(-55.2840225057543,-2.34563722905757,
177.23703696138));
#12650=CARTESIAN_POINT('Ctrl Pts',(-55.2039936793606,-2.30896761153951,
177.345998347345));
#12651=CARTESIAN_POINT('Ctrl Pts',(-55.1587206712145,-2.28906361698866,
177.401367187303));
#12652=CARTESIAN_POINT('Ctrl Pts',(-55.1161897096451,-2.27071607222657,
177.448351373365));
#12653=CARTESIAN_POINT('Ctrl Pts',(-50.0383214665825,-27.1440081492037,
177.018259765604));
#12654=CARTESIAN_POINT('Ctrl Pts',(-49.9984978891038,-27.1200869921306,
177.079962725598));
#12655=CARTESIAN_POINT('Ctrl Pts',(-49.9575055461974,-27.1020674615118,
177.117111982701));
#12656=CARTESIAN_POINT('Ctrl Pts',(-49.8677888002033,-27.0582153119246,
177.208150208202));
#12657=CARTESIAN_POINT('Ctrl Pts',(-49.8200811333233,-27.0356913176731,
177.250904604008));
#12658=CARTESIAN_POINT('Ctrl Pts',(-49.6696339972988,-26.9667169890279,
177.369319858048));
#12659=CARTESIAN_POINT('Ctrl Pts',(-49.5596041625372,-26.9190141211719,
177.434440092329));
#12660=CARTESIAN_POINT('Ctrl Pts',(-49.2118492777513,-26.7720570333375,
177.585359994682));
#12661=CARTESIAN_POINT('Ctrl Pts',(-48.9561313182544,-26.6696252716912,
177.624018992736));
#12662=CARTESIAN_POINT('Ctrl Pts',(-48.2061347626312,-26.3651189875991,
177.541325063495));
#12663=CARTESIAN_POINT('Ctrl Pts',(-47.7414452899411,-26.1688071749961,
177.206816180124));
#12664=CARTESIAN_POINT('Ctrl Pts',(-47.2997616792461,-25.8707230428421,
176.259912393579));
#12665=CARTESIAN_POINT('Ctrl Pts',(-47.3254088075791,-25.7696878441865,
175.668385446485));
#12666=CARTESIAN_POINT('Ctrl Pts',(-47.8755348089008,-25.6608852645148,
174.730075629747));
#12667=CARTESIAN_POINT('Ctrl Pts',(-48.3883745667453,-25.6533154874374,
174.409130171609));
#12668=CARTESIAN_POINT('Ctrl Pts',(-49.4697935970405,-25.6493947609597,
174.331547147859));
#12669=CARTESIAN_POINT('Ctrl Pts',(-50.0242338430418,-25.649381701477,174.571983854445));
#12670=CARTESIAN_POINT('Ctrl Pts',(-50.7048786270563,-25.5680766842178,
175.408205503607));
#12671=CARTESIAN_POINT('Ctrl Pts',(-50.8241348799264,-25.4835527568238,
175.999504945815));
#12672=CARTESIAN_POINT('Ctrl Pts',(-50.5299373615978,-25.2151761375736,
177.003363164347));
#12673=CARTESIAN_POINT('Ctrl Pts',(-50.1239438073276,-25.0297634587285,
177.413176265946));
#12674=CARTESIAN_POINT('Ctrl Pts',(-49.1505246752548,-24.6280758402134,
177.688626402201));
#12675=CARTESIAN_POINT('Ctrl Pts',(-48.5986534337901,-24.4145815428545,
177.549736774231));
#12676=CARTESIAN_POINT('Ctrl Pts',(-47.8611459428243,-24.0600384609719,
176.839550282587));
#12677=CARTESIAN_POINT('Ctrl Pts',(-47.6799485846058,-23.9185188665616,
176.282427966132));
#12678=CARTESIAN_POINT('Ctrl Pts',(-47.8667875018081,-23.7413010936383,
175.228664295839));
#12679=CARTESIAN_POINT('Ctrl Pts',(-48.2335406641398,-23.7053609783786,
174.748651320702));
#12680=CARTESIAN_POINT('Ctrl Pts',(-49.2178139490401,-23.6827183215843,
174.294936194443));
#12681=CARTESIAN_POINT('Ctrl Pts',(-49.8219962257384,-23.6923479099038,
174.323992647469));
#12682=CARTESIAN_POINT('Ctrl Pts',(-50.7591498572879,-23.6591435932359,
174.876124371948));
#12683=CARTESIAN_POINT('Ctrl Pts',(-51.077522753783,-23.6134950148359,175.39172485521));
#12684=CARTESIAN_POINT('Ctrl Pts',(-51.1535820381579,-23.415693423287,176.455061557909));
#12685=CARTESIAN_POINT('Ctrl Pts',(-50.918643706726,-23.2638702537623,176.988610346676));
#12686=CARTESIAN_POINT('Ctrl Pts',(-50.1109113395739,-22.8948872174005,
177.611393006538));
#12687=CARTESIAN_POINT('Ctrl Pts',(-49.550353441179,-22.680074585543,177.689808241912));
#12688=CARTESIAN_POINT('Ctrl Pts',(-48.6137447048011,-22.28702457331,177.311258226648));
#12689=CARTESIAN_POINT('Ctrl Pts',(-48.2490117887893,-22.1098470443037,
176.862573175931));
#12690=CARTESIAN_POINT('Ctrl Pts',(-48.0569364843034,-21.8588516971627,
175.821098220226));
#12691=CARTESIAN_POINT('Ctrl Pts',(-48.2348449020816,-21.7860567828884,
175.244332219005));
#12692=CARTESIAN_POINT('Ctrl Pts',(-49.0386897150743,-21.7181941257994,
174.442583421401));
#12693=CARTESIAN_POINT('Ctrl Pts',(-49.6927278496366,-21.7268807239962,
174.267611662058));
#12694=CARTESIAN_POINT('Ctrl Pts',(-50.8411043798997,-21.7141199241716,
174.588524908528));
#12695=CARTESIAN_POINT('Ctrl Pts',(-51.3094013702521,-21.6876269507243,
175.077312328235));
#12696=CARTESIAN_POINT('Ctrl Pts',(-51.5921855585383,-21.5071481278118,
176.224756535618));
#12697=CARTESIAN_POINT('Ctrl Pts',(-51.3974806497779,-21.3525654190584,
176.857134695111));
#12698=CARTESIAN_POINT('Ctrl Pts',(-50.5541169969121,-20.9549536496367,
177.606432421015));
#12699=CARTESIAN_POINT('Ctrl Pts',(-49.9226700094089,-20.7151144402318,
177.707627413831));
#12700=CARTESIAN_POINT('Ctrl Pts',(-48.9071810235129,-20.2857229365746,
177.254800594979));
#12701=CARTESIAN_POINT('Ctrl Pts',(-48.539258060867,-20.0973264562627,176.718436772752));
#12702=CARTESIAN_POINT('Ctrl Pts',(-48.475069365768,-19.8507243142978,175.553477519371));
#12703=CARTESIAN_POINT('Ctrl Pts',(-48.7817617425817,-19.793065331538,174.952184411851));
#12704=CARTESIAN_POINT('Ctrl Pts',(-49.7883433018784,-19.7521647995451,
174.308551222089));
#12705=CARTESIAN_POINT('Ctrl Pts',(-50.4672686416896,-19.7660480884512,
174.284275257332));
#12706=CARTESIAN_POINT('Ctrl Pts',(-51.5185621567429,-19.7338211938064,
174.853733695028));
#12707=CARTESIAN_POINT('Ctrl Pts',(-51.8704305933054,-19.6836035315617,
175.436932234299));
#12708=CARTESIAN_POINT('Ctrl Pts',(-51.8843323266907,-19.4527281797322,
176.606134032902));
#12709=CARTESIAN_POINT('Ctrl Pts',(-51.5571193795133,-19.2721887380014,
177.170821269618));
#12710=CARTESIAN_POINT('Ctrl Pts',(-50.5738822832083,-18.8483164964054,
177.696322750616));
#12711=CARTESIAN_POINT('Ctrl Pts',(-49.9420101663495,-18.6096692642048,
177.644259926591));
#12712=CARTESIAN_POINT('Ctrl Pts',(-49.0472024681392,-18.2021277928874,
176.964465534643));
#12713=CARTESIAN_POINT('Ctrl Pts',(-48.8080140865945,-18.0389468515475,
176.349664596734));
#12714=CARTESIAN_POINT('Ctrl Pts',(-49.0066488397389,-17.8423059144124,
175.186793179499));
#12715=CARTESIAN_POINT('Ctrl Pts',(-49.4421820059815,-17.8082452535064,
174.661978305101));
#12716=CARTESIAN_POINT('Ctrl Pts',(-50.56604357313,-17.7913894148755,174.265152819574));
#12717=CARTESIAN_POINT('Ctrl Pts',(-51.2311395254822,-17.8022399917982,
174.391161445375));
#12718=CARTESIAN_POINT('Ctrl Pts',(-52.1286453083844,-17.7409968363402,
175.174698745784));
#12719=CARTESIAN_POINT('Ctrl Pts',(-52.340061283037,-17.6649540872478,175.813880719354));
#12720=CARTESIAN_POINT('Ctrl Pts',(-52.1027685307223,-17.384247754716,176.951110854015));
#12721=CARTESIAN_POINT('Ctrl Pts',(-51.6569691297711,-17.1812314095055,
177.42208876923));
#12722=CARTESIAN_POINT('Ctrl Pts',(-50.5803007618318,-16.7386138153048,
177.697510231007));
#12723=CARTESIAN_POINT('Ctrl Pts',(-49.9722430688612,-16.5033958825231,
177.495874655633));
#12724=CARTESIAN_POINT('Ctrl Pts',(-49.2598451033921,-16.1323520825764,
176.614580397518));
#12725=CARTESIAN_POINT('Ctrl Pts',(-49.1633964478354,-15.9963838869222,
175.958557394859));
#12726=CARTESIAN_POINT('Ctrl Pts',(-49.6135825845651,-15.8488720097956,
174.863627023648));
#12727=CARTESIAN_POINT('Ctrl Pts',(-50.1513088289339,-15.8357216637453,
174.451396860398));
#12728=CARTESIAN_POINT('Ctrl Pts',(-51.3373123393945,-15.8295083514664,
174.304991255183));
#12729=CARTESIAN_POINT('Ctrl Pts',(-51.9598057434752,-15.8324905082382,
174.577589691682));
#12730=CARTESIAN_POINT('Ctrl Pts',(-52.662356604517,-15.7329936013494,175.540542955831));
#12731=CARTESIAN_POINT('Ctrl Pts',(-52.7287365437827,-15.6278770852026,
176.211335092655));
#12732=CARTESIAN_POINT('Ctrl Pts',(-52.2404503570114,-15.2999892249187,
177.248966419092));
#12733=CARTESIAN_POINT('Ctrl Pts',(-51.7049290320028,-15.079336195701,177.599407337456));
#12734=CARTESIAN_POINT('Ctrl Pts',(-50.599341197491,-14.6318604318474,177.611289749054));
#12735=CARTESIAN_POINT('Ctrl Pts',(-50.0563698831837,-14.4102803084529,
177.271399907022));
#12736=CARTESIAN_POINT('Ctrl Pts',(-49.5511866458666,-14.0779293284932,
176.24060069501));
#12737=CARTESIAN_POINT('Ctrl Pts',(-49.604058679892,-13.971112568136,175.571774049481));
#12738=CARTESIAN_POINT('Ctrl Pts',(-50.2895824050587,-13.8682646399117,
174.596554366676));
#12739=CARTESIAN_POINT('Ctrl Pts',(-50.9089033822508,-13.8698152300494,
174.310925422501));
#12740=CARTESIAN_POINT('Ctrl Pts',(-52.0945937584551,-13.8647732522077,
174.438441317441));
#12741=CARTESIAN_POINT('Ctrl Pts',(-52.6396705452532,-13.8524570813917,
174.840092836798));
#12742=CARTESIAN_POINT('Ctrl Pts',(-53.1114861845869,-13.7091720746061,
175.926135983292));
#12743=CARTESIAN_POINT('Ctrl Pts',(-53.0273981908184,-13.5760746720968,
176.585468457757));
#12744=CARTESIAN_POINT('Ctrl Pts',(-52.3273047331872,-13.2061141571923,
177.480731662196));
#12745=CARTESIAN_POINT('Ctrl Pts',(-51.7260689896615,-12.9732036309654,
177.694033962224));
#12746=CARTESIAN_POINT('Ctrl Pts',(-50.6444965881338,-12.5296009109336,
177.439340266607));
#12747=CARTESIAN_POINT('Ctrl Pts',(-50.1880101288259,-12.323622761024,176.975929902189));
#12748=CARTESIAN_POINT('Ctrl Pts',(-49.9332603826239,-12.0409453485109,
175.846473225312));
#12749=CARTESIAN_POINT('Ctrl Pts',(-50.1325085529845,-11.9618298866148,
175.20357102314));
#12750=CARTESIAN_POINT('Ctrl Pts',(-51.0139495749547,-11.8975707104174,
174.402850839007));
#12751=CARTESIAN_POINT('Ctrl Pts',(-51.6770380739026,-11.9086053392238,
174.263669429449));
#12752=CARTESIAN_POINT('Ctrl Pts',(-52.8102442474793,-11.89211453585,174.644220443453));
#12753=CARTESIAN_POINT('Ctrl Pts',(-53.2534129688289,-11.860550625243,175.158200214442));
#12754=CARTESIAN_POINT('Ctrl Pts',(-53.4727724514858,-11.667970777174,176.317676214963));
#12755=CARTESIAN_POINT('Ctrl Pts',(-53.2447122957938,-11.5059876351892,
176.940267405791));
#12756=CARTESIAN_POINT('Ctrl Pts',(-52.3630606041574,-11.1023742765951,
177.633671542876));
#12757=CARTESIAN_POINT('Ctrl Pts',(-51.7328063873735,-10.863413150139,177.698996091772));
#12758=CARTESIAN_POINT('Ctrl Pts',(-50.7387975664535,-10.4373493069837,
177.194617067458));
#12759=CARTESIAN_POINT('Ctrl Pts',(-50.4003959556136,-10.2552411513015,
176.636362249629));
#12760=CARTESIAN_POINT('Ctrl Pts',(-50.3964887911414,-10.0195709762704,
175.464836254896));
#12761=CARTESIAN_POINT('Ctrl Pts',(-50.7352645697859,-9.96785241001128,
174.878086269107));
#12762=CARTESIAN_POINT('Ctrl Pts',(-51.7761584941716,-9.93363014738946,
174.290073576044));
#12763=CARTESIAN_POINT('Ctrl Pts',(-52.4578743221659,-9.94721824196466,
174.301034748671));
#12764=CARTESIAN_POINT('Ctrl Pts',(-53.4723487166264,-9.90911175935534,
174.927224952557));
#12765=CARTESIAN_POINT('Ctrl Pts',(-53.7905639694071,-9.85304000489839,
175.522456262626));
#12766=CARTESIAN_POINT('Ctrl Pts',(-53.7495974866252,-9.61086987508902,
176.689642787431));
#12767=CARTESIAN_POINT('Ctrl Pts',(-53.3913473444599,-9.42486391207369,
177.234457154129));
#12768=CARTESIAN_POINT('Ctrl Pts',(-52.3804909291071,-8.9950096827268,177.705080880716));
#12769=CARTESIAN_POINT('Ctrl Pts',(-51.7506169575959,-8.75656955580448,
177.617528508224));
#12770=CARTESIAN_POINT('Ctrl Pts',(-50.8938217209944,-8.35631416012115,
176.884644400558));
#12771=CARTESIAN_POINT('Ctrl Pts',(-50.686386739593,-8.19840449522365,176.254364811283));
#12772=CARTESIAN_POINT('Ctrl Pts',(-50.9496816541175,-8.01563271032117,
175.10646784668));
#12773=CARTESIAN_POINT('Ctrl Pts',(-51.4086597834924,-7.98657238824085,
174.608429324338));
#12774=CARTESIAN_POINT('Ctrl Pts',(-52.5506583028891,-7.97253715897243,
174.264721414109));
#12775=CARTESIAN_POINT('Ctrl Pts',(-53.2085070979977,-7.98255305121696,
174.427141629608));
#12776=CARTESIAN_POINT('Ctrl Pts',(-54.0661826067832,-7.91293346685192,
175.257046778597));
#12777=CARTESIAN_POINT('Ctrl Pts',(-54.2443196068901,-7.83026930904402,
175.907383805075));
#12778=CARTESIAN_POINT('Ctrl Pts',(-53.9449265679421,-7.53766373675317,
177.027297077911));
#12779=CARTESIAN_POINT('Ctrl Pts',(-53.4737144264175,-7.32885697968307,
177.474235384447));
#12780=CARTESIAN_POINT('Ctrl Pts',(-52.3866301268079,-6.88556912331281,
177.682767568372));
#12781=CARTESIAN_POINT('Ctrl Pts',(-51.7946034524202,-6.6539762900198,177.44919290535));
#12782=CARTESIAN_POINT('Ctrl Pts',(-51.1242376556131,-6.29031677842802,
176.53135144958));
#12783=CARTESIAN_POINT('Ctrl Pts',(-51.0636455015902,-6.16179111781231,
175.868699032101));
#12784=CARTESIAN_POINT('Ctrl Pts',(-51.5708785507503,-6.02461835391231,
174.795021951807));
#12785=CARTESIAN_POINT('Ctrl Pts',(-52.1305414737447,-6.01557067494389,
174.410384417273));
#12786=CARTESIAN_POINT('Ctrl Pts',(-53.3239707675344,-6.01072022664985,
174.329110015938));
#12787=CARTESIAN_POINT('Ctrl Pts',(-53.9334177584311,-6.01040522494539,
174.634606029695));
#12788=CARTESIAN_POINT('Ctrl Pts',(-54.5783977308191,-5.90111793801205,
175.631553651875));
#12789=CARTESIAN_POINT('Ctrl Pts',(-54.6093650217473,-5.78956533803437,
176.299320421659));
#12790=CARTESIAN_POINT('Ctrl Pts',(-54.0728671794864,-5.45185644429227,
177.309544041851));
#12791=CARTESIAN_POINT('Ctrl Pts',(-53.5182109168208,-5.22801082267814,
177.628618080665));
#12792=CARTESIAN_POINT('Ctrl Pts',(-52.4111095558568,-4.77949537513279,
177.578747218087));
#12793=CARTESIAN_POINT('Ctrl Pts',(-51.8857104064777,-4.56119881916171,
177.207895099161));
#12794=CARTESIAN_POINT('Ctrl Pts',(-51.4375681932236,-4.23993965724606,
176.147216345704));
#12795=CARTESIAN_POINT('Ctrl Pts',(-51.5255341013567,-4.13891120462634,
175.478088476179));
#12796=CARTESIAN_POINT('Ctrl Pts',(-52.2621121714531,-4.04739311840896,
174.545543255356));
#12797=CARTESIAN_POINT('Ctrl Pts',(-52.8911810801,-4.05123090724587,174.294043710706));
#12798=CARTESIAN_POINT('Ctrl Pts',(-54.0705541410016,-4.04422766004653,
174.477498952297));
#12799=CARTESIAN_POINT('Ctrl Pts',(-54.593284417315,-4.02816934534973,174.908686002258));
#12800=CARTESIAN_POINT('Ctrl Pts',(-55.0092587601974,-3.87346271742067,
176.018250487428));
#12801=CARTESIAN_POINT('Ctrl Pts',(-54.8907029615328,-3.73358556412494,
176.67236673678));
#12802=CARTESIAN_POINT('Ctrl Pts',(-54.1422797098421,-3.35431610458726,
177.524634651606));
#12803=CARTESIAN_POINT('Ctrl Pts',(-53.5287781394068,-3.11818277146878,
177.704881014433));
#12804=CARTESIAN_POINT('Ctrl Pts',(-52.4666030700143,-2.67965003658039,
177.385814188219));
#12805=CARTESIAN_POINT('Ctrl Pts',(-52.037952109723,-2.47949238143003,176.900644117435));
#12806=CARTESIAN_POINT('Ctrl Pts',(-51.8369606432704,-2.20643344946428,
175.75693673757));
#12807=CARTESIAN_POINT('Ctrl Pts',(-52.0709636415419,-2.13467360272607,
175.124746251973));
#12808=CARTESIAN_POINT('Ctrl Pts',(-52.9948906247979,-2.07782438513344,
174.368185237747));
#12809=CARTESIAN_POINT('Ctrl Pts',(-53.6658603596095,-2.09023021076396,
174.26394539811));
#12810=CARTESIAN_POINT('Ctrl Pts',(-54.7763899734937,-2.0695796979931,174.705748499134));
#12811=CARTESIAN_POINT('Ctrl Pts',(-55.193636646253,-2.03216929631525,175.243747077929));
#12812=CARTESIAN_POINT('Ctrl Pts',(-55.2990804121262,-1.89289436927212,
176.038719570758));
#12813=CARTESIAN_POINT('Ctrl Pts',(-55.2875271080061,-1.8476232285876,176.255654667139));
#12814=CARTESIAN_POINT('Ctrl Pts',(-55.2062064365128,-1.76817883590891,
176.561034862255));
#12815=CARTESIAN_POINT('Ctrl Pts',(-55.1692797902087,-1.73965218400568,
176.660101738528));
#12816=CARTESIAN_POINT('Ctrl Pts',(-55.100781391479,-1.69439363416682,176.801019080259));
#12817=CARTESIAN_POINT('Ctrl Pts',(-55.0757487692566,-1.67889591755103,
176.846705834293));
#12818=CARTESIAN_POINT('Ctrl Pts',(-55.0215162671022,-1.64716827604208,
176.934897450488));
#12819=CARTESIAN_POINT('Ctrl Pts',(-54.9831012773678,-1.62642361195712,
176.988063802692));
#12820=CARTESIAN_POINT('Ctrl Pts',(-54.9611536226478,-1.61438316700751,
177.018013216499));
#12821=CARTESIAN_POINT('Ctrl Pts',(-49.4509304485228,-27.5317240793367,
176.63793339336));
#12822=CARTESIAN_POINT('Ctrl Pts',(-49.4291393884885,-27.5076562767722,
176.671636728953));
#12823=CARTESIAN_POINT('Ctrl Pts',(-49.4023252814003,-27.49622653535,176.696313164424));
#12824=CARTESIAN_POINT('Ctrl Pts',(-49.3476504462613,-27.4590129437169,
176.750465273433));
#12825=CARTESIAN_POINT('Ctrl Pts',(-49.3184236390985,-27.4399206811032,
176.775937697594));
#12826=CARTESIAN_POINT('Ctrl Pts',(-49.2266057058354,-27.3820561699738,
176.84602259684));
#12827=CARTESIAN_POINT('Ctrl Pts',(-49.1608892759397,-27.3435420466437,
176.883532818161));
#12828=CARTESIAN_POINT('Ctrl Pts',(-48.9520433277106,-27.2233369569446,
176.969216598557));
#12829=CARTESIAN_POINT('Ctrl Pts',(-48.7994772773074,-27.140753695473,176.988359561004));
#12830=CARTESIAN_POINT('Ctrl Pts',(-48.3519200751284,-26.8936813947759,
176.923562975379));
#12831=CARTESIAN_POINT('Ctrl Pts',(-48.0823456895327,-26.734263465041,176.708580257885));
#12832=CARTESIAN_POINT('Ctrl Pts',(-47.8449430900585,-26.4783672905687,
176.126725989992));
#12833=CARTESIAN_POINT('Ctrl Pts',(-47.8767939676907,-26.3778568396964,
175.764012928805));
#12834=CARTESIAN_POINT('Ctrl Pts',(-48.2463197375522,-26.2327937589041,
175.197492946021));
#12835=CARTESIAN_POINT('Ctrl Pts',(-48.5747178643875,-26.1889682126354,
175.01137731386));
#12836=CARTESIAN_POINT('Ctrl Pts',(-49.2462054467177,-26.1087803247027,
174.981703215741));
#12837=CARTESIAN_POINT('Ctrl Pts',(-49.5907543357586,-26.0676212071441,
175.137035562833));
#12838=CARTESIAN_POINT('Ctrl Pts',(-50.009388927793,-25.9343746307825,175.661646016755));
#12839=CARTESIAN_POINT('Ctrl Pts',(-50.0783027352647,-25.8394975457309,
176.025761110018));
#12840=CARTESIAN_POINT('Ctrl Pts',(-49.8988780633176,-25.5959204367964,
176.628597112503));
#12841=CARTESIAN_POINT('Ctrl Pts',(-49.6518990744916,-25.4405710050954,
176.873652740602));
#12842=CARTESIAN_POINT('Ctrl Pts',(-49.0655102948359,-25.1120926941016,
177.024416386827));
#12843=CARTESIAN_POINT('Ctrl Pts',(-48.7382306499136,-24.9412172473198,
176.927283980104));
#12844=CARTESIAN_POINT('Ctrl Pts',(-48.31783324883,-24.6506072191097,176.48408449858));
#12845=CARTESIAN_POINT('Ctrl Pts',(-48.2223197693695,-24.5249427903147,
176.139359044285));
#12846=CARTESIAN_POINT('Ctrl Pts',(-48.3708320195333,-24.3389138358785,
175.495466335841));
#12847=CARTESIAN_POINT('Ctrl Pts',(-48.6129161956615,-24.2782922597527,
175.208867671322));
#12848=CARTESIAN_POINT('Ctrl Pts',(-49.2318343995499,-24.18785243492,174.949625492768));
#12849=CARTESIAN_POINT('Ctrl Pts',(-49.6097264895464,-24.153250081799,174.976039603467));
#12850=CARTESIAN_POINT('Ctrl Pts',(-50.1907740657023,-24.0499499019578,
175.330958269522));
#12851=CARTESIAN_POINT('Ctrl Pts',(-50.3830787723347,-23.9792981329734,
175.653008106489));
#12852=CARTESIAN_POINT('Ctrl Pts',(-50.427159666228,-23.7781136900229,176.297852422263));
#12853=CARTESIAN_POINT('Ctrl Pts',(-50.2832787288339,-23.643180828803,176.621446326487));
#12854=CARTESIAN_POINT('Ctrl Pts',(-49.7924641893585,-23.3338917128074,
176.988303084673));
#12855=CARTESIAN_POINT('Ctrl Pts',(-49.455479895244,-23.1615506277796,177.024112028042));
#12856=CARTESIAN_POINT('Ctrl Pts',(-48.9089639726264,-22.8463871647641,
176.778406765063));
#12857=CARTESIAN_POINT('Ctrl Pts',(-48.699448601228,-22.6985448431478,176.497595410894));
#12858=CARTESIAN_POINT('Ctrl Pts',(-48.6153144001997,-22.4669397150842,
175.854418703293));
#12859=CARTESIAN_POINT('Ctrl Pts',(-48.7438560906085,-22.3839338201049,
175.504557803726));
#12860=CARTESIAN_POINT('Ctrl Pts',(-49.2595227997445,-22.2634194140522,
175.031489327737));
#12861=CARTESIAN_POINT('Ctrl Pts',(-49.6731287428438,-22.2242903845664,
174.93387435438));
#12862=CARTESIAN_POINT('Ctrl Pts',(-50.3871280758708,-22.1273049999089,
175.149675576275));
#12863=CARTESIAN_POINT('Ctrl Pts',(-50.6724659987737,-22.0667095289654,
175.454257853488));
#12864=CARTESIAN_POINT('Ctrl Pts',(-50.8432291330538,-21.8630647724227,
176.162580877915));
#12865=CARTESIAN_POINT('Ctrl Pts',(-50.7223573298116,-21.7238000115757,
176.543315008655));
#12866=CARTESIAN_POINT('Ctrl Pts',(-50.2109398093855,-21.3899066275767,
176.985840165295));
#12867=CARTESIAN_POINT('Ctrl Pts',(-49.8297406934723,-21.1967740899633,
177.034608068765));
#12868=CARTESIAN_POINT('Ctrl Pts',(-49.2383022679982,-20.8522162432738,
176.742643808163));
#12869=CARTESIAN_POINT('Ctrl Pts',(-49.0288695410029,-20.692930608689,176.406589078903));
#12870=CARTESIAN_POINT('Ctrl Pts',(-49.026421127215,-20.4577766282769,175.692082743004));
#12871=CARTESIAN_POINT('Ctrl Pts',(-49.2307435857662,-20.3815547180372,
175.331094438645));
#12872=CARTESIAN_POINT('Ctrl Pts',(-49.8766835352141,-20.269544445424,174.953525304613));
#12873=CARTESIAN_POINT('Ctrl Pts',(-50.2982947167721,-20.234888952096,174.950394529643));
#12874=CARTESIAN_POINT('Ctrl Pts',(-50.9484787003876,-20.125016744292,175.316388781725));
#12875=CARTESIAN_POINT('Ctrl Pts',(-51.1618775184403,-20.046547250015,175.681463428659));
#12876=CARTESIAN_POINT('Ctrl Pts',(-51.1680956128,-19.8172503157992,176.389348367045));
#12877=CARTESIAN_POINT('Ctrl Pts',(-50.9669054157941,-19.6595598406301,
176.731136037536));
#12878=CARTESIAN_POINT('Ctrl Pts',(-50.3735191706099,-19.3104097045359,
177.03446439702));
#12879=CARTESIAN_POINT('Ctrl Pts',(-49.9983681415115,-19.122445314997,176.992069263085));
#12880=CARTESIAN_POINT('Ctrl Pts',(-49.4783291859613,-18.7856098039383,
176.558083132201));
#12881=CARTESIAN_POINT('Ctrl Pts',(-49.3516920035876,-18.6452157185327,
176.179591346513));
#12882=CARTESIAN_POINT('Ctrl Pts',(-49.5099669630901,-18.4404938180664,
175.471248155379));
#12883=CARTESIAN_POINT('Ctrl Pts',(-49.7966826107081,-18.3761869903911,
175.157298861455));
#12884=CARTESIAN_POINT('Ctrl Pts',(-50.5005002255267,-18.2813908051205,
174.934848239897));
#12885=CARTESIAN_POINT('Ctrl Pts',(-50.9163195448478,-18.2427172185017,
175.022527695559));
#12886=CARTESIAN_POINT('Ctrl Pts',(-51.4689900750814,-18.1145211614547,
175.516882458909));
#12887=CARTESIAN_POINT('Ctrl Pts',(-51.5957313663424,-18.0233261232984,
175.908710828391));
#12888=CARTESIAN_POINT('Ctrl Pts',(-51.4475718943418,-17.7582443007608,
176.601404917962));
#12889=CARTESIAN_POINT('Ctrl Pts',(-51.1767645681398,-17.5900571721881,
176.879541091562));
#12890=CARTESIAN_POINT('Ctrl Pts',(-50.5307383316194,-17.2301836239675,
177.028185493998));
#12891=CARTESIAN_POINT('Ctrl Pts',(-50.1698955770676,-17.0410908031352,
176.891376748831));
#12892=CARTESIAN_POINT('Ctrl Pts',(-49.7689671613288,-16.733171977968,176.344861065041));
#12893=CARTESIAN_POINT('Ctrl Pts',(-49.7283236820348,-16.606509721343,175.939499115166));
#12894=CARTESIAN_POINT('Ctrl Pts',(-50.039329025483,-16.4317046321664,175.276913396961));
#12895=CARTESIAN_POINT('Ctrl Pts',(-50.3811663065111,-16.3819545297351,
175.034692629757));
#12896=CARTESIAN_POINT('Ctrl Pts',(-51.1285550225506,-16.289595439286,174.965429755586));
#12897=CARTESIAN_POINT('Ctrl Pts',(-51.5107791504261,-16.247329788901,175.141829956289));
#12898=CARTESIAN_POINT('Ctrl Pts',(-51.9410271179475,-16.0950193648309,
175.742297045045));
#12899=CARTESIAN_POINT('Ctrl Pts',(-51.9772772372669,-15.9825461483302,
176.155328152494));
#12900=CARTESIAN_POINT('Ctrl Pts',(-51.6813604170028,-15.6948169276305,
176.775145838897));
#12901=CARTESIAN_POINT('Ctrl Pts',(-51.3553093740791,-15.5131006527082,
176.981869312707));
#12902=CARTESIAN_POINT('Ctrl Pts',(-50.6958293220101,-15.1512003838696,
176.968860943967));
#12903=CARTESIAN_POINT('Ctrl Pts',(-50.3793004471536,-14.974461104635,176.752883253889));
#12904=CARTESIAN_POINT('Ctrl Pts',(-50.1044053585231,-14.6849545931669,
176.110550614429));
#12905=CARTESIAN_POINT('Ctrl Pts',(-50.1562892256051,-14.5790344049375,
175.704381183727));
#12906=CARTESIAN_POINT('Ctrl Pts',(-50.6091148636379,-14.4310075872896,
175.119365593043));
#12907=CARTESIAN_POINT('Ctrl Pts',(-51.0040002342342,-14.3877335732316,
174.956144468714));
#12908=CARTESIAN_POINT('Ctrl Pts',(-51.7368765161625,-14.2984333198446,
175.052400920313));
#12909=CARTESIAN_POINT('Ctrl Pts',(-52.0746787278137,-14.2446881736679,
175.307721150405));
#12910=CARTESIAN_POINT('Ctrl Pts',(-52.3618029222314,-14.0653384618121,
175.979593696432));
#12911=CARTESIAN_POINT('Ctrl Pts',(-52.3085224478133,-13.9393545956389,
176.378830696363));
#12912=CARTESIAN_POINT('Ctrl Pts',(-51.8806097785072,-13.6203167705008,
176.914733769747));
#12913=CARTESIAN_POINT('Ctrl Pts',(-51.5196766160896,-13.4348339691437,
177.033422941425));
#12914=CARTESIAN_POINT('Ctrl Pts',(-50.8796650354229,-13.0760747213028,
176.857816848924));
#12915=CARTESIAN_POINT('Ctrl Pts',(-50.6171262914928,-12.905954023484,176.563294278628));
#12916=CARTESIAN_POINT('Ctrl Pts',(-50.4974416512911,-12.6523824704848,
175.874038771655));
#12917=CARTESIAN_POINT('Ctrl Pts',(-50.6384867622314,-12.5605842376971,
175.481424733232));
#12918=CARTESIAN_POINT('Ctrl Pts',(-51.2082627201524,-12.4357774521296,
175.006422958104));
#12919=CARTESIAN_POINT('Ctrl Pts',(-51.6220204445227,-12.3999030775176,
174.932310130414));
#12920=CARTESIAN_POINT('Ctrl Pts',(-52.3278760969134,-12.2994377602634,
175.185413156184));
#12921=CARTESIAN_POINT('Ctrl Pts',(-52.5969267492371,-12.2353856775628,
175.505423112887));
#12922=CARTESIAN_POINT('Ctrl Pts',(-52.7283564524999,-12.0255423744405,
176.2175433277));
#12923=CARTESIAN_POINT('Ctrl Pts',(-52.5846730379872,-11.8782873041682,
176.594912064781));
#12924=CARTESIAN_POINT('Ctrl Pts',(-52.0559417647627,-11.5457913524836,
176.999632681105));
#12925=CARTESIAN_POINT('Ctrl Pts',(-51.6759748702359,-11.3536364027873,
177.029489895259));
#12926=CARTESIAN_POINT('Ctrl Pts',(-51.0935427887116,-11.0064931497742,
176.702663500826));
#12927=CARTESIAN_POINT('Ctrl Pts',(-50.9048767955961,-10.8544314216914,
176.357244031546));
#12928=CARTESIAN_POINT('Ctrl Pts',(-50.9399834898308,-10.6247204655602,
175.63759182164));
#12929=CARTESIAN_POINT('Ctrl Pts',(-51.1643267174014,-10.5520247194105,
175.286394351447));
#12930=CARTESIAN_POINT('Ctrl Pts',(-51.827873009513,-10.4447251212865,174.944424130566));
#12931=CARTESIAN_POINT('Ctrl Pts',(-52.2552179028772,-10.4077182802165,
174.964702471846));
#12932=CARTESIAN_POINT('Ctrl Pts',(-52.8763669051787,-10.2968258721765,
175.360239151239));
#12933=CARTESIAN_POINT('Ctrl Pts',(-53.071683414474,-10.215593033151,175.73103698433));
#12934=CARTESIAN_POINT('Ctrl Pts',(-53.0437675059112,-9.97549498249197,
176.443487491333));
#12935=CARTESIAN_POINT('Ctrl Pts',(-52.825568431635,-9.81766629245078,176.768582048511));
#12936=CARTESIAN_POINT('Ctrl Pts',(-52.2143534856381,-9.46331409552581,
177.038351228206));
#12937=CARTESIAN_POINT('Ctrl Pts',(-51.8411412849432,-9.27545967967225,
176.973585868646));
#12938=CARTESIAN_POINT('Ctrl Pts',(-51.3467118649778,-8.94477024831946,
176.509526159241));
#12939=CARTESIAN_POINT('Ctrl Pts',(-51.2404836863797,-8.80483732687828,
176.117599105019));
#12940=CARTESIAN_POINT('Ctrl Pts',(-51.4349583516297,-8.61185430488912,
175.425788146171));
#12941=CARTESIAN_POINT('Ctrl Pts',(-51.7335486000159,-8.55040314694308,
175.126384517701));
#12942=CARTESIAN_POINT('Ctrl Pts',(-52.4549196826756,-8.45481293341497,
174.935526629257));
#12943=CARTESIAN_POINT('Ctrl Pts',(-52.8607223331575,-8.41739346719437,
175.04474867484));
#12944=CARTESIAN_POINT('Ctrl Pts',(-53.3897252776085,-8.28282809274167,
175.568595073035));
#12945=CARTESIAN_POINT('Ctrl Pts',(-53.4952826969923,-8.1872595086965,175.966830212787));
#12946=CARTESIAN_POINT('Ctrl Pts',(-53.3101642867802,-7.91637813164073,
176.645610777581));
#12947=CARTESIAN_POINT('Ctrl Pts',(-53.02056762136,-7.74105352934409,176.910070201754));
#12948=CARTESIAN_POINT('Ctrl Pts',(-52.3751524190461,-7.38599804306437,
177.017607675131));
#12949=CARTESIAN_POINT('Ctrl Pts',(-52.0232566558232,-7.19924964083975,
176.864225220861));
#12950=CARTESIAN_POINT('Ctrl Pts',(-51.6458284953554,-6.89163712519652,
176.29020971736));
#12951=CARTESIAN_POINT('Ctrl Pts',(-51.6277644578821,-6.7724816775637,175.885858382765));
#12952=CARTESIAN_POINT('Ctrl Pts',(-51.9747906942483,-6.6028499237395,175.235443151034));
#12953=CARTESIAN_POINT('Ctrl Pts',(-52.3299962525585,-6.55546850196264,
175.011060208135));
#12954=CARTESIAN_POINT('Ctrl Pts',(-53.0782096175287,-6.46444741567071,
174.9816560919));
#12955=CARTESIAN_POINT('Ctrl Pts',(-53.4553178435249,-6.41778988524295,
175.181401713961));
#12956=CARTESIAN_POINT('Ctrl Pts',(-53.8466529433518,-6.26265155715774,
175.795420851333));
#12957=CARTESIAN_POINT('Ctrl Pts',(-53.864188958285,-6.14704492720176,176.206287912404));
#12958=CARTESIAN_POINT('Ctrl Pts',(-53.5358416511927,-5.84903598495515,
176.813977641948));
#12959=CARTESIAN_POINT('Ctrl Pts',(-53.2017653978813,-5.66889429660941,
176.99856451113));
#12960=CARTESIAN_POINT('Ctrl Pts',(-52.5405403606902,-5.30479587533914,
176.947248559284));
#12961=CARTESIAN_POINT('Ctrl Pts',(-52.2356929075399,-5.13012364220884,
176.712058308829));
#12962=CARTESIAN_POINT('Ctrl Pts',(-51.9967219623743,-4.84888631606004,
176.054758979681));
#12963=CARTESIAN_POINT('Ctrl Pts',(-52.0727509238964,-4.74401755802611,
175.645031481929));
#12964=CARTESIAN_POINT('Ctrl Pts',(-52.5505176724514,-4.6056507589775,175.091566392661));
#12965=CARTESIAN_POINT('Ctrl Pts',(-52.9499574883172,-4.56374410570602,
174.946492448473));
#12966=CARTESIAN_POINT('Ctrl Pts',(-53.685231908784,-4.47066113931358,175.078743542747));
#12967=CARTESIAN_POINT('Ctrl Pts',(-54.0046084640979,-4.41655583760205,
175.349203817777));
#12968=CARTESIAN_POINT('Ctrl Pts',(-54.2577428662421,-4.2288827567675,176.036685454146));
#12969=CARTESIAN_POINT('Ctrl Pts',(-54.1828214302285,-4.09851492101137,
176.431966849275));
#12970=CARTESIAN_POINT('Ctrl Pts',(-53.7276699197103,-3.77548143923658,
176.939160233154));
#12971=CARTESIAN_POINT('Ctrl Pts',(-53.3559275609679,-3.58443131799679,
177.036850521868));
#12972=CARTESIAN_POINT('Ctrl Pts',(-52.7340684542075,-3.23387064793483,
176.825149499914));
#12973=CARTESIAN_POINT('Ctrl Pts',(-52.4865052787647,-3.06716804391598,
176.519600526728));
#12974=CARTESIAN_POINT('Ctrl Pts',(-52.4000162427049,-2.81575249291398,
175.815720536334));
#12975=CARTESIAN_POINT('Ctrl Pts',(-52.5606356723736,-2.73100846880393,
175.434725535823));
#12976=CARTESIAN_POINT('Ctrl Pts',(-53.1578253291134,-2.60958353788362,
174.986380686329));
#12977=CARTESIAN_POINT('Ctrl Pts',(-53.575919582614,-2.57427864177586,174.934476257966));
#12978=CARTESIAN_POINT('Ctrl Pts',(-54.2645385526377,-2.47204238084449,
175.223470220004));
#12979=CARTESIAN_POINT('Ctrl Pts',(-54.5189943505689,-2.4021627120238,175.561903562137));
#12980=CARTESIAN_POINT('Ctrl Pts',(-54.5814297773468,-2.25612793931688,
176.045419377677));
#12981=CARTESIAN_POINT('Ctrl Pts',(-54.5735173041519,-2.21013144506474,
176.178993521001));
#12982=CARTESIAN_POINT('Ctrl Pts',(-54.5239654997844,-2.13806319233694,
176.36226950621));
#12983=CARTESIAN_POINT('Ctrl Pts',(-54.5010361022764,-2.1121733501921,176.42270110964));
#12984=CARTESIAN_POINT('Ctrl Pts',(-54.4586925003588,-2.07172971741335,
176.508171829538));
#12985=CARTESIAN_POINT('Ctrl Pts',(-54.4432559654462,-2.05799768545568,
176.53580222906));
#12986=CARTESIAN_POINT('Ctrl Pts',(-54.410122331684,-2.03029642349882,176.588723178982));
#12987=CARTESIAN_POINT('Ctrl Pts',(-54.3884821434676,-2.0139079395113,176.618668306411));
#12988=CARTESIAN_POINT('Ctrl Pts',(-54.3738267566562,-2.00237092626598,
176.637865020199));
#12989=CARTESIAN_POINT('Ctrl Pts',(-49.6057233026533,-28.1882175989763,
177.068114089093));
#12990=CARTESIAN_POINT('Ctrl Pts',(-49.5663192275732,-28.1656109096198,
177.105925367078));
#12991=CARTESIAN_POINT('Ctrl Pts',(-49.5216854287654,-28.1457023853521,
177.148383027181));
#12992=CARTESIAN_POINT('Ctrl Pts',(-49.4301127133764,-28.1014695235449,
177.220446553382));
#12993=CARTESIAN_POINT('Ctrl Pts',(-49.3819809603125,-28.0788363277035,
177.253617740645));
#12994=CARTESIAN_POINT('Ctrl Pts',(-49.2321484222821,-28.0099337266433,
177.343479018307));
#12995=CARTESIAN_POINT('Ctrl Pts',(-49.1254026293825,-27.9629901656525,
177.390284377819));
#12996=CARTESIAN_POINT('Ctrl Pts',(-48.7929164986652,-27.8189908160803,
177.48590296908));
#12997=CARTESIAN_POINT('Ctrl Pts',(-48.55635218661,-27.7202377019268,177.490394220553));
#12998=CARTESIAN_POINT('Ctrl Pts',(-47.8840648999533,-27.4305281812212,
177.324447440169));
#12999=CARTESIAN_POINT('Ctrl Pts',(-47.5006474873523,-27.2497443022818,
176.963331771584));
#13000=CARTESIAN_POINT('Ctrl Pts',(-47.2040861213115,-26.9802047380462,
176.046394548579));
#13001=CARTESIAN_POINT('Ctrl Pts',(-47.2954018922066,-26.8917044501032,
175.506598760119));
#13002=CARTESIAN_POINT('Ctrl Pts',(-47.9062028356891,-26.7943163650827,
174.710326627486));
#13003=CARTESIAN_POINT('Ctrl Pts',(-48.4108882632775,-26.7850298620733,
174.47568647468));
#13004=CARTESIAN_POINT('Ctrl Pts',(-49.4081207961382,-26.7654318876047,
174.522051214009));
#13005=CARTESIAN_POINT('Ctrl Pts',(-49.8895805322777,-26.7512165827191,
174.803706734764));
#13006=CARTESIAN_POINT('Ctrl Pts',(-50.419859907048,-26.6406327974915,175.641132157405));
#13007=CARTESIAN_POINT('Ctrl Pts',(-50.4638072135826,-26.5414518590087,
176.190943138814));
#13008=CARTESIAN_POINT('Ctrl Pts',(-50.0902675056585,-26.258306693899,177.06820282525));
#13009=CARTESIAN_POINT('Ctrl Pts',(-49.6753169680471,-26.0710530131776,
177.393289133135));
#13010=CARTESIAN_POINT('Ctrl Pts',(-48.760110273011,-25.6803067135432,177.526354227003));
#13011=CARTESIAN_POINT('Ctrl Pts',(-48.2752065557733,-25.4795815288234,
177.333261554155));
#13012=CARTESIAN_POINT('Ctrl Pts',(-47.6834949732814,-25.1537104488559,
176.598820399841));
#13013=CARTESIAN_POINT('Ctrl Pts',(-47.581935800625,-25.0274199406948,176.066471856633));
#13014=CARTESIAN_POINT('Ctrl Pts',(-47.8743577335121,-24.8702793490883,
175.122570330099));
#13015=CARTESIAN_POINT('Ctrl Pts',(-48.2639300332364,-24.8386062285325,
174.72605490093));
#13016=CARTESIAN_POINT('Ctrl Pts',(-49.2134664973944,-24.8097944361078,
174.418869413643));
#13017=CARTESIAN_POINT('Ctrl Pts',(-49.7639560285487,-24.8089577046691,
174.513086690221));
#13018=CARTESIAN_POINT('Ctrl Pts',(-50.5601436025432,-24.7482854574026,
175.121296078095));
#13019=CARTESIAN_POINT('Ctrl Pts',(-50.7937850628585,-24.6861522884041,
175.625415363842));
#13020=CARTESIAN_POINT('Ctrl Pts',(-50.7513118113109,-24.4660502953853,
176.598470930813));
#13021=CARTESIAN_POINT('Ctrl Pts',(-50.4787452748198,-24.3068424850894,
177.056448064075));
#13022=CARTESIAN_POINT('Ctrl Pts',(-49.6755858463959,-23.9384579984121,
177.525629368769));
#13023=CARTESIAN_POINT('Ctrl Pts',(-49.1583261106009,-23.7318611386462,
177.529378707235));
#13024=CARTESIAN_POINT('Ctrl Pts',(-48.3492917504345,-23.3639427741862,
177.074636497803));
#13025=CARTESIAN_POINT('Ctrl Pts',(-48.0678997211374,-23.2027238239874,
176.620161976926));
#13026=CARTESIAN_POINT('Ctrl Pts',(-48.0133698591323,-22.9779683240005,
175.643265853549));
#13027=CARTESIAN_POINT('Ctrl Pts',(-48.2419634078688,-22.9148026311583,
175.13669620061));
#13028=CARTESIAN_POINT('Ctrl Pts',(-49.0648716087653,-22.8512007031896,
174.491772947554));
#13029=CARTESIAN_POINT('Ctrl Pts',(-49.6839608902416,-22.8528771386521,
174.405900021421));
#13030=CARTESIAN_POINT('Ctrl Pts',(-50.6991943315865,-22.8143164724711,
174.826217042058));
#13031=CARTESIAN_POINT('Ctrl Pts',(-51.0745700439279,-22.7701586995258,
175.322569579276));
#13032=CARTESIAN_POINT('Ctrl Pts',(-51.2073695092728,-22.5604456438022,
176.396956445951));
#13033=CARTESIAN_POINT('Ctrl Pts',(-50.9625278765238,-22.3963905325425,
176.94851178212));
#13034=CARTESIAN_POINT('Ctrl Pts',(-50.1139689940341,-21.9977514714476,
177.529315681618));
#13035=CARTESIAN_POINT('Ctrl Pts',(-49.5293219694751,-21.7666067892758,
177.544699935169));
#13036=CARTESIAN_POINT('Ctrl Pts',(-48.6567664449969,-21.3653910132907,
177.013098304479));
#13037=CARTESIAN_POINT('Ctrl Pts',(-48.383128531039,-21.1949054338945,176.477577858981));
#13038=CARTESIAN_POINT('Ctrl Pts',(-48.4582777380059,-20.975048733324,175.402873064259));
#13039=CARTESIAN_POINT('Ctrl Pts',(-48.8055781932514,-20.9254744005303,
174.886960050279));
#13040=CARTESIAN_POINT('Ctrl Pts',(-49.7998797569528,-20.8818943796597,
174.412232108109));
#13041=CARTESIAN_POINT('Ctrl Pts',(-50.4230224397188,-20.885216808613,174.464849386198));
#13042=CARTESIAN_POINT('Ctrl Pts',(-51.3220781362712,-20.8236066704411,
175.100442044691));
#13043=CARTESIAN_POINT('Ctrl Pts',(-51.5785314568021,-20.7546592125729,
175.670463366294));
#13044=CARTESIAN_POINT('Ctrl Pts',(-51.4682882413066,-20.5004564781585,
176.732562819156));
#13045=CARTESIAN_POINT('Ctrl Pts',(-51.1076577914431,-20.313201754554,177.207532153307));
#13046=CARTESIAN_POINT('Ctrl Pts',(-50.156411198824,-19.8953744930702,177.56803029022));
#13047=CARTESIAN_POINT('Ctrl Pts',(-49.5878400685962,-19.6691878319784,
177.446385146947));
#13048=CARTESIAN_POINT('Ctrl Pts',(-48.852079415717,-19.2920053425884,176.716949064536));
#13049=CARTESIAN_POINT('Ctrl Pts',(-48.7034574890464,-19.1464856081966,
176.127114392609));
#13050=CARTESIAN_POINT('Ctrl Pts',(-49.017896392823,-18.9721498737463,175.084671234462));
#13051=CARTESIAN_POINT('Ctrl Pts',(-49.4761175027563,-18.9421345006494,
174.655217811997));
#13052=CARTESIAN_POINT('Ctrl Pts',(-50.5469446991098,-18.915664221674,174.415005106013));
#13053=CARTESIAN_POINT('Ctrl Pts',(-51.1421889783774,-18.9127734302845,
174.605352538579));
#13054=CARTESIAN_POINT('Ctrl Pts',(-51.8771202801842,-18.8200557591642,
175.418505113175));
#13055=CARTESIAN_POINT('Ctrl Pts',(-52.0018165496213,-18.7275436462981,
176.022835099282));
#13056=CARTESIAN_POINT('Ctrl Pts',(-51.6614363875286,-18.4266465795959,
177.027259608014));
#13057=CARTESIAN_POINT('Ctrl Pts',(-51.2055166082591,-18.2218754080822,
177.403206831321));
#13058=CARTESIAN_POINT('Ctrl Pts',(-50.1969770591628,-17.7923688711786,
177.524973109627));
#13059=CARTESIAN_POINT('Ctrl Pts',(-49.6679526067506,-17.5720619524455,
177.267256975221));
#13060=CARTESIAN_POINT('Ctrl Pts',(-49.1179984398299,-17.2329564925234,
176.379271882249));
#13061=CARTESIAN_POINT('Ctrl Pts',(-49.1058293111544,-17.1129691055462,
175.766207634738));
#13062=CARTESIAN_POINT('Ctrl Pts',(-49.6421979468107,-16.981953011196,174.814805282058));
#13063=CARTESIAN_POINT('Ctrl Pts',(-50.1794692968359,-16.96896833752,174.497498655776));
#13064=CARTESIAN_POINT('Ctrl Pts',(-51.2815033366288,-16.9462509137644,
174.497183387712));
#13065=CARTESIAN_POINT('Ctrl Pts',(-51.8206810039433,-16.9333636766774,
174.813868002799));
#13066=CARTESIAN_POINT('Ctrl Pts',(-52.3579329121243,-16.8019633847227,
175.767995550527));
#13067=CARTESIAN_POINT('Ctrl Pts',(-52.3444015552563,-16.6811074119364,
176.384253300385));
#13068=CARTESIAN_POINT('Ctrl Pts',(-51.7908025496479,-16.3412377353734,
177.270036214878));
#13069=CARTESIAN_POINT('Ctrl Pts',(-51.2640575414935,-16.1220052064028,
177.524939199898));
#13070=CARTESIAN_POINT('Ctrl Pts',(-50.2584821099884,-15.6936926334193,
177.402964762685));
#13071=CARTESIAN_POINT('Ctrl Pts',(-49.8024659570259,-15.4891340123335,
177.028965203342));
#13072=CARTESIAN_POINT('Ctrl Pts',(-49.4615190985809,-15.1881425443655,
176.024838210267));
#13073=CARTESIAN_POINT('Ctrl Pts',(-49.584917871472,-15.0951235636284,175.418993178211));
#13074=CARTESIAN_POINT('Ctrl Pts',(-50.3224323861862,-15.0022736039987,
174.603877612758));
#13075=CARTESIAN_POINT('Ctrl Pts',(-50.9209588419739,-14.9994851008446,
174.413907495741));
#13076=CARTESIAN_POINT('Ctrl Pts',(-51.9913299824675,-14.9728180278691,
174.658436700836));
#13077=CARTESIAN_POINT('Ctrl Pts',(-52.4458562262816,-14.942768055369,175.086526075902));
#13078=CARTESIAN_POINT('Ctrl Pts',(-52.7589234637054,-14.768747576336,176.126312497655));
#13079=CARTESIAN_POINT('Ctrl Pts',(-52.6119738826496,-14.6237809758753,
176.715478760326));
#13080=CARTESIAN_POINT('Ctrl Pts',(-51.8767097042875,-14.2467264136774,
177.445252299972));
#13081=CARTESIAN_POINT('Ctrl Pts',(-51.3074205647036,-14.0201741438431,
177.568755188896));
#13082=CARTESIAN_POINT('Ctrl Pts',(-50.3534291722187,-13.6011459302421,
177.20657523661));
#13083=CARTESIAN_POINT('Ctrl Pts',(-49.9921349812078,-13.4131957453291,
176.728222347554));
#13084=CARTESIAN_POINT('Ctrl Pts',(-49.8860852889645,-13.159806046502,175.66552302478));
#13085=CARTESIAN_POINT('Ctrl Pts',(-50.1425376823364,-13.0914495220188,
175.099033652958));
#13086=CARTESIAN_POINT('Ctrl Pts',(-51.0393482876635,-13.0300320803285,
174.465742160163));
#13087=CARTESIAN_POINT('Ctrl Pts',(-51.661049564308,-13.0333384108268,174.411629490546));
#13088=CARTESIAN_POINT('Ctrl Pts',(-52.6556849728402,-12.9898139344045,
174.885756683857));
#13089=CARTESIAN_POINT('Ctrl Pts',(-53.0050117718212,-12.9403514819039,
175.401975295897));
#13090=CARTESIAN_POINT('Ctrl Pts',(-53.0797917942593,-12.7198628954119,
176.47950485369));
#13091=CARTESIAN_POINT('Ctrl Pts',(-52.8035180796908,-12.5482535501767,
177.017249165378));
#13092=CARTESIAN_POINT('Ctrl Pts',(-51.928756778869,-12.1465816152287,177.545168184464));
#13093=CARTESIAN_POINT('Ctrl Pts',(-51.3476399628683,-11.9168238447545,
177.52855345072));
#13094=CARTESIAN_POINT('Ctrl Pts',(-50.5013329357435,-11.5191203268418,
176.948730973903));
#13095=CARTESIAN_POINT('Ctrl Pts',(-50.2557375091139,-11.3551615877155,
176.398843509589));
#13096=CARTESIAN_POINT('Ctrl Pts',(-50.3877927376681,-11.145398461788,175.324825412843));
#13097=CARTESIAN_POINT('Ctrl Pts',(-50.762684868614,-11.1008426423184,174.826271833705));
#13098=CARTESIAN_POINT('Ctrl Pts',(-51.7811268292925,-11.0622619854364,
174.405264562934));
#13099=CARTESIAN_POINT('Ctrl Pts',(-52.4028793467296,-11.063958202758,174.492793292778));
#13100=CARTESIAN_POINT('Ctrl Pts',(-53.2632154661256,-10.9967409315864,
175.172494096186));
#13101=CARTESIAN_POINT('Ctrl Pts',(-53.4886849878534,-10.9225114509841,
175.750866168407));
#13102=CARTESIAN_POINT('Ctrl Pts',(-53.3251423960266,-10.6565821386363,
176.805379202472));
#13103=CARTESIAN_POINT('Ctrl Pts',(-52.9407422532226,-10.465785944074,177.259010843821));
#13104=CARTESIAN_POINT('Ctrl Pts',(-51.9697953271392,-10.0433159226031,
177.565260787091));
#13105=CARTESIAN_POINT('Ctrl Pts',(-51.4073968434514,-9.81808614025534,
177.411394538556));
#13106=CARTESIAN_POINT('Ctrl Pts',(-50.7116066211125,-9.44884954788431,
176.639139203566));
#13107=CARTESIAN_POINT('Ctrl Pts',(-50.5960828064805,-9.30833579234248,
176.038056438509));
#13108=CARTESIAN_POINT('Ctrl Pts',(-50.9640903737478,-9.14636922546571,
175.0167568496));
#13109=CARTESIAN_POINT('Ctrl Pts',(-51.4414488535671,-9.12058052193367,
174.612974652851));
#13110=CARTESIAN_POINT('Ctrl Pts',(-52.5249204417031,-9.09513784416194,
174.426509843431));
#13111=CARTESIAN_POINT('Ctrl Pts',(-53.1088418277628,-9.09114996369398,
174.646804488947));
#13112=CARTESIAN_POINT('Ctrl Pts',(-53.801661971168,-8.98942785386125,175.498626413927));
#13113=CARTESIAN_POINT('Ctrl Pts',(-53.8945655335682,-8.89052591977855,
176.108945227942));
#13114=CARTESIAN_POINT('Ctrl Pts',(-53.5007325042087,-8.57967938234873,
177.090495387502));
#13115=CARTESIAN_POINT('Ctrl Pts',(-53.0228734977247,-8.36926263084827,
177.439659990072));
#13116=CARTESIAN_POINT('Ctrl Pts',(-52.0134388460396,-7.941561484533,177.502665384752));
#13117=CARTESIAN_POINT('Ctrl Pts',(-51.5009539686643,-7.72503451842822,
177.217498325365));
#13118=CARTESIAN_POINT('Ctrl Pts',(-50.9958226444158,-7.39311721565184,
176.298072843289));
#13119=CARTESIAN_POINT('Ctrl Pts',(-51.0149583411939,-7.28021855779389,
175.684524900703));
#13120=CARTESIAN_POINT('Ctrl Pts',(-51.602189663565,-7.15816051285745,174.759352960774));
#13121=CARTESIAN_POINT('Ctrl Pts',(-52.1561751142271,-7.14821693453925,
174.470064567704));
#13122=CARTESIAN_POINT('Ctrl Pts',(-53.257284967077,-7.12553378294388,174.528734890764));
#13123=CARTESIAN_POINT('Ctrl Pts',(-53.7798318899166,-7.10813319884164,
174.876062446534));
#13124=CARTESIAN_POINT('Ctrl Pts',(-54.263309402104,-6.96831483361839,175.852098283111));
#13125=CARTESIAN_POINT('Ctrl Pts',(-54.2182177005742,-6.84182185515181,
176.463118413));
#13126=CARTESIAN_POINT('Ctrl Pts',(-53.620326169719,-6.49215310837908,177.317242942806));
#13127=CARTESIAN_POINT('Ctrl Pts',(-53.0815432796407,-6.27162057701451,
177.542753252723));
#13128=CARTESIAN_POINT('Ctrl Pts',(-52.0813405764902,-5.84340716815714,
177.363069610828));
#13129=CARTESIAN_POINT('Ctrl Pts',(-51.6451899827477,-5.64252013198273,
176.962963727015));
#13130=CARTESIAN_POINT('Ctrl Pts',(-51.3585173428123,-5.35236886702559,
175.939011043839));
#13131=CARTESIAN_POINT('Ctrl Pts',(-51.5164782073777,-5.2645103327986,175.337256223397));
#13132=CARTESIAN_POINT('Ctrl Pts',(-52.2924300679745,-5.18119763163266,
174.565366155634));
#13133=CARTESIAN_POINT('Ctrl Pts',(-52.8973452213176,-5.1801045826173,174.406680096152));
#13134=CARTESIAN_POINT('Ctrl Pts',(-53.956162505713,-5.14973256956073,174.705214074754));
#13135=CARTESIAN_POINT('Ctrl Pts',(-54.3874707400874,-5.11629663400306,
175.155234787811));
#13136=CARTESIAN_POINT('Ctrl Pts',(-54.6460006492434,-4.93091655090319,
176.210608238885));
#13137=CARTESIAN_POINT('Ctrl Pts',(-54.4681690759566,-4.77980797892323,
176.790635503925));
#13138=CARTESIAN_POINT('Ctrl Pts',(-53.6946945331643,-4.3956772156615,177.47627897342));
#13139=CARTESIAN_POINT('Ctrl Pts',(-53.1174419759953,-4.16620647621949,
177.565792133827));
#13140=CARTESIAN_POINT('Ctrl Pts',(-52.1878574222778,-3.75385530866336,
177.150829002666));
#13141=CARTESIAN_POINT('Ctrl Pts',(-51.8529856411974,-3.5715083216093,176.654958973924));
#13142=CARTESIAN_POINT('Ctrl Pts',(-51.8010050251376,-3.32706416715232,
175.583828138226));
#13143=CARTESIAN_POINT('Ctrl Pts',(-52.0854219579878,-3.26527816982496,
175.031488604324));
#13144=CARTESIAN_POINT('Ctrl Pts',(-53.0170398348192,-3.20959915076688,
174.444132662069));
#13145=CARTESIAN_POINT('Ctrl Pts',(-53.6416591927321,-3.21325709639781,
174.423035709656));
#13146=CARTESIAN_POINT('Ctrl Pts',(-54.6090153740635,-3.16498595686182,
174.948967905512));
#13147=CARTESIAN_POINT('Ctrl Pts',(-54.9308286711417,-3.10893139642228,
175.48555871107));
#13148=CARTESIAN_POINT('Ctrl Pts',(-54.9426665516143,-2.95192631073098,
176.218540695264));
#13149=CARTESIAN_POINT('Ctrl Pts',(-54.9070365263685,-2.90171640292054,
176.413787336324));
#13150=CARTESIAN_POINT('Ctrl Pts',(-54.8013987998623,-2.81782847468563,
176.681821034794));
#13151=CARTESIAN_POINT('Ctrl Pts',(-54.7570848510793,-2.78787367953458,
176.767627228561));
#13152=CARTESIAN_POINT('Ctrl Pts',(-54.6793253219128,-2.74078668455889,
176.887592985838));
#13153=CARTESIAN_POINT('Ctrl Pts',(-54.651529701944,-2.72473899696222,176.926133356148));
#13154=CARTESIAN_POINT('Ctrl Pts',(-54.5925997439423,-2.69209575899625,
176.999824075839));
#13155=CARTESIAN_POINT('Ctrl Pts',(-54.5641015373143,-2.67654794454284,
177.031971691023));
#13156=CARTESIAN_POINT('Ctrl Pts',(-54.5288628436534,-2.65870383148503,
177.068203177065));
#13157=CARTESIAN_POINT('Ctrl Pts',(-49.7605161567837,-28.8447111186158,
177.498294784826));
#13158=CARTESIAN_POINT('Ctrl Pts',(-49.703499066658,-28.8235655424673,177.540214005203));
#13159=CARTESIAN_POINT('Ctrl Pts',(-49.6410455761305,-28.7951782353542,
177.600452889938));
#13160=CARTESIAN_POINT('Ctrl Pts',(-49.5125749804916,-28.7439261033728,
177.690427833332));
#13161=CARTESIAN_POINT('Ctrl Pts',(-49.4455382815264,-28.7177519743038,
177.731297783696));
#13162=CARTESIAN_POINT('Ctrl Pts',(-49.2376911387288,-28.6378112833129,
177.840935439774));
#13163=CARTESIAN_POINT('Ctrl Pts',(-49.0899159828253,-28.5824382846613,
177.897035937477));
#13164=CARTESIAN_POINT('Ctrl Pts',(-48.6337896696199,-28.4146446752159,
178.002589339604));
#13165=CARTESIAN_POINT('Ctrl Pts',(-48.3132270959126,-28.2997217083806,
177.992428880102));
#13166=CARTESIAN_POINT('Ctrl Pts',(-47.4162097247782,-27.9673749676665,
177.725331904959));
#13167=CARTESIAN_POINT('Ctrl Pts',(-46.9189492851719,-27.7652251395226,
177.218083285283));
#13168=CARTESIAN_POINT('Ctrl Pts',(-46.5632291525645,-27.4820421855238,
175.966063107167));
#13169=CARTESIAN_POINT('Ctrl Pts',(-46.7140098167225,-27.4055520605101,
175.249184591433));
#13170=CARTESIAN_POINT('Ctrl Pts',(-47.566085933826,-27.3558389712614,174.223160308952));
#13171=CARTESIAN_POINT('Ctrl Pts',(-48.2470586621674,-27.3810915115113,
173.939995635501));
#13172=CARTESIAN_POINT('Ctrl Pts',(-49.5700361455588,-27.4220834505067,
174.062399212278));
#13173=CARTESIAN_POINT('Ctrl Pts',(-50.1884067287968,-27.434811958294,174.470377906696));
#13174=CARTESIAN_POINT('Ctrl Pts',(-50.8303308863031,-27.3468909642006,
175.620618298056));
#13175=CARTESIAN_POINT('Ctrl Pts',(-50.8493116919004,-27.2434061722865,
176.356125167609));
#13176=CARTESIAN_POINT('Ctrl Pts',(-50.2816569479994,-26.9206929510016,
177.507808537998));
#13177=CARTESIAN_POINT('Ctrl Pts',(-49.6987348616025,-26.7015350212598,
177.912925525668));
#13178=CARTESIAN_POINT('Ctrl Pts',(-48.454710251186,-26.2485207329848,178.028292067179));
#13179=CARTESIAN_POINT('Ctrl Pts',(-47.8121824616331,-26.017945810327,177.739239128205));
#13180=CARTESIAN_POINT('Ctrl Pts',(-47.0491566977328,-25.6568136786021,
176.713556301102));
#13181=CARTESIAN_POINT('Ctrl Pts',(-46.9415518318806,-25.5298970910749,
175.993584668982));
#13182=CARTESIAN_POINT('Ctrl Pts',(-47.3778834474909,-25.4016448622981,
174.749674324357));
#13183=CARTESIAN_POINT('Ctrl Pts',(-47.9149438708112,-25.3989201973124,
174.243242130538));
#13184=CARTESIAN_POINT('Ctrl Pts',(-49.195098595239,-25.4317364372956,173.888113334518));
#13185=CARTESIAN_POINT('Ctrl Pts',(-49.918185567551,-25.4646653275392,174.050133776974));
#13186=CARTESIAN_POINT('Ctrl Pts',(-50.9295131393841,-25.4466210128473,
174.911633886668));
#13187=CARTESIAN_POINT('Ctrl Pts',(-51.2044913533823,-25.3930064438348,
175.597822621196));
#13188=CARTESIAN_POINT('Ctrl Pts',(-51.0754639563939,-25.1539869007477,
176.899089439364));
#13189=CARTESIAN_POINT('Ctrl Pts',(-50.6742118208058,-24.9705041413757,
177.491449801663));
#13190=CARTESIAN_POINT('Ctrl Pts',(-49.5587075034334,-24.5430242840169,
178.062955652865));
#13191=CARTESIAN_POINT('Ctrl Pts',(-48.8611723259578,-24.3021716495128,
178.034645386427));
#13192=CARTESIAN_POINT('Ctrl Pts',(-47.7896195282427,-23.8814983836082,
177.370866230542));
#13193=CARTESIAN_POINT('Ctrl Pts',(-47.4363508410467,-23.7069028048269,
176.742728542957));
#13194=CARTESIAN_POINT('Ctrl Pts',(-47.4114253180649,-23.4889969329168,
175.432113003805));
#13195=CARTESIAN_POINT('Ctrl Pts',(-47.740070725129,-23.4456714422117,174.768834597493));
#13196=CARTESIAN_POINT('Ctrl Pts',(-48.8702204177861,-23.4389819923271,
173.952056567371));
#13197=CARTESIAN_POINT('Ctrl Pts',(-49.6947930376395,-23.4814638927378,
173.877925688461));
#13198=CARTESIAN_POINT('Ctrl Pts',(-51.0112605873021,-23.5013279450334,
174.502758507842));
#13199=CARTESIAN_POINT('Ctrl Pts',(-51.4766740890821,-23.4736078700863,
175.190881305064));
#13200=CARTESIAN_POINT('Ctrl Pts',(-51.5715098854918,-23.2578265151817,
176.631332013987));
#13201=CARTESIAN_POINT('Ctrl Pts',(-51.2026984232359,-23.0689810535093,
177.353708555585));
#13202=CARTESIAN_POINT('Ctrl Pts',(-50.0169981786826,-22.6055963153184,
178.072791197941));
#13203=CARTESIAN_POINT('Ctrl Pts',(-49.2289032454779,-22.3364394885883,
178.054791801573));
#13204=CARTESIAN_POINT('Ctrl Pts',(-48.0752306219957,-21.8785657833076,
177.283552800795));
#13205=CARTESIAN_POINT('Ctrl Pts',(-47.7373875210752,-21.6968802590999,
176.548566639058));
#13206=CARTESIAN_POINT('Ctrl Pts',(-47.8901343487967,-21.492320838371,175.113663385513));
#13207=CARTESIAN_POINT('Ctrl Pts',(-48.3804128007365,-21.4693940830233,
174.442825661914));
#13208=CARTESIAN_POINT('Ctrl Pts',(-49.7230759786915,-21.4942443138953,
173.870938911605));
#13209=CARTESIAN_POINT('Ctrl Pts',(-50.5477501626655,-21.53554466513,173.979304242753));
#13210=CARTESIAN_POINT('Ctrl Pts',(-51.6956775721548,-21.5221965965903,
174.884495307656));
#13211=CARTESIAN_POINT('Ctrl Pts',(-51.995185395164,-21.4627711751308,175.65946330393));
#13212=CARTESIAN_POINT('Ctrl Pts',(-51.7684808698132,-21.1836626405178,
177.075777271268));
#13213=CARTESIAN_POINT('Ctrl Pts',(-51.248410167092,-20.9668436684778,177.683928269078));
#13214=CARTESIAN_POINT('Ctrl Pts',(-49.9393032270381,-20.4803392816045,
178.101596183419));
#13215=CARTESIAN_POINT('Ctrl Pts',(-49.1773119956809,-20.2159303489599,
177.900701030808));
#13216=CARTESIAN_POINT('Ctrl Pts',(-48.2258296454727,-19.7984008812386,
176.875814996871));
#13217=CARTESIAN_POINT('Ctrl Pts',(-48.0552229745052,-19.6477554978605,
176.074637438704));
#13218=CARTESIAN_POINT('Ctrl Pts',(-48.5258258225559,-19.5038059294262,
174.698094313544));
#13219=CARTESIAN_POINT('Ctrl Pts',(-49.1555523948045,-19.5080820109078,
174.15313676254));
#13220=CARTESIAN_POINT('Ctrl Pts',(-50.5933891726929,-19.5499376382275,
173.895161972129));
#13221=CARTESIAN_POINT('Ctrl Pts',(-51.368058411907,-19.5828296420673,174.188177381599));
#13222=CARTESIAN_POINT('Ctrl Pts',(-52.285250485287,-19.5255903568737,175.320127767442));
#13223=CARTESIAN_POINT('Ctrl Pts',(-52.4079017329002,-19.4317611692977,
176.136959370172));
#13224=CARTESIAN_POINT('Ctrl Pts',(-51.8753008807154,-19.0950488584311,
177.453114298066));
#13225=CARTESIAN_POINT('Ctrl Pts',(-51.2342686483785,-18.8536936439763,
177.926872571079));
#13226=CARTESIAN_POINT('Ctrl Pts',(-49.8632157867063,-18.3545541183897,
178.021760725256));
#13227=CARTESIAN_POINT('Ctrl Pts',(-49.1660096364335,-18.1030331017558,
177.643137201611));
#13228=CARTESIAN_POINT('Ctrl Pts',(-48.4670297183309,-17.7327410070788,
176.413682699456));
#13229=CARTESIAN_POINT('Ctrl Pts',(-48.483334940274,-17.6194284897493,175.592916154309));
#13230=CARTESIAN_POINT('Ctrl Pts',(-49.2450668681383,-17.5322013902257,
174.352697167155));
#13231=CARTESIAN_POINT('Ctrl Pts',(-49.9777722871607,-17.5559821453049,
173.960304681794));
#13232=CARTESIAN_POINT('Ctrl Pts',(-51.4344516507071,-17.6029063882428,
174.028937019837));
#13233=CARTESIAN_POINT('Ctrl Pts',(-52.1305828574604,-17.6193975644539,
174.485906049309));
#13234=CARTESIAN_POINT('Ctrl Pts',(-52.774838706301,-17.5089074046146,175.793694056009));
#13235=CARTESIAN_POINT('Ctrl Pts',(-52.7115258732458,-17.3796686755426,
176.613178448276));
#13236=CARTESIAN_POINT('Ctrl Pts',(-51.9002446822929,-16.9876585431162,
177.764926590858));
#13237=CARTESIAN_POINT('Ctrl Pts',(-51.1728057089079,-16.7309097600974,
178.068009087089));
#13238=CARTESIAN_POINT('Ctrl Pts',(-49.8211348979667,-16.2361848829689,
177.837068581403));
#13239=CARTESIAN_POINT('Ctrl Pts',(-49.2256314668982,-16.0038069200319,
177.305047152795));
#13240=CARTESIAN_POINT('Ctrl Pts',(-48.8186328386387,-15.691330495564,175.939125806104));
#13241=CARTESIAN_POINT('Ctrl Pts',(-49.013546517339,-15.6112127223192,175.133605172695));
#13242=CARTESIAN_POINT('Ctrl Pts',(-50.0357499087345,-15.5735396207079,
174.088389632472));
#13243=CARTESIAN_POINT('Ctrl Pts',(-50.8379174497137,-15.6112366284576,
173.871670522767));
#13244=CARTESIAN_POINT('Ctrl Pts',(-52.2457834487726,-15.6472027358935,
174.26447248136));
#13245=CARTESIAN_POINT('Ctrl Pts',(-52.8170337247495,-15.6408479370702,
174.8653310014));
#13246=CARTESIAN_POINT('Ctrl Pts',(-53.1560440051794,-15.4721566908598,
176.273031298879));
#13247=CARTESIAN_POINT('Ctrl Pts',(-52.9154253174859,-15.3082073561117,
177.052126824288));
#13248=CARTESIAN_POINT('Ctrl Pts',(-51.8728096300678,-14.8731360568539,
177.975770830197));
#13249=CARTESIAN_POINT('Ctrl Pts',(-51.0951645133176,-14.6055143185424,
178.104087436367));
#13250=CARTESIAN_POINT('Ctrl Pts',(-49.8271933090145,-14.1262171391814,
177.555333624295));
#13251=CARTESIAN_POINT('Ctrl Pts',(-49.3671436709228,-13.9204374671742,
176.893150416479));
#13252=CARTESIAN_POINT('Ctrl Pts',(-49.274728926638,-13.6672296225191,175.457007277905));
#13253=CARTESIAN_POINT('Ctrl Pts',(-49.6465886024413,-13.6223148063404,
174.716642572685));
#13254=CARTESIAN_POINT('Ctrl Pts',(-50.8704338551746,-13.6242867085274,
173.925061362222));
#13255=CARTESIAN_POINT('Ctrl Pts',(-51.7000786840932,-13.666773744136,173.890948850678));
#13256=CARTESIAN_POINT('Ctrl Pts',(-52.983493848767,-13.6801901085456,174.58610021153));
#13257=CARTESIAN_POINT('Ctrl Pts',(-53.4130967944053,-13.6453172862449,
175.298527478907));
#13258=CARTESIAN_POINT('Ctrl Pts',(-53.4312271360186,-13.4141834163833,
176.741466379681));
#13259=CARTESIAN_POINT('Ctrl Pts',(-53.0223631213944,-13.2182197961852,
177.439586265974));
#13260=CARTESIAN_POINT('Ctrl Pts',(-51.8015717929752,-12.7473718779738,
178.090703687822));
#13261=CARTESIAN_POINT('Ctrl Pts',(-51.0193050555008,-12.4800112867217,
178.027617006182));
#13262=CARTESIAN_POINT('Ctrl Pts',(-49.9091230827754,-12.0317475039094,
177.194798446979));
#13263=CARTESIAN_POINT('Ctrl Pts',(-49.6065982226317,-11.8558917537395,
176.440442987632));
#13264=CARTESIAN_POINT('Ctrl Pts',(-49.8356019855053,-11.6660764580159,
175.012059004046));
#13265=CARTESIAN_POINT('Ctrl Pts',(-50.3610430198266,-11.6496605652263,
174.366149315963));
#13266=CARTESIAN_POINT('Ctrl Pts',(-51.7343806490719,-11.6797988495863,
173.866104995302));
#13267=CARTESIAN_POINT('Ctrl Pts',(-52.550540790582,-11.7201981252995,174.02088411371));
#13268=CARTESIAN_POINT('Ctrl Pts',(-53.6500640270725,-11.6966559909963,
174.984749041133));
#13269=CARTESIAN_POINT('Ctrl Pts',(-53.9056865612328,-11.6294298688172,
175.770695352483));
#13270=CARTESIAN_POINT('Ctrl Pts',(-53.6065172861421,-11.3376692947806,
177.167270913611));
#13271=CARTESIAN_POINT('Ctrl Pts',(-53.0559160748103,-11.1139055956972,
177.749439639131));
#13272=CARTESIAN_POINT('Ctrl Pts',(-51.7252371686403,-10.6233177496803,
178.092170345976));
#13273=CARTESIAN_POINT('Ctrl Pts',(-50.9736524019596,-10.3607126008384,
177.849203208466));
#13274=CARTESIAN_POINT('Ctrl Pts',(-50.0765013772471,-9.95292884744916,
176.76875224789));
#13275=CARTESIAN_POINT('Ctrl Pts',(-49.9516819265813,-9.81183425780667,
175.958513771998));
#13276=CARTESIAN_POINT('Ctrl Pts',(-50.4932223958658,-9.68088414604229,
174.607725553029));
#13277=CARTESIAN_POINT('Ctrl Pts',(-51.1493491071183,-9.69075789692425,
174.099564788001));
#13278=CARTESIAN_POINT('Ctrl Pts',(-52.5949212007306,-9.73546275490891,
173.917493057606));
#13279=CARTESIAN_POINT('Ctrl Pts',(-53.3569613223681,-9.76490646019358,
174.248860303054));
#13280=CARTESIAN_POINT('Ctrl Pts',(-54.2135986647274,-9.69602761498083,
175.428657754819));
#13281=CARTESIAN_POINT('Ctrl Pts',(-54.293848370144,-9.59379233086061,176.251060243097));
#13282=CARTESIAN_POINT('Ctrl Pts',(-53.6913007216372,-9.24298063305673,
177.535379997424));
#13283=CARTESIAN_POINT('Ctrl Pts',(-53.0251793740895,-8.99747173235245,
177.96924977839));
#13284=CARTESIAN_POINT('Ctrl Pts',(-51.651725273033,-8.49712492600163,177.987723094373));
#13285=CARTESIAN_POINT('Ctrl Pts',(-50.9786512815054,-8.25081939601668,
177.570771429869));
#13286=CARTESIAN_POINT('Ctrl Pts',(-50.3458167934762,-7.89459730610716,
176.305935969218));
#13287=CARTESIAN_POINT('Ctrl Pts',(-50.4021522245058,-7.78795543802409,
175.483191418641));
#13288=CARTESIAN_POINT('Ctrl Pts',(-51.2295886328818,-7.71347110197539,
174.283262770515));
#13289=CARTESIAN_POINT('Ctrl Pts',(-51.9823539758956,-7.74096536711586,
173.929068927273));
#13290=CARTESIAN_POINT('Ctrl Pts',(-53.4363603166253,-7.78662015021704,
174.075813689628));
#13291=CARTESIAN_POINT('Ctrl Pts',(-54.1043459363082,-7.79847651244032,
174.570723179108));
#13292=CARTESIAN_POINT('Ctrl Pts',(-54.6799658608561,-7.67397811007903,
175.90877571489));
#13293=CARTESIAN_POINT('Ctrl Pts',(-54.5722464428634,-7.53659878310187,
176.719948913595));
#13294=CARTESIAN_POINT('Ctrl Pts',(-53.7048106882453,-7.13527023180301,
177.820508243663));
#13295=CARTESIAN_POINT('Ctrl Pts',(-52.9613211614002,-6.87434685741961,
178.086941994317));
#13296=CARTESIAN_POINT('Ctrl Pts',(-51.6221407922901,-6.38201846097514,
177.778890662373));
#13297=CARTESIAN_POINT('Ctrl Pts',(-51.0546870579556,-6.15491662175662,
177.213869145202));
#13298=CARTESIAN_POINT('Ctrl Pts',(-50.7203127232504,-5.85585141799114,
175.823263107997));
#13299=CARTESIAN_POINT('Ctrl Pts',(-50.9602054908589,-5.78500310757108,
175.029480964866));
#13300=CARTESIAN_POINT('Ctrl Pts',(-52.0343424634976,-5.75674450428783,
174.039165918607));
#13301=CARTESIAN_POINT('Ctrl Pts',(-52.8447329543179,-5.79646505952858,
173.866867743832));
#13302=CARTESIAN_POINT('Ctrl Pts',(-54.227093102642,-5.82880399980787,174.331684606762));
#13303=CARTESIAN_POINT('Ctrl Pts',(-54.7703330160768,-5.81603743040407,
174.961265757845));
#13304=CARTESIAN_POINT('Ctrl Pts',(-55.0342584322448,-5.63295034503888,
176.384531023624));
#13305=CARTESIAN_POINT('Ctrl Pts',(-54.7535167216846,-5.46110103683509,
177.149304158576));
#13306=CARTESIAN_POINT('Ctrl Pts',(-53.6617191466184,-5.01587299208642,
178.013397713687));
#13307=CARTESIAN_POINT('Ctrl Pts',(-52.8789563910228,-4.7479816344422,178.094733745787));
#13308=CARTESIAN_POINT('Ctrl Pts',(-51.6416463903481,-4.27383996939189,
177.476508505419));
#13309=CARTESIAN_POINT('Ctrl Pts',(-51.2194660036301,-4.07584859930261,
176.790317421121));
#13310=CARTESIAN_POINT('Ctrl Pts',(-51.2019938075703,-3.83837584139065,
175.351935740118));
#13311=CARTESIAN_POINT('Ctrl Pts',(-51.610208243602,-3.79954787084599,174.628251672824));
#13312=CARTESIAN_POINT('Ctrl Pts',(-52.8762543405249,-3.80961476365013,
173.901884637809));
#13313=CARTESIAN_POINT('Ctrl Pts',(-53.7073988028502,-3.85223555101975,
173.911595161346));
#13314=CARTESIAN_POINT('Ctrl Pts',(-54.9534921954892,-3.85792953287916,
174.67446559102));
#13315=CARTESIAN_POINT('Ctrl Pts',(-55.3426629917145,-3.81570008082077,
175.409213860003));
#13316=CARTESIAN_POINT('Ctrl Pts',(-55.3039033258818,-3.64772468214507,
176.391662012851));
#13317=CARTESIAN_POINT('Ctrl Pts',(-55.240555748585,-3.59330136077634,176.648581151648));
#13318=CARTESIAN_POINT('Ctrl Pts',(-55.0788320999402,-3.49759375703432,
177.001372563377));
#13319=CARTESIAN_POINT('Ctrl Pts',(-55.0131335998823,-3.46357400887706,
177.112553347482));
#13320=CARTESIAN_POINT('Ctrl Pts',(-54.8999581434668,-3.40984365170443,
177.267014142137));
#13321=CARTESIAN_POINT('Ctrl Pts',(-54.8598034384417,-3.39148030846876,
177.316464483235));
#13322=CARTESIAN_POINT('Ctrl Pts',(-54.7750771562006,-3.35389509449369,
177.410924972696));
#13323=CARTESIAN_POINT('Ctrl Pts',(-54.7397209311609,-3.33918794957438,
177.445275075635));
#13324=CARTESIAN_POINT('Ctrl Pts',(-54.6838989306507,-3.31503673670408,
177.498541333932));
#13325=CARTESIAN_POINT('Ctrl Pts',(-50.3479071748434,-28.4569951884828,
177.87862115707));
#13326=CARTESIAN_POINT('Ctrl Pts',(-50.2728575672733,-28.4359962578257,
177.948540001849));
#13327=CARTESIAN_POINT('Ctrl Pts',(-50.1962258409275,-28.4010191615162,
178.021251708215));
#13328=CARTESIAN_POINT('Ctrl Pts',(-50.0327133344336,-28.3431284715803,
178.148112768101));
#13329=CARTESIAN_POINT('Ctrl Pts',(-49.9471957757512,-28.3135226108735,
178.206264690109));
#13330=CARTESIAN_POINT('Ctrl Pts',(-49.6807194301921,-28.2224721023673,
178.364232700982));
#13331=CARTESIAN_POINT('Ctrl Pts',(-49.4886308694229,-28.1579103591893,
178.447943211646));
#13332=CARTESIAN_POINT('Ctrl Pts',(-48.8935956196606,-27.9633647516093,
178.618732735728));
#13333=CARTESIAN_POINT('Ctrl Pts',(-48.4698811368596,-27.8285932845993,
178.628088311833));
#13334=CARTESIAN_POINT('Ctrl Pts',(-47.2704244122812,-27.4388125604887,
178.343093993075));
#13335=CARTESIAN_POINT('Ctrl Pts',(-46.5780488855805,-27.1997688494767,
177.716319207522));
#13336=CARTESIAN_POINT('Ctrl Pts',(-46.0180477417519,-26.8743979377982,
176.099249510754));
#13337=CARTESIAN_POINT('Ctrl Pts',(-46.162624656611,-26.7973830650002,175.153557109113));
#13338=CARTESIAN_POINT('Ctrl Pts',(-47.1953010051746,-26.7839304768722,
173.755742992678));
#13339=CARTESIAN_POINT('Ctrl Pts',(-48.0607153645256,-26.8454387863112,
173.337748493251));
#13340=CARTESIAN_POINT('Ctrl Pts',(-49.7936242958811,-26.9626978867657,
173.412243144396));
#13341=CARTESIAN_POINT('Ctrl Pts',(-50.6218862360795,-27.016572452629,173.905326198308));
#13342=CARTESIAN_POINT('Ctrl Pts',(-51.5258205855669,-26.9805930176338,
175.367177784907));
#13343=CARTESIAN_POINT('Ctrl Pts',(-51.5951438365624,-26.8874613833773,
176.329869003407));
#13344=CARTESIAN_POINT('Ctrl Pts',(-50.9127162462792,-26.5399486517808,
177.882574589842));
#13345=CARTESIAN_POINT('Ctrl Pts',(-50.1707795944383,-26.2907274748939,
178.452449051012));
#13346=CARTESIAN_POINT('Ctrl Pts',(-48.5397246316051,-25.7645038790956,
178.692502082553));
#13347=CARTESIAN_POINT('Ctrl Pts',(-47.67260524551,-25.4913101058597,178.361691922331));
#13348=CARTESIAN_POINT('Ctrl Pts',(-46.5924693917267,-25.0662449204663,
177.069022085109));
#13349=CARTESIAN_POINT('Ctrl Pts',(-46.3991806471167,-24.9234731673228,
176.136653590829));
#13350=CARTESIAN_POINT('Ctrl Pts',(-46.8738389297659,-24.8040321200569,
174.482872284355));
#13351=CARTESIAN_POINT('Ctrl Pts',(-47.5355683392896,-24.8259889159373,
173.783025779917));
#13352=CARTESIAN_POINT('Ctrl Pts',(-49.181078144729,-24.926602323961,173.233424036193));
#13353=CARTESIAN_POINT('Ctrl Pts',(-50.130455303743,-25.0037631556439,173.398086820976));
#13354=CARTESIAN_POINT('Ctrl Pts',(-51.4978889309697,-25.0558147041254,
174.456799989093));
#13355=CARTESIAN_POINT('Ctrl Pts',(-51.8989353348306,-25.0272033256972,
175.336539369917));
#13356=CARTESIAN_POINT('Ctrl Pts',(-51.8018863283238,-24.7915666340119,
177.05629857501));
#13357=CARTESIAN_POINT('Ctrl Pts',(-51.3095767986978,-24.5911935663349,
177.858613821852));
#13358=CARTESIAN_POINT('Ctrl Pts',(-49.8771546536489,-24.10401978861,178.68604557473));
#13359=CARTESIAN_POINT('Ctrl Pts',(-48.9560458718938,-23.8206956072764,
178.700341600297));
#13360=CARTESIAN_POINT('Ctrl Pts',(-47.4944002604164,-23.3221357921539,
177.903717692127));
#13361=CARTESIAN_POINT('Ctrl Pts',(-46.9859140286074,-23.1182050059858,
177.107706307993));
#13362=CARTESIAN_POINT('Ctrl Pts',(-46.8530474021693,-22.8809089149922,
175.398792520737));
#13363=CARTESIAN_POINT('Ctrl Pts',(-47.231059536602,-22.8477944049951,174.508609012772));
#13364=CARTESIAN_POINT('Ctrl Pts',(-48.6493873331158,-22.8937567040743,
173.363150661036));
#13365=CARTESIAN_POINT('Ctrl Pts',(-49.7143921444323,-22.9840542321675,
173.211662996139));
#13366=CARTESIAN_POINT('Ctrl Pts',(-51.4652368913311,-23.0881428692961,
173.941607840096));
#13367=CARTESIAN_POINT('Ctrl Pts',(-52.1136094605607,-23.094525291844,174.813935779811));
#13368=CARTESIAN_POINT('Ctrl Pts',(-52.3204663109761,-22.9019098705719,
176.69350767169));
#13369=CARTESIAN_POINT('Ctrl Pts',(-51.877821743202,-22.6977464609932,177.66752824204));
#13370=CARTESIAN_POINT('Ctrl Pts',(-50.3601753662095,-22.1706433373772,
178.693383453661));
#13371=CARTESIAN_POINT('Ctrl Pts',(-49.3218325614145,-21.8547798388568,
178.72781114664));
#13372=CARTESIAN_POINT('Ctrl Pts',(-47.7441093775104,-21.3120724766084,
177.795709587611));
#13373=CARTESIAN_POINT('Ctrl Pts',(-47.2477760409393,-21.1012761066736,
176.860414332907));
#13374=CARTESIAN_POINT('Ctrl Pts',(-47.3387825873497,-20.8852685243919,
174.97505816188));
#13375=CARTESIAN_POINT('Ctrl Pts',(-47.9314309575524,-20.8809046965219,
174.063915635121));
#13376=CARTESIAN_POINT('Ctrl Pts',(-49.6347357453554,-20.9768646680186,
173.225964829082));
#13377=CARTESIAN_POINT('Ctrl Pts',(-50.7167240875825,-21.0667038014875,
173.313184970442));
#13378=CARTESIAN_POINT('Ctrl Pts',(-52.2657610285106,-21.1310010461024,
174.421840220958));
#13379=CARTESIAN_POINT('Ctrl Pts',(-52.7037384700293,-21.0998274566763,
175.41493210957));
#13380=CARTESIAN_POINT('Ctrl Pts',(-52.4847175837037,-20.8191405044519,
177.292562937125));
#13381=CARTESIAN_POINT('Ctrl Pts',(-51.8386241308113,-20.5794725658491,
178.12361350116));
#13382=CARTESIAN_POINT('Ctrl Pts',(-50.1396663396365,-20.018246073474,178.763454537015));
#13383=CARTESIAN_POINT('Ctrl Pts',(-49.1209540205185,-19.7031542981699,
178.552891694314));
#13384=CARTESIAN_POINT('Ctrl Pts',(-47.794702927651,-19.2149188701855,177.282197399313));
#13385=CARTESIAN_POINT('Ctrl Pts',(-47.5115450575125,-19.0414866308731,
176.244710688925));
#13386=CARTESIAN_POINT('Ctrl Pts',(-48.0225076992042,-18.9056180257745,
174.413639337664));
#13387=CARTESIAN_POINT('Ctrl Pts',(-48.8010517900779,-18.9401402740231,
173.657816206187));
#13388=CARTESIAN_POINT('Ctrl Pts',(-50.6589325202962,-19.0599362479824,
173.225466551806));
#13389=CARTESIAN_POINT('Ctrl Pts',(-51.6828783925415,-19.1423524153639,
173.556811131415));
#13390=CARTESIAN_POINT('Ctrl Pts',(-52.94490571859,-19.1520660317591,174.977944054317));
#13391=CARTESIAN_POINT('Ctrl Pts',(-53.1522316495948,-19.0733891332466,
176.042129261136));
#13392=CARTESIAN_POINT('Ctrl Pts',(-52.5304975170958,-18.7210523123868,
177.802820234119));
#13393=CARTESIAN_POINT('Ctrl Pts',(-51.7144732100097,-18.4448678812944,
178.469420248747));
#13394=CARTESIAN_POINT('Ctrl Pts',(-49.9127782169188,-17.8629843097264,
178.691085462265));
#13395=CARTESIAN_POINT('Ctrl Pts',(-48.9683571282271,-17.5653381811437,
178.247635108413));
#13396=CARTESIAN_POINT('Ctrl Pts',(-47.9579076603942,-17.1319211116872,
176.683402031933));
#13397=CARTESIAN_POINT('Ctrl Pts',(-47.9184077060768,-17.009302655329,175.611974434002));
#13398=CARTESIAN_POINT('Ctrl Pts',(-48.8193204272181,-16.9493687678545,
173.939410793842));
#13399=CARTESIAN_POINT('Ctrl Pts',(-49.7479148095836,-17.0097492793151,
173.377008912436));
#13400=CARTESIAN_POINT('Ctrl Pts',(-51.643208967551,-17.1428193004232,173.368498519432));
#13401=CARTESIAN_POINT('Ctrl Pts',(-52.5796094505093,-17.2045582837911,
173.921665784702));
#13402=CARTESIAN_POINT('Ctrl Pts',(-53.4961681928706,-17.1468816411331,
175.591939966795));
#13403=CARTESIAN_POINT('Ctrl Pts',(-53.4629851797616,-17.024999612415,176.669185388437));
#13404=CARTESIAN_POINT('Ctrl Pts',(-52.4593346223015,-16.5928308404044,
178.238747171052));
#13405=CARTESIAN_POINT('Ctrl Pts',(-51.5224253668316,-16.2971453030902,
178.685547111838));
#13406=CARTESIAN_POINT('Ctrl Pts',(-49.7246467734476,-15.7168449309467,
178.479497386489));
#13407=CARTESIAN_POINT('Ctrl Pts',(-48.9027009029283,-15.4396261238498,
177.823563805929));
#13408=CARTESIAN_POINT('Ctrl Pts',(-48.2654141259822,-15.0843052308904,
176.069175886686));
#13409=CARTESIAN_POINT('Ctrl Pts',(-48.4613159716259,-15.0032908855178,
175.000998038449));
#13410=CARTESIAN_POINT('Ctrl Pts',(-49.7162174501553,-15.01079667333,173.565578406105));
#13411=CARTESIAN_POINT('Ctrl Pts',(-50.7428205977302,-15.0933182852754,
173.226451476554));
#13412=CARTESIAN_POINT('Ctrl Pts',(-52.6035006910652,-15.2135426682566,
173.650512878487));
#13413=CARTESIAN_POINT('Ctrl Pts',(-53.382025542189,-15.2486168447941,174.397702687793));
#13414=CARTESIAN_POINT('Ctrl Pts',(-53.905727267535,-15.1159903036539,176.219573585739));
#13415=CARTESIAN_POINT('Ctrl Pts',(-53.6343010604909,-14.9449274325696,
177.258764585683));
#13416=CARTESIAN_POINT('Ctrl Pts',(-52.3195045847479,-14.4589334435455,
178.541768722646));
#13417=CARTESIAN_POINT('Ctrl Pts',(-51.3015568868895,-14.1438839803641,
178.764698457169));
#13418=CARTESIAN_POINT('Ctrl Pts',(-49.5920248617255,-13.5797433288121,
178.136857041975));
#13419=CARTESIAN_POINT('Ctrl Pts',(-48.9380275082558,-13.3381062047143,
177.30578604004));
#13420=CARTESIAN_POINT('Ctrl Pts',(-48.7105476579708,-13.0557925005452,
175.429441731563));
#13421=CARTESIAN_POINT('Ctrl Pts',(-49.1406103931943,-13.0235604552581,
174.438788862592));
#13422=CARTESIAN_POINT('Ctrl Pts',(-50.6761207099769,-13.0860799668151,
173.321489243126));
#13423=CARTESIAN_POINT('Ctrl Pts',(-51.7550963134731,-13.1754760058423,
173.222308149713));
#13424=CARTESIAN_POINT('Ctrl Pts',(-53.4658619993328,-13.2728668841322,
174.044907498799));
#13425=CARTESIAN_POINT('Ctrl Pts',(-54.0695830139971,-13.2704822339251,
174.951304580462));
#13426=CARTESIAN_POINT('Ctrl Pts',(-54.1756431350045,-13.0566118191168,
176.841599266944));
#13427=CARTESIAN_POINT('Ctrl Pts',(-53.682402379201,-12.8459201272062,177.784941606983));
#13428=CARTESIAN_POINT('Ctrl Pts',(-52.1086906323698,-12.3039548020853,
178.724742549594));
#13429=CARTESIAN_POINT('Ctrl Pts',(-51.0761365726385,-11.9897880340734,
178.697123202695));
#13430=CARTESIAN_POINT('Ctrl Pts',(-49.5543778605173,-11.4626036611189,
177.68675201361));
#13431=CARTESIAN_POINT('Ctrl Pts',(-49.102117382649,-11.2567014833508,176.719561205716));
#13432=CARTESIAN_POINT('Ctrl Pts',(-49.292107286816,-11.0609269687249,174.839303437302));
#13433=CARTESIAN_POINT('Ctrl Pts',(-49.9319808722111,-11.065488255827,173.957841233623));
#13434=CARTESIAN_POINT('Ctrl Pts',(-51.6826661337304,-11.1687038756892,
173.21175444078));
#13435=CARTESIAN_POINT('Ctrl Pts',(-52.7531972098707,-11.2596980870477,
173.357216390535));
#13436=CARTESIAN_POINT('Ctrl Pts',(-54.2460458385202,-11.3089418781751,
174.551734842451));
#13437=CARTESIAN_POINT('Ctrl Pts',(-54.6245671161656,-11.2668768405657,
175.56211463078));
#13438=CARTESIAN_POINT('Ctrl Pts',(-54.3123472668563,-10.9730441873765,
177.413426209709));
#13439=CARTESIAN_POINT('Ctrl Pts',(-53.6216949876352,-10.7211032153202,
178.215314744748));
#13440=CARTESIAN_POINT('Ctrl Pts',(-51.8913746121094,-10.1550133368813,
178.758899998487));
#13441=CARTESIAN_POINT('Ctrl Pts',(-50.8831280746124,-9.84182247697009,
178.493145848044));
#13442=CARTESIAN_POINT('Ctrl Pts',(-49.6236112332636,-9.36447275925141,
177.143870489208));
#13443=CARTESIAN_POINT('Ctrl Pts',(-49.3975849797945,-9.20540142615231,
176.095279478262));
#13444=CARTESIAN_POINT('Ctrl Pts',(-50.0079456983536,-9.08466255147406,
174.288405253537));
#13445=CARTESIAN_POINT('Ctrl Pts',(-50.8244602905949,-9.12692713822202,
173.581609594638));
#13446=CARTESIAN_POINT('Ctrl Pts',(-52.6906598209441,-9.25318698046637,
173.246687842459));
#13447=CARTESIAN_POINT('Ctrl Pts',(-53.7047460872083,-9.33006604421617,
173.631253257821));
#13448=CARTESIAN_POINT('Ctrl Pts',(-54.8900559939021,-9.32613298909108,
175.117109460381));
#13449=CARTESIAN_POINT('Ctrl Pts',(-55.0428852800419,-9.23680213120813,
176.191613835385));
#13450=CARTESIAN_POINT('Ctrl Pts',(-54.3260630027991,-8.86426623816917,
177.917066297754));
#13451=CARTESIAN_POINT('Ctrl Pts',(-53.4783261791472,-8.5852751826903,178.533414961083));
#13452=CARTESIAN_POINT('Ctrl Pts',(-51.6632029807945,-7.99669600625119,
178.652882987613));
#13453=CARTESIAN_POINT('Ctrl Pts',(-50.7499980781025,-7.70554604519678,
178.155739114359));
#13454=CARTESIAN_POINT('Ctrl Pts',(-49.8242259537338,-7.29327695933862,
176.547077701437));
#13455=CARTESIAN_POINT('Ctrl Pts',(-49.838033268214,-7.17726487827271,175.466032067978));
#13456=CARTESIAN_POINT('Ctrl Pts',(-50.8256764893838,-7.13523953214819,
173.842841571287));
#13457=CARTESIAN_POINT('Ctrl Pts',(-51.7828991970818,-7.20106754009712,
173.328393136411));
#13458=CARTESIAN_POINT('Ctrl Pts',(-53.682121466631,-7.33289296119618,173.423267613666));
#13459=CARTESIAN_POINT('Ctrl Pts',(-54.5824458512144,-7.39109185214275,
174.023927494841));
#13460=CARTESIAN_POINT('Ctrl Pts',(-55.4117106483233,-7.31244449093335,
175.744908515432));
#13461=CARTESIAN_POINT('Ctrl Pts',(-55.3174225063257,-7.17911919393448,
176.81298142285));
#13462=CARTESIAN_POINT('Ctrl Pts',(-54.241836216539,-6.73809069114013,178.316074643566));
#13463=CARTESIAN_POINT('Ctrl Pts',(-53.2777666803375,-6.43346338348791,
178.716995563853));
#13464=CARTESIAN_POINT('Ctrl Pts',(-51.492709987459,-5.85671796076922,178.410389321177));
#13465=CARTESIAN_POINT('Ctrl Pts',(-50.7047045568934,-5.58599179870949,
177.709705935534));
#13466=CARTESIAN_POINT('Ctrl Pts',(-50.1611589540997,-5.24690475917716,
175.91572047402));
#13467=CARTESIAN_POINT('Ctrl Pts',(-50.412988668319,-5.17989675417243,174.862537959116));
#13468=CARTESIAN_POINT('Ctrl Pts',(-51.7459369624996,-5.19848686371817,
173.493142781303));
#13469=CARTESIAN_POINT('Ctrl Pts',(-52.7859565461007,-5.28395186106844,
173.214419006065));
#13470=CARTESIAN_POINT('Ctrl Pts',(-54.6124153348595,-5.40237052054082,
173.730440016312));
#13471=CARTESIAN_POINT('Ctrl Pts',(-55.3590089692939,-5.42765093815174,
174.520747942326));
#13472=CARTESIAN_POINT('Ctrl Pts',(-55.7857743262001,-5.27753030569205,
176.366096056906));
#13473=CARTESIAN_POINT('Ctrl Pts',(-55.461398252989,-5.09617167994865,177.38970404608));
#13474=CARTESIAN_POINT('Ctrl Pts',(-54.0763289367501,-4.5947076574371,178.59887213214));
#13475=CARTESIAN_POINT('Ctrl Pts',(-53.0518069694618,-4.2817330879142,178.762764238352));
#13476=CARTESIAN_POINT('Ctrl Pts',(-51.3741810061549,-3.71961935803744,
178.037173193724));
#13477=CARTESIAN_POINT('Ctrl Pts',(-50.7709128345885,-3.48817293681553,
177.171361011829));
#13478=CARTESIAN_POINT('Ctrl Pts',(-50.6389382081356,-3.22905679794207,
175.293151941354));
#13479=CARTESIAN_POINT('Ctrl Pts',(-51.12053621277,-3.20321300476925,174.318272388974));
#13480=CARTESIAN_POINT('Ctrl Pts',(-52.7133196362096,-3.27785561089881,
173.283689189228));
#13481=CARTESIAN_POINT('Ctrl Pts',(-53.7973395798457,-3.36818712000785,
173.24106430149));
#13482=CARTESIAN_POINT('Ctrl Pts',(-55.4653436163453,-3.45546685002776,
174.15674387015));
#13483=CARTESIAN_POINT('Ctrl Pts',(-56.0173052873986,-3.44570666511222,
175.091057375796));
#13484=CARTESIAN_POINT('Ctrl Pts',(-56.0215539606611,-3.28449111210032,
176.384962205932));
#13485=CARTESIAN_POINT('Ctrl Pts',(-55.9545655524391,-3.23079314429921,
176.725242297786));
#13486=CARTESIAN_POINT('Ctrl Pts',(-55.7610730366685,-3.12770940060629,
177.200137919422));
#13487=CARTESIAN_POINT('Ctrl Pts',(-55.6813772878146,-3.09105284269064,
177.349953976371));
#13488=CARTESIAN_POINT('Ctrl Pts',(-55.542047034587,-3.0325075684579,177.559861392858));
#13489=CARTESIAN_POINT('Ctrl Pts',(-55.4922962422521,-3.01237854056411,
177.627368088468));
#13490=CARTESIAN_POINT('Ctrl Pts',(-55.3864710916189,-2.97076694703694,
177.757099244203));
#13491=CARTESIAN_POINT('Ctrl Pts',(-55.3343400650611,-2.9517036220202,177.814670571915));
#13492=CARTESIAN_POINT('Ctrl Pts',(-55.2712257966423,-2.92704897744562,
177.878689530232));
#13493=CARTESIAN_POINT('Ctrl Pts',(-50.193114320713,-27.8005016688432,177.448440461337));
#13494=CARTESIAN_POINT('Ctrl Pts',(-50.1356777281885,-27.7780416249781,
177.514251363723));
#13495=CARTESIAN_POINT('Ctrl Pts',(-50.0768656935625,-27.751543311514,177.569181845458));
#13496=CARTESIAN_POINT('Ctrl Pts',(-49.9502510673185,-27.7006718917524,
177.678131488152));
#13497=CARTESIAN_POINT('Ctrl Pts',(-49.8836384545372,-27.6746069642733,
177.728584647058));
#13498=CARTESIAN_POINT('Ctrl Pts',(-49.6751767137455,-27.5945945456976,
177.866776279515));
#13499=CARTESIAN_POINT('Ctrl Pts',(-49.5241175159801,-27.5384622401806,
177.941191651987));
#13500=CARTESIAN_POINT('Ctrl Pts',(-49.052722448706,-27.3677108924734,178.102046365205));
#13501=CARTESIAN_POINT('Ctrl Pts',(-48.713006227557,-27.2491092781452,178.126053652285));
#13502=CARTESIAN_POINT('Ctrl Pts',(-47.7382795874562,-26.9019657740439,
177.942209528285));
#13503=CARTESIAN_POINT('Ctrl Pts',(-47.1597470877608,-26.6842880122364,
177.461567693823));
#13504=CARTESIAN_POINT('Ctrl Pts',(-46.658904710499,-26.3725604903201,176.179580952166));
#13505=CARTESIAN_POINT('Ctrl Pts',(-46.744016732095,-26.2835354545934,175.410971277798));
#13506=CARTESIAN_POINT('Ctrl Pts',(-47.5354179070377,-26.2224078706935,
174.242909311213));
#13507=CARTESIAN_POINT('Ctrl Pts',(-48.2245449656354,-26.2493771368743,
173.87343933243));
#13508=CARTESIAN_POINT('Ctrl Pts',(-49.6317089464608,-26.3060463238627,
173.871895146128));
#13509=CARTESIAN_POINT('Ctrl Pts',(-50.3230600395606,-26.332977077053,174.238655026377));
#13510=CARTESIAN_POINT('Ctrl Pts',(-51.1153496063116,-26.2743348509258,
175.387691644257));
#13511=CARTESIAN_POINT('Ctrl Pts',(-51.2096393582444,-26.1855070701005,
176.164686974611));
#13512=CARTESIAN_POINT('Ctrl Pts',(-50.7213268039385,-25.8775623946772,
177.442968877094));
#13513=CARTESIAN_POINT('Ctrl Pts',(-50.1473617008829,-25.6602454668112,
177.932812658479));
#13514=CARTESIAN_POINT('Ctrl Pts',(-48.8451246534299,-25.1962898596545,
178.190564242377));
#13515=CARTESIAN_POINT('Ctrl Pts',(-48.1356293396501,-24.9529458243571,
177.955714348281));
#13516=CARTESIAN_POINT('Ctrl Pts',(-47.2268076672755,-24.5631416907191,
176.954286183848));
#13517=CARTESIAN_POINT('Ctrl Pts',(-47.0395646158613,-24.4209960169422,
176.20954077848));
#13518=CARTESIAN_POINT('Ctrl Pts',(-47.370313215787,-24.2726666068476,174.855768290097));
#13519=CARTESIAN_POINT('Ctrl Pts',(-47.8845545017147,-24.265674947158,174.26583855031));
#13520=CARTESIAN_POINT('Ctrl Pts',(-49.1994460468846,-24.3046603227726,
173.764180115318));
#13521=CARTESIAN_POINT('Ctrl Pts',(-49.9762257647407,-24.3480555327739,
173.861039734223));
#13522=CARTESIAN_POINT('Ctrl Pts',(-51.1285193941288,-24.3574791486806,
174.66646218052));
#13523=CARTESIAN_POINT('Ctrl Pts',(-51.4882290443068,-24.3203491702665,
175.364132112564));
#13524=CARTESIAN_POINT('Ctrl Pts',(-51.4777341832408,-24.1036300286494,
176.755680066459));
#13525=CARTESIAN_POINT('Ctrl Pts',(-51.1141102527119,-23.9275319100486,
177.423612084264));
#13526=CARTESIAN_POINT('Ctrl Pts',(-49.9940329966114,-23.4994535030053,
178.148719290634));
#13527=CARTESIAN_POINT('Ctrl Pts',(-49.2531996565364,-23.2503850964097,
178.195074921104));
#13528=CARTESIAN_POINT('Ctrl Pts',(-48.0540724826088,-22.804580182732,177.607487959387));
#13529=CARTESIAN_POINT('Ctrl Pts',(-47.6174629086983,-22.6140260251447,
176.985139741962));
#13530=CARTESIAN_POINT('Ctrl Pts',(-47.4549919432363,-22.3698803060775,
175.609945370482));
#13531=CARTESIAN_POINT('Ctrl Pts',(-47.7329522193418,-22.3169255939418,
174.876470615888));
#13532=CARTESIAN_POINT('Ctrl Pts',(-48.8440385240951,-22.3059754149369,
173.902867041218));
#13533=CARTESIAN_POINT('Ctrl Pts',(-49.7035599970344,-22.3554674780819,
173.739637329099));
#13534=CARTESIAN_POINT('Ctrl Pts',(-51.1531706356154,-22.4011313967338,
174.265066374312));
#13535=CARTESIAN_POINT('Ctrl Pts',(-51.7115054154064,-22.3910761212842,
174.945624054023));
#13536=CARTESIAN_POINT('Ctrl Pts',(-51.9563259347572,-22.2045289991918,
176.459132103654));
#13537=CARTESIAN_POINT('Ctrl Pts',(-51.63765119649,-22.0251559400258,177.262331468575));
#13538=CARTESIAN_POINT('Ctrl Pts',(-50.4571461815608,-21.5627984935069,
178.149907937338));
#13539=CARTESIAN_POINT('Ctrl Pts',(-49.6222512854117,-21.2849471395443,
178.217719280236));
#13540=CARTESIAN_POINT('Ctrl Pts',(-48.3256452005116,-20.7988977065915,
177.525255091295));
#13541=CARTESIAN_POINT('Ctrl Pts',(-47.8935170509031,-20.5993012814682,
176.78942555283));
#13542=CARTESIAN_POINT('Ctrl Pts',(-47.9069259765589,-20.3679964193449,
175.264267840625));
#13543=CARTESIAN_POINT('Ctrl Pts',(-48.3565963500671,-20.33698501403,174.508050023486));
#13544=CARTESIAN_POINT('Ctrl Pts',(-49.7115395236169,-20.3645147337819,
173.767258025586));
#13545=CARTESIAN_POINT('Ctrl Pts',(-50.5919963646361,-20.4163759449694,
173.798730113887));
#13546=CARTESIAN_POINT('Ctrl Pts',(-51.8921615926268,-20.4324111199544,
174.637786957993));
#13547=CARTESIAN_POINT('Ctrl Pts',(-52.2870845316673,-20.391715494119,175.425932171935));
#13548=CARTESIAN_POINT('Ctrl Pts',(-52.1845249551972,-20.1359343420921,
176.949348485014));
#13549=CARTESIAN_POINT('Ctrl Pts',(-51.6978717551623,-19.9258306519252,
177.647217385389));
#13550=CARTESIAN_POINT('Ctrl Pts',(-50.3567743114224,-19.4332812849397,
178.229888643815));
#13551=CARTESIAN_POINT('Ctrl Pts',(-49.531482093434,-19.1564117811874,178.098575810452));
#13552=CARTESIAN_POINT('Ctrl Pts',(-48.4209526978951,-18.7085233315365,
177.123331466978));
#13553=CARTESIAN_POINT('Ctrl Pts',(-48.1597795720535,-18.5402167412103,
176.29718764283));
#13554=CARTESIAN_POINT('Ctrl Pts',(-48.5145782694716,-18.3739619700934,
174.800216258582));
#13555=CARTESIAN_POINT('Ctrl Pts',(-49.1216168980297,-18.3741927637648,
174.159897255644));
#13556=CARTESIAN_POINT('Ctrl Pts',(-50.6124880467131,-18.4256628314289,
173.74530968569));
#13557=CARTESIAN_POINT('Ctrl Pts',(-51.4570089590119,-18.472296203581,173.973986288395));
#13558=CARTESIAN_POINT('Ctrl Pts',(-52.5367755134872,-18.4465314340497,
175.076321400051));
#13559=CARTESIAN_POINT('Ctrl Pts',(-52.7461464663159,-18.3691716102472,
175.928004990245));
#13560=CARTESIAN_POINT('Ctrl Pts',(-52.3166330239091,-18.0526500335514,
177.376965544067));
#13561=CARTESIAN_POINT('Ctrl Pts',(-51.6857211698905,-17.8130496454,177.945754508989));
#13562=CARTESIAN_POINT('Ctrl Pts',(-50.2465394893753,-17.3007990625156,
178.194297846636));
#13563=CARTESIAN_POINT('Ctrl Pts',(-49.4703000985441,-17.0343670318334,
177.871754882023));
#13564=CARTESIAN_POINT('Ctrl Pts',(-48.6088763818932,-16.6321365971318,
176.648991214725));
#13565=CARTESIAN_POINT('Ctrl Pts',(-48.5409020769561,-16.5028432711256,
175.78526591443));
#13566=CARTESIAN_POINT('Ctrl Pts',(-49.2164515058916,-16.3991203888251,
174.401518908745));
#13567=CARTESIAN_POINT('Ctrl Pts',(-49.9496118192587,-16.4227354715302,
173.914202886417));
#13568=CARTESIAN_POINT('Ctrl Pts',(-51.4902606534728,-16.4861638259448,
173.836744887307));
#13569=CARTESIAN_POINT('Ctrl Pts',(-52.2697075969923,-16.5185243960147,
174.249627738192));
#13570=CARTESIAN_POINT('Ctrl Pts',(-53.0792623986938,-16.4399376212412,
175.566241461313));
#13571=CARTESIAN_POINT('Ctrl Pts',(-53.0958608617722,-16.3264383488088,
176.440260240546));
#13572=CARTESIAN_POINT('Ctrl Pts',(-52.3498924896565,-15.9464100326616,
177.743856795072));
#13573=CARTESIAN_POINT('Ctrl Pts',(-51.6136771994172,-15.6882407493956,
178.142477224647));
#13574=CARTESIAN_POINT('Ctrl Pts',(-50.1619939854693,-15.1743526813971,
178.045393567771));
#13575=CARTESIAN_POINT('Ctrl Pts',(-49.479535393056,-14.9249532161513,177.547481856475));
#13576=CARTESIAN_POINT('Ctrl Pts',(-48.9083003859244,-14.5811172796918,
176.154888290848));
#13577=CARTESIAN_POINT('Ctrl Pts',(-49.032687325759,-14.4872017268269,175.286386043965));
#13578=CARTESIAN_POINT('Ctrl Pts',(-50.002899927607,-14.4395306566209,174.08106638639));
#13579=CARTESIAN_POINT('Ctrl Pts',(-50.8258619899905,-14.4815667576624,
173.768688449528));
#13580=CARTESIAN_POINT('Ctrl Pts',(-52.3490472247602,-14.5391579602322,
174.044477097964));
#13581=CARTESIAN_POINT('Ctrl Pts',(-53.0108480437211,-14.5505369630929,
174.618897762295));
#13582=CARTESIAN_POINT('Ctrl Pts',(-53.508606726061,-14.41258118913,176.072854784516));
#13583=CARTESIAN_POINT('Ctrl Pts',(-53.3308496256547,-14.2605010523332,
176.92211652172));
#13584=CARTESIAN_POINT('Ctrl Pts',(-52.3234046589676,-13.8325238003689,
178.011250192421));
#13585=CARTESIAN_POINT('Ctrl Pts',(-51.5138129382755,-13.5585438056648,
178.229366209696));
#13586=CARTESIAN_POINT('Ctrl Pts',(-50.1182607249297,-13.0546721198729,
177.788098654291));
#13587=CARTESIAN_POINT('Ctrl Pts',(-49.5630188185408,-12.8308644828691,
177.140857971114));
#13588=CARTESIAN_POINT('Ctrl Pts',(-49.3219040202974,-12.5483689245281,
175.637957478437));
#13589=CARTESIAN_POINT('Ctrl Pts',(-49.6365594730894,-12.4926951709364,
174.821179942866));
#13590=CARTESIAN_POINT('Ctrl Pts',(-50.8450351424658,-12.4918253386163,
173.862170041067));
#13591=CARTESIAN_POINT('Ctrl Pts',(-51.7160671936879,-12.5420406725331,
173.742988789581));
#13592=CARTESIAN_POINT('Ctrl Pts',(-53.1380531234061,-12.5824907099911,
174.344563971126));
#13593=CARTESIAN_POINT('Ctrl Pts',(-53.661497991413,-12.565516429584,175.054752397452));
#13594=CARTESIAN_POINT('Ctrl Pts',(-53.8242077932451,-12.3622912981454,
176.579637740953));
#13595=CARTESIAN_POINT('Ctrl Pts',(-53.4635573374974,-12.1759538811977,
177.362604506387));
#13596=CARTESIAN_POINT('Ctrl Pts',(-52.2358756182636,-11.7031645393402,
178.179207046235));
#13597=CARTESIAN_POINT('Ctrl Pts',(-51.404471480006,-11.4266005921062,178.198059647233));
#13598=CARTESIAN_POINT('Ctrl Pts',(-50.1465877134854,-10.9499764840513,
177.440684540534));
#13599=CARTESIAN_POINT('Ctrl Pts',(-49.7512566691313,-10.7559713173261,
176.677961727673));
#13600=CARTESIAN_POINT('Ctrl Pts',(-49.8442980389787,-10.5402489724976,
175.152069846099));
#13601=CARTESIAN_POINT('Ctrl Pts',(-50.3336227209985,-10.5166703329192,
174.417963751365));
#13602=CARTESIAN_POINT('Ctrl Pts',(-51.729412313951,-10.5511670115394,173.750914008412));
#13603=CARTESIAN_POINT('Ctrl Pts',(-52.6055357660183,-10.6034581645062,
173.829125569603));
#13604=CARTESIAN_POINT('Ctrl Pts',(-53.8591972775733,-10.6090268187652,
174.739479897504));
#13605=CARTESIAN_POINT('Ctrl Pts',(-54.2075655427863,-10.559958422732,175.542285446703));
#13606=CARTESIAN_POINT('Ctrl Pts',(-54.0309723767407,-10.2919570312328,
177.05153449857));
#13607=CARTESIAN_POINT('Ctrl Pts',(-53.5065211660476,-10.0729835636969,
177.724885949439));
#13608=CARTESIAN_POINT('Ctrl Pts',(-52.1359327706082,-9.57501150980407,
178.231990439602));
#13609=CARTESIAN_POINT('Ctrl Pts',(-51.3168725161042,-9.29919601638729,
178.055337178134));
#13610=CARTESIAN_POINT('Ctrl Pts',(-50.258716477129,-8.86039345968628,177.014257444883));
#13611=CARTESIAN_POINT('Ctrl Pts',(-50.0419858596938,-8.70190296068798,
176.174822144773));
#13612=CARTESIAN_POINT('Ctrl Pts',(-50.4788136762356,-8.55014763089762,
174.697436550109));
#13613=CARTESIAN_POINT('Ctrl Pts',(-51.1165600370436,-8.55674976323144,
174.095019459488));
#13614=CARTESIAN_POINT('Ctrl Pts',(-52.6206590619166,-8.6128620697194,173.755704628284));
#13615=CARTESIAN_POINT('Ctrl Pts',(-53.456626592603,-8.65630954771657,174.029197443714));
#13616=CARTESIAN_POINT('Ctrl Pts',(-54.4781193003427,-8.6195332279715,175.187078119489));
#13617=CARTESIAN_POINT('Ctrl Pts',(-54.643602443466,-8.53353572012608,176.04949882023));
#13618=CARTESIAN_POINT('Ctrl Pts',(-54.1354947853707,-8.20096498746117,
177.472181687833));
#13619=CARTESIAN_POINT('Ctrl Pts',(-53.4760203027823,-7.95706608118669,
178.003825172765));
#13620=CARTESIAN_POINT('Ctrl Pts',(-52.0249165538012,-7.441132564782,178.167825277993));
#13621=CARTESIAN_POINT('Ctrl Pts',(-51.2723007652614,-7.17976116760829,
177.802466009854));
#13622=CARTESIAN_POINT('Ctrl Pts',(-50.4742318046734,-6.79179686888332,
176.539214575509));
#13623=CARTESIAN_POINT('Ctrl Pts',(-50.4508393849021,-6.66952799804251,
175.667365550039));
#13624=CARTESIAN_POINT('Ctrl Pts',(-51.1982775200671,-6.57992894303025,
174.318931761547));
#13625=CARTESIAN_POINT('Ctrl Pts',(-51.9567203354133,-6.60831910752051,
173.869388776842));
#13626=CARTESIAN_POINT('Ctrl Pts',(-53.5030461170827,-6.67180659392302,
173.876188814802));
#13627=CARTESIAN_POINT('Ctrl Pts',(-54.2579318048227,-6.70074853854407,
174.329266762268));
#13628=CARTESIAN_POINT('Ctrl Pts',(-54.9950541895712,-6.6067812144727,175.688231083653));
#13629=CARTESIAN_POINT('Ctrl Pts',(-54.9633937640365,-6.48434226598442,
176.556150922255));
#13630=CARTESIAN_POINT('Ctrl Pts',(-54.1573516980127,-6.0949735677162,177.812809342709));
#13631=CARTESIAN_POINT('Ctrl Pts',(-53.3979887985791,-5.83073710308303,
178.172806822259));
#13632=CARTESIAN_POINT('Ctrl Pts',(-51.9519097716579,-5.31810666795101,
177.994568269632));
#13633=CARTESIAN_POINT('Ctrl Pts',(-51.2952074816856,-5.0735953089356,177.458800517348));
#13634=CARTESIAN_POINT('Ctrl Pts',(-50.7993635736617,-4.74342220821161,
176.031468409862));
#13635=CARTESIAN_POINT('Ctrl Pts',(-50.9692613848378,-4.65940397939939,
175.170313217647));
#13636=CARTESIAN_POINT('Ctrl Pts',(-52.0040245669764,-4.62293999106357,
174.01934301833));
#13637=CARTESIAN_POINT('Ctrl Pts',(-52.8385688131003,-4.66759138415716,
173.754231358386));
#13638=CARTESIAN_POINT('Ctrl Pts',(-54.3414847379305,-4.72329909029368,
174.103969484305));
#13639=CARTESIAN_POINT('Ctrl Pts',(-54.9761466933045,-4.72791014175074,
174.714716972292));
#13640=CARTESIAN_POINT('Ctrl Pts',(-55.3975165431988,-4.57549651155636,
176.192173272167));
#13641=CARTESIAN_POINT('Ctrl Pts',(-55.1760506072609,-4.4148786220368,177.03103539143));
#13642=CARTESIAN_POINT('Ctrl Pts',(-54.1093043232961,-3.97451188101218,
178.061753391873));
#13643=CARTESIAN_POINT('Ctrl Pts',(-53.2902925544343,-3.69995792969149,
178.233822626392));
#13644=CARTESIAN_POINT('Ctrl Pts',(-51.9203920380846,-3.19963469730891,
177.711493690972));
#13645=CARTESIAN_POINT('Ctrl Pts',(-51.4044324721558,-2.98383265912278,
177.036002564632));
#13646=CARTESIAN_POINT('Ctrl Pts',(-51.237949425703,-2.71774512370317,175.525044339462));
#13647=CARTESIAN_POINT('Ctrl Pts',(-51.5957499271559,-2.66894330374766,
174.721509320474));
#13648=CARTESIAN_POINT('Ctrl Pts',(-52.8541051305037,-2.67783999801612,
173.825937213487));
#13649=CARTESIAN_POINT('Ctrl Pts',(-53.7315999697276,-2.7292086653859,173.7525048498));
#13650=CARTESIAN_POINT('Ctrl Pts',(-55.1208667949195,-2.76252327401043,
174.431246184642));
#13651=CARTESIAN_POINT('Ctrl Pts',(-55.6054709668258,-2.73893798071373,
175.167402226862));
#13652=CARTESIAN_POINT('Ctrl Pts',(-55.6603171863937,-2.58869274068622,
176.211840888345));
#13653=CARTESIAN_POINT('Ctrl Pts',(-55.6210463302226,-2.5392081864434,176.490448482462));
#13654=CARTESIAN_POINT('Ctrl Pts',(-55.4836397365907,-2.4479441182576,176.880586390838));
#13655=CARTESIAN_POINT('Ctrl Pts',(-55.4253285390117,-2.41535251334816,
177.005027857449));
#13656=CARTESIAN_POINT('Ctrl Pts',(-55.321414213033,-2.36345060131236,177.180440236558));
#13657=CARTESIAN_POINT('Ctrl Pts',(-55.2840225057543,-2.34563722905757,
177.23703696138));
#13658=CARTESIAN_POINT('Ctrl Pts',(-55.2039936793606,-2.30896761153951,
177.345998347345));
#13659=CARTESIAN_POINT('Ctrl Pts',(-55.1587206712145,-2.28906361698866,
177.401367187303));
#13660=CARTESIAN_POINT('Ctrl Pts',(-55.1161897096451,-2.27071607222657,
177.448351373365));
#13661=CARTESIAN_POINT('',(-49.6057233026533,-28.1882175989763,177.068114089093));
#13662=CARTESIAN_POINT('',(-50.193114320713,-27.8005016688432,177.448440461337));
#13663=CARTESIAN_POINT('Origin',(-49.8994188116831,-27.9943596339097,177.258277275215));
#13664=CARTESIAN_POINT('Ctrl Pts',(-49.6057233026533,-28.1882175989763,
177.068114089093));
#13665=CARTESIAN_POINT('Ctrl Pts',(-49.5663192275732,-28.1656109096198,
177.105925367078));
#13666=CARTESIAN_POINT('Ctrl Pts',(-49.5216854287654,-28.1457023853521,
177.148383027181));
#13667=CARTESIAN_POINT('Ctrl Pts',(-49.4301127133764,-28.1014695235449,
177.220446553382));
#13668=CARTESIAN_POINT('Ctrl Pts',(-49.3819809603125,-28.0788363277035,
177.253617740645));
#13669=CARTESIAN_POINT('Ctrl Pts',(-49.2321484222821,-28.0099337266433,
177.343479018307));
#13670=CARTESIAN_POINT('Ctrl Pts',(-49.1254026293825,-27.9629901656525,
177.390284377819));
#13671=CARTESIAN_POINT('Ctrl Pts',(-48.7929164986652,-27.8189908160803,
177.48590296908));
#13672=CARTESIAN_POINT('Ctrl Pts',(-48.55635218661,-27.7202377019268,177.490394220553));
#13673=CARTESIAN_POINT('Ctrl Pts',(-47.8840648999533,-27.4305281812212,
177.324447440169));
#13674=CARTESIAN_POINT('Ctrl Pts',(-47.5006474873523,-27.2497443022818,
176.963331771584));
#13675=CARTESIAN_POINT('Ctrl Pts',(-47.2040861213115,-26.9802047380462,
176.046394548579));
#13676=CARTESIAN_POINT('Ctrl Pts',(-47.2954018922066,-26.8917044501032,
175.506598760119));
#13677=CARTESIAN_POINT('Ctrl Pts',(-47.9062028356891,-26.7943163650827,
174.710326627486));
#13678=CARTESIAN_POINT('Ctrl Pts',(-48.4108882632775,-26.7850298620733,
174.47568647468));
#13679=CARTESIAN_POINT('Ctrl Pts',(-49.4081207961382,-26.7654318876047,
174.522051214009));
#13680=CARTESIAN_POINT('Ctrl Pts',(-49.8895805322777,-26.7512165827191,
174.803706734764));
#13681=CARTESIAN_POINT('Ctrl Pts',(-50.419859907048,-26.6406327974915,175.641132157405));
#13682=CARTESIAN_POINT('Ctrl Pts',(-50.4638072135826,-26.5414518590087,
176.190943138814));
#13683=CARTESIAN_POINT('Ctrl Pts',(-50.0902675056585,-26.258306693899,177.06820282525));
#13684=CARTESIAN_POINT('Ctrl Pts',(-49.6753169680471,-26.0710530131776,
177.393289133135));
#13685=CARTESIAN_POINT('Ctrl Pts',(-48.760110273011,-25.6803067135432,177.526354227003));
#13686=CARTESIAN_POINT('Ctrl Pts',(-48.2752065557733,-25.4795815288234,
177.333261554155));
#13687=CARTESIAN_POINT('Ctrl Pts',(-47.6834949732814,-25.1537104488559,
176.598820399841));
#13688=CARTESIAN_POINT('Ctrl Pts',(-47.581935800625,-25.0274199406948,176.066471856633));
#13689=CARTESIAN_POINT('Ctrl Pts',(-47.8743577335121,-24.8702793490883,
175.122570330099));
#13690=CARTESIAN_POINT('Ctrl Pts',(-48.2639300332364,-24.8386062285325,
174.72605490093));
#13691=CARTESIAN_POINT('Ctrl Pts',(-49.2134664973944,-24.8097944361078,
174.418869413643));
#13692=CARTESIAN_POINT('Ctrl Pts',(-49.7639560285487,-24.8089577046691,
174.513086690221));
#13693=CARTESIAN_POINT('Ctrl Pts',(-50.5601436025432,-24.7482854574026,
175.121296078095));
#13694=CARTESIAN_POINT('Ctrl Pts',(-50.7937850628585,-24.6861522884041,
175.625415363842));
#13695=CARTESIAN_POINT('Ctrl Pts',(-50.7513118113109,-24.4660502953853,
176.598470930813));
#13696=CARTESIAN_POINT('Ctrl Pts',(-50.4787452748198,-24.3068424850894,
177.056448064075));
#13697=CARTESIAN_POINT('Ctrl Pts',(-49.6755858463959,-23.9384579984121,
177.525629368769));
#13698=CARTESIAN_POINT('Ctrl Pts',(-49.1583261106009,-23.7318611386462,
177.529378707235));
#13699=CARTESIAN_POINT('Ctrl Pts',(-48.3492917504345,-23.3639427741862,
177.074636497803));
#13700=CARTESIAN_POINT('Ctrl Pts',(-48.0678997211374,-23.2027238239874,
176.620161976926));
#13701=CARTESIAN_POINT('Ctrl Pts',(-48.0133698591323,-22.9779683240005,
175.643265853549));
#13702=CARTESIAN_POINT('Ctrl Pts',(-48.2419634078688,-22.9148026311583,
175.13669620061));
#13703=CARTESIAN_POINT('Ctrl Pts',(-49.0648716087653,-22.8512007031896,
174.491772947554));
#13704=CARTESIAN_POINT('Ctrl Pts',(-49.6839608902416,-22.8528771386521,
174.405900021421));
#13705=CARTESIAN_POINT('Ctrl Pts',(-50.6991943315865,-22.8143164724711,
174.826217042058));
#13706=CARTESIAN_POINT('Ctrl Pts',(-51.0745700439279,-22.7701586995258,
175.322569579276));
#13707=CARTESIAN_POINT('Ctrl Pts',(-51.2073695092728,-22.5604456438022,
176.396956445951));
#13708=CARTESIAN_POINT('Ctrl Pts',(-50.9625278765238,-22.3963905325425,
176.94851178212));
#13709=CARTESIAN_POINT('Ctrl Pts',(-50.1139689940341,-21.9977514714476,
177.529315681618));
#13710=CARTESIAN_POINT('Ctrl Pts',(-49.5293219694751,-21.7666067892758,
177.544699935169));
#13711=CARTESIAN_POINT('Ctrl Pts',(-48.6567664449969,-21.3653910132907,
177.013098304479));
#13712=CARTESIAN_POINT('Ctrl Pts',(-48.383128531039,-21.1949054338945,176.477577858981));
#13713=CARTESIAN_POINT('Ctrl Pts',(-48.4582777380059,-20.975048733324,175.402873064259));
#13714=CARTESIAN_POINT('Ctrl Pts',(-48.8055781932514,-20.9254744005303,
174.886960050279));
#13715=CARTESIAN_POINT('Ctrl Pts',(-49.7998797569528,-20.8818943796597,
174.412232108109));
#13716=CARTESIAN_POINT('Ctrl Pts',(-50.4230224397188,-20.885216808613,174.464849386198));
#13717=CARTESIAN_POINT('Ctrl Pts',(-51.3220781362712,-20.8236066704411,
175.100442044691));
#13718=CARTESIAN_POINT('Ctrl Pts',(-51.5785314568021,-20.7546592125729,
175.670463366294));
#13719=CARTESIAN_POINT('Ctrl Pts',(-51.4682882413066,-20.5004564781585,
176.732562819156));
#13720=CARTESIAN_POINT('Ctrl Pts',(-51.1076577914431,-20.313201754554,177.207532153307));
#13721=CARTESIAN_POINT('Ctrl Pts',(-50.156411198824,-19.8953744930702,177.56803029022));
#13722=CARTESIAN_POINT('Ctrl Pts',(-49.5878400685962,-19.6691878319784,
177.446385146947));
#13723=CARTESIAN_POINT('Ctrl Pts',(-48.852079415717,-19.2920053425884,176.716949064536));
#13724=CARTESIAN_POINT('Ctrl Pts',(-48.7034574890464,-19.1464856081966,
176.127114392609));
#13725=CARTESIAN_POINT('Ctrl Pts',(-49.017896392823,-18.9721498737463,175.084671234462));
#13726=CARTESIAN_POINT('Ctrl Pts',(-49.4761175027563,-18.9421345006494,
174.655217811997));
#13727=CARTESIAN_POINT('Ctrl Pts',(-50.5469446991098,-18.915664221674,174.415005106013));
#13728=CARTESIAN_POINT('Ctrl Pts',(-51.1421889783774,-18.9127734302845,
174.605352538579));
#13729=CARTESIAN_POINT('Ctrl Pts',(-51.8771202801842,-18.8200557591642,
175.418505113175));
#13730=CARTESIAN_POINT('Ctrl Pts',(-52.0018165496213,-18.7275436462981,
176.022835099282));
#13731=CARTESIAN_POINT('Ctrl Pts',(-51.6614363875286,-18.4266465795959,
177.027259608014));
#13732=CARTESIAN_POINT('Ctrl Pts',(-51.2055166082591,-18.2218754080822,
177.403206831321));
#13733=CARTESIAN_POINT('Ctrl Pts',(-50.1969770591628,-17.7923688711786,
177.524973109627));
#13734=CARTESIAN_POINT('Ctrl Pts',(-49.6679526067506,-17.5720619524455,
177.267256975221));
#13735=CARTESIAN_POINT('Ctrl Pts',(-49.1179984398299,-17.2329564925234,
176.379271882249));
#13736=CARTESIAN_POINT('Ctrl Pts',(-49.1058293111544,-17.1129691055462,
175.766207634738));
#13737=CARTESIAN_POINT('Ctrl Pts',(-49.6421979468107,-16.981953011196,174.814805282058));
#13738=CARTESIAN_POINT('Ctrl Pts',(-50.1794692968359,-16.96896833752,174.497498655776));
#13739=CARTESIAN_POINT('Ctrl Pts',(-51.2815033366288,-16.9462509137644,
174.497183387712));
#13740=CARTESIAN_POINT('Ctrl Pts',(-51.8206810039433,-16.9333636766774,
174.813868002799));
#13741=CARTESIAN_POINT('Ctrl Pts',(-52.3579329121243,-16.8019633847227,
175.767995550527));
#13742=CARTESIAN_POINT('Ctrl Pts',(-52.3444015552563,-16.6811074119364,
176.384253300385));
#13743=CARTESIAN_POINT('Ctrl Pts',(-51.7908025496479,-16.3412377353734,
177.270036214878));
#13744=CARTESIAN_POINT('Ctrl Pts',(-51.2640575414935,-16.1220052064028,
177.524939199898));
#13745=CARTESIAN_POINT('Ctrl Pts',(-50.2584821099884,-15.6936926334193,
177.402964762685));
#13746=CARTESIAN_POINT('Ctrl Pts',(-49.8024659570259,-15.4891340123335,
177.028965203342));
#13747=CARTESIAN_POINT('Ctrl Pts',(-49.4615190985809,-15.1881425443655,
176.024838210267));
#13748=CARTESIAN_POINT('Ctrl Pts',(-49.584917871472,-15.0951235636284,175.418993178211));
#13749=CARTESIAN_POINT('Ctrl Pts',(-50.3224323861862,-15.0022736039987,
174.603877612758));
#13750=CARTESIAN_POINT('Ctrl Pts',(-50.9209588419739,-14.9994851008446,
174.413907495741));
#13751=CARTESIAN_POINT('Ctrl Pts',(-51.9913299824675,-14.9728180278691,
174.658436700836));
#13752=CARTESIAN_POINT('Ctrl Pts',(-52.4458562262816,-14.942768055369,175.086526075902));
#13753=CARTESIAN_POINT('Ctrl Pts',(-52.7589234637054,-14.768747576336,176.126312497655));
#13754=CARTESIAN_POINT('Ctrl Pts',(-52.6119738826496,-14.6237809758753,
176.715478760326));
#13755=CARTESIAN_POINT('Ctrl Pts',(-51.8767097042875,-14.2467264136774,
177.445252299972));
#13756=CARTESIAN_POINT('Ctrl Pts',(-51.3074205647036,-14.0201741438431,
177.568755188896));
#13757=CARTESIAN_POINT('Ctrl Pts',(-50.3534291722187,-13.6011459302421,
177.20657523661));
#13758=CARTESIAN_POINT('Ctrl Pts',(-49.9921349812078,-13.4131957453291,
176.728222347554));
#13759=CARTESIAN_POINT('Ctrl Pts',(-49.8860852889645,-13.159806046502,175.66552302478));
#13760=CARTESIAN_POINT('Ctrl Pts',(-50.1425376823364,-13.0914495220188,
175.099033652958));
#13761=CARTESIAN_POINT('Ctrl Pts',(-51.0393482876635,-13.0300320803285,
174.465742160163));
#13762=CARTESIAN_POINT('Ctrl Pts',(-51.661049564308,-13.0333384108268,174.411629490546));
#13763=CARTESIAN_POINT('Ctrl Pts',(-52.6556849728402,-12.9898139344045,
174.885756683857));
#13764=CARTESIAN_POINT('Ctrl Pts',(-53.0050117718212,-12.9403514819039,
175.401975295897));
#13765=CARTESIAN_POINT('Ctrl Pts',(-53.0797917942593,-12.7198628954119,
176.47950485369));
#13766=CARTESIAN_POINT('Ctrl Pts',(-52.8035180796908,-12.5482535501767,
177.017249165378));
#13767=CARTESIAN_POINT('Ctrl Pts',(-51.928756778869,-12.1465816152287,177.545168184464));
#13768=CARTESIAN_POINT('Ctrl Pts',(-51.3476399628683,-11.9168238447545,
177.52855345072));
#13769=CARTESIAN_POINT('Ctrl Pts',(-50.5013329357435,-11.5191203268418,
176.948730973903));
#13770=CARTESIAN_POINT('Ctrl Pts',(-50.2557375091139,-11.3551615877155,
176.398843509589));
#13771=CARTESIAN_POINT('Ctrl Pts',(-50.3877927376681,-11.145398461788,175.324825412843));
#13772=CARTESIAN_POINT('Ctrl Pts',(-50.762684868614,-11.1008426423184,174.826271833705));
#13773=CARTESIAN_POINT('Ctrl Pts',(-51.7811268292925,-11.0622619854364,
174.405264562934));
#13774=CARTESIAN_POINT('Ctrl Pts',(-52.4028793467296,-11.063958202758,174.492793292778));
#13775=CARTESIAN_POINT('Ctrl Pts',(-53.2632154661256,-10.9967409315864,
175.172494096186));
#13776=CARTESIAN_POINT('Ctrl Pts',(-53.4886849878534,-10.9225114509841,
175.750866168407));
#13777=CARTESIAN_POINT('Ctrl Pts',(-53.3251423960266,-10.6565821386363,
176.805379202472));
#13778=CARTESIAN_POINT('Ctrl Pts',(-52.9407422532226,-10.465785944074,177.259010843821));
#13779=CARTESIAN_POINT('Ctrl Pts',(-51.9697953271392,-10.0433159226031,
177.565260787091));
#13780=CARTESIAN_POINT('Ctrl Pts',(-51.4073968434514,-9.81808614025534,
177.411394538556));
#13781=CARTESIAN_POINT('Ctrl Pts',(-50.7116066211125,-9.44884954788431,
176.639139203566));
#13782=CARTESIAN_POINT('Ctrl Pts',(-50.5960828064805,-9.30833579234248,
176.038056438509));
#13783=CARTESIAN_POINT('Ctrl Pts',(-50.9640903737478,-9.14636922546571,
175.0167568496));
#13784=CARTESIAN_POINT('Ctrl Pts',(-51.4414488535671,-9.12058052193367,
174.612974652851));
#13785=CARTESIAN_POINT('Ctrl Pts',(-52.5249204417031,-9.09513784416194,
174.426509843431));
#13786=CARTESIAN_POINT('Ctrl Pts',(-53.1088418277628,-9.09114996369398,
174.646804488947));
#13787=CARTESIAN_POINT('Ctrl Pts',(-53.801661971168,-8.98942785386125,175.498626413927));
#13788=CARTESIAN_POINT('Ctrl Pts',(-53.8945655335682,-8.89052591977855,
176.108945227942));
#13789=CARTESIAN_POINT('Ctrl Pts',(-53.5007325042087,-8.57967938234873,
177.090495387502));
#13790=CARTESIAN_POINT('Ctrl Pts',(-53.0228734977247,-8.36926263084827,
177.439659990072));
#13791=CARTESIAN_POINT('Ctrl Pts',(-52.0134388460396,-7.941561484533,177.502665384752));
#13792=CARTESIAN_POINT('Ctrl Pts',(-51.5009539686643,-7.72503451842822,
177.217498325365));
#13793=CARTESIAN_POINT('Ctrl Pts',(-50.9958226444158,-7.39311721565184,
176.298072843289));
#13794=CARTESIAN_POINT('Ctrl Pts',(-51.0149583411939,-7.28021855779389,
175.684524900703));
#13795=CARTESIAN_POINT('Ctrl Pts',(-51.602189663565,-7.15816051285745,174.759352960774));
#13796=CARTESIAN_POINT('Ctrl Pts',(-52.1561751142271,-7.14821693453925,
174.470064567704));
#13797=CARTESIAN_POINT('Ctrl Pts',(-53.257284967077,-7.12553378294388,174.528734890764));
#13798=CARTESIAN_POINT('Ctrl Pts',(-53.7798318899166,-7.10813319884164,
174.876062446534));
#13799=CARTESIAN_POINT('Ctrl Pts',(-54.263309402104,-6.96831483361839,175.852098283111));
#13800=CARTESIAN_POINT('Ctrl Pts',(-54.2182177005742,-6.84182185515181,
176.463118413));
#13801=CARTESIAN_POINT('Ctrl Pts',(-53.620326169719,-6.49215310837908,177.317242942806));
#13802=CARTESIAN_POINT('Ctrl Pts',(-53.0815432796407,-6.27162057701451,
177.542753252723));
#13803=CARTESIAN_POINT('Ctrl Pts',(-52.0813405764902,-5.84340716815714,
177.363069610828));
#13804=CARTESIAN_POINT('Ctrl Pts',(-51.6451899827477,-5.64252013198273,
176.962963727015));
#13805=CARTESIAN_POINT('Ctrl Pts',(-51.3585173428123,-5.35236886702559,
175.939011043839));
#13806=CARTESIAN_POINT('Ctrl Pts',(-51.5164782073777,-5.2645103327986,175.337256223397));
#13807=CARTESIAN_POINT('Ctrl Pts',(-52.2924300679745,-5.18119763163266,
174.565366155634));
#13808=CARTESIAN_POINT('Ctrl Pts',(-52.8973452213176,-5.1801045826173,174.406680096152));
#13809=CARTESIAN_POINT('Ctrl Pts',(-53.956162505713,-5.14973256956073,174.705214074754));
#13810=CARTESIAN_POINT('Ctrl Pts',(-54.3874707400874,-5.11629663400306,
175.155234787811));
#13811=CARTESIAN_POINT('Ctrl Pts',(-54.6460006492434,-4.93091655090319,
176.210608238885));
#13812=CARTESIAN_POINT('Ctrl Pts',(-54.4681690759566,-4.77980797892323,
176.790635503925));
#13813=CARTESIAN_POINT('Ctrl Pts',(-53.6946945331643,-4.3956772156615,177.47627897342));
#13814=CARTESIAN_POINT('Ctrl Pts',(-53.1174419759953,-4.16620647621949,
177.565792133827));
#13815=CARTESIAN_POINT('Ctrl Pts',(-52.1878574222778,-3.75385530866336,
177.150829002666));
#13816=CARTESIAN_POINT('Ctrl Pts',(-51.8529856411974,-3.5715083216093,176.654958973924));
#13817=CARTESIAN_POINT('Ctrl Pts',(-51.8010050251376,-3.32706416715232,
175.583828138226));
#13818=CARTESIAN_POINT('Ctrl Pts',(-52.0854219579878,-3.26527816982496,
175.031488604324));
#13819=CARTESIAN_POINT('Ctrl Pts',(-53.0170398348192,-3.20959915076688,
174.444132662069));
#13820=CARTESIAN_POINT('Ctrl Pts',(-53.6416591927321,-3.21325709639781,
174.423035709656));
#13821=CARTESIAN_POINT('Ctrl Pts',(-54.6090153740635,-3.16498595686182,
174.948967905512));
#13822=CARTESIAN_POINT('Ctrl Pts',(-54.9308286711417,-3.10893139642228,
175.48555871107));
#13823=CARTESIAN_POINT('Ctrl Pts',(-54.9426665516143,-2.95192631073098,
176.218540695264));
#13824=CARTESIAN_POINT('Ctrl Pts',(-54.9070365263685,-2.90171640292054,
176.413787336324));
#13825=CARTESIAN_POINT('Ctrl Pts',(-54.8013987998623,-2.81782847468563,
176.681821034794));
#13826=CARTESIAN_POINT('Ctrl Pts',(-54.7570848510793,-2.78787367953458,
176.767627228561));
#13827=CARTESIAN_POINT('Ctrl Pts',(-54.6793253219128,-2.74078668455889,
176.887592985838));
#13828=CARTESIAN_POINT('Ctrl Pts',(-54.651529701944,-2.72473899696222,176.926133356148));
#13829=CARTESIAN_POINT('Ctrl Pts',(-54.5925997439423,-2.69209575899625,
176.999824075839));
#13830=CARTESIAN_POINT('Ctrl Pts',(-54.5641015373143,-2.67654794454284,
177.031971691023));
#13831=CARTESIAN_POINT('Ctrl Pts',(-54.5288628436534,-2.65870383148502,
177.068203177065));
#13832=CARTESIAN_POINT('Ctrl Pts',(-50.193114320713,-27.8005016688432,177.448440461337));
#13833=CARTESIAN_POINT('Ctrl Pts',(-50.1356777281885,-27.7780416249781,
177.514251363723));
#13834=CARTESIAN_POINT('Ctrl Pts',(-50.0768656935625,-27.751543311514,177.569181845458));
#13835=CARTESIAN_POINT('Ctrl Pts',(-49.9502510673185,-27.7006718917524,
177.678131488152));
#13836=CARTESIAN_POINT('Ctrl Pts',(-49.8836384545372,-27.6746069642733,
177.728584647058));
#13837=CARTESIAN_POINT('Ctrl Pts',(-49.6751767137455,-27.5945945456976,
177.866776279515));
#13838=CARTESIAN_POINT('Ctrl Pts',(-49.5241175159801,-27.5384622401806,
177.941191651987));
#13839=CARTESIAN_POINT('Ctrl Pts',(-49.052722448706,-27.3677108924734,178.102046365205));
#13840=CARTESIAN_POINT('Ctrl Pts',(-48.713006227557,-27.2491092781452,178.126053652285));
#13841=CARTESIAN_POINT('Ctrl Pts',(-47.7382795874562,-26.9019657740439,
177.942209528285));
#13842=CARTESIAN_POINT('Ctrl Pts',(-47.1597470877608,-26.6842880122364,
177.461567693823));
#13843=CARTESIAN_POINT('Ctrl Pts',(-46.658904710499,-26.3725604903201,176.179580952166));
#13844=CARTESIAN_POINT('Ctrl Pts',(-46.744016732095,-26.2835354545934,175.410971277798));
#13845=CARTESIAN_POINT('Ctrl Pts',(-47.5354179070377,-26.2224078706935,
174.242909311213));
#13846=CARTESIAN_POINT('Ctrl Pts',(-48.2245449656354,-26.2493771368743,
173.87343933243));
#13847=CARTESIAN_POINT('Ctrl Pts',(-49.6317089464608,-26.3060463238627,
173.871895146128));
#13848=CARTESIAN_POINT('Ctrl Pts',(-50.3230600395606,-26.332977077053,174.238655026377));
#13849=CARTESIAN_POINT('Ctrl Pts',(-51.1153496063116,-26.2743348509258,
175.387691644257));
#13850=CARTESIAN_POINT('Ctrl Pts',(-51.2096393582444,-26.1855070701005,
176.164686974611));
#13851=CARTESIAN_POINT('Ctrl Pts',(-50.7213268039385,-25.8775623946772,
177.442968877094));
#13852=CARTESIAN_POINT('Ctrl Pts',(-50.1473617008829,-25.6602454668112,
177.932812658479));
#13853=CARTESIAN_POINT('Ctrl Pts',(-48.8451246534299,-25.1962898596545,
178.190564242377));
#13854=CARTESIAN_POINT('Ctrl Pts',(-48.1356293396501,-24.9529458243571,
177.955714348281));
#13855=CARTESIAN_POINT('Ctrl Pts',(-47.2268076672755,-24.5631416907191,
176.954286183848));
#13856=CARTESIAN_POINT('Ctrl Pts',(-47.0395646158613,-24.4209960169422,
176.20954077848));
#13857=CARTESIAN_POINT('Ctrl Pts',(-47.370313215787,-24.2726666068476,174.855768290097));
#13858=CARTESIAN_POINT('Ctrl Pts',(-47.8845545017147,-24.265674947158,174.26583855031));
#13859=CARTESIAN_POINT('Ctrl Pts',(-49.1994460468846,-24.3046603227726,
173.764180115318));
#13860=CARTESIAN_POINT('Ctrl Pts',(-49.9762257647407,-24.3480555327739,
173.861039734223));
#13861=CARTESIAN_POINT('Ctrl Pts',(-51.1285193941288,-24.3574791486806,
174.66646218052));
#13862=CARTESIAN_POINT('Ctrl Pts',(-51.4882290443068,-24.3203491702665,
175.364132112564));
#13863=CARTESIAN_POINT('Ctrl Pts',(-51.4777341832408,-24.1036300286494,
176.755680066459));
#13864=CARTESIAN_POINT('Ctrl Pts',(-51.1141102527119,-23.9275319100486,
177.423612084264));
#13865=CARTESIAN_POINT('Ctrl Pts',(-49.9940329966114,-23.4994535030053,
178.148719290634));
#13866=CARTESIAN_POINT('Ctrl Pts',(-49.2531996565364,-23.2503850964097,
178.195074921104));
#13867=CARTESIAN_POINT('Ctrl Pts',(-48.0540724826088,-22.804580182732,177.607487959387));
#13868=CARTESIAN_POINT('Ctrl Pts',(-47.6174629086983,-22.6140260251447,
176.985139741962));
#13869=CARTESIAN_POINT('Ctrl Pts',(-47.4549919432363,-22.3698803060775,
175.609945370482));
#13870=CARTESIAN_POINT('Ctrl Pts',(-47.7329522193418,-22.3169255939418,
174.876470615888));
#13871=CARTESIAN_POINT('Ctrl Pts',(-48.8440385240951,-22.3059754149369,
173.902867041218));
#13872=CARTESIAN_POINT('Ctrl Pts',(-49.7035599970344,-22.3554674780819,
173.739637329099));
#13873=CARTESIAN_POINT('Ctrl Pts',(-51.1531706356154,-22.4011313967338,
174.265066374312));
#13874=CARTESIAN_POINT('Ctrl Pts',(-51.7115054154064,-22.3910761212842,
174.945624054023));
#13875=CARTESIAN_POINT('Ctrl Pts',(-51.9563259347572,-22.2045289991918,
176.459132103654));
#13876=CARTESIAN_POINT('Ctrl Pts',(-51.63765119649,-22.0251559400258,177.262331468575));
#13877=CARTESIAN_POINT('Ctrl Pts',(-50.4571461815608,-21.5627984935069,
178.149907937338));
#13878=CARTESIAN_POINT('Ctrl Pts',(-49.6222512854117,-21.2849471395443,
178.217719280236));
#13879=CARTESIAN_POINT('Ctrl Pts',(-48.3256452005116,-20.7988977065915,
177.525255091295));
#13880=CARTESIAN_POINT('Ctrl Pts',(-47.8935170509031,-20.5993012814682,
176.78942555283));
#13881=CARTESIAN_POINT('Ctrl Pts',(-47.9069259765589,-20.3679964193449,
175.264267840625));
#13882=CARTESIAN_POINT('Ctrl Pts',(-48.3565963500671,-20.33698501403,174.508050023486));
#13883=CARTESIAN_POINT('Ctrl Pts',(-49.7115395236169,-20.3645147337819,
173.767258025586));
#13884=CARTESIAN_POINT('Ctrl Pts',(-50.5919963646361,-20.4163759449694,
173.798730113887));
#13885=CARTESIAN_POINT('Ctrl Pts',(-51.8921615926268,-20.4324111199544,
174.637786957993));
#13886=CARTESIAN_POINT('Ctrl Pts',(-52.2870845316673,-20.391715494119,175.425932171935));
#13887=CARTESIAN_POINT('Ctrl Pts',(-52.1845249551972,-20.1359343420921,
176.949348485014));
#13888=CARTESIAN_POINT('Ctrl Pts',(-51.6978717551623,-19.9258306519252,
177.647217385389));
#13889=CARTESIAN_POINT('Ctrl Pts',(-50.3567743114224,-19.4332812849397,
178.229888643815));
#13890=CARTESIAN_POINT('Ctrl Pts',(-49.531482093434,-19.1564117811874,178.098575810452));
#13891=CARTESIAN_POINT('Ctrl Pts',(-48.4209526978951,-18.7085233315365,
177.123331466978));
#13892=CARTESIAN_POINT('Ctrl Pts',(-48.1597795720535,-18.5402167412103,
176.29718764283));
#13893=CARTESIAN_POINT('Ctrl Pts',(-48.5145782694716,-18.3739619700934,
174.800216258582));
#13894=CARTESIAN_POINT('Ctrl Pts',(-49.1216168980297,-18.3741927637648,
174.159897255644));
#13895=CARTESIAN_POINT('Ctrl Pts',(-50.6124880467131,-18.4256628314289,
173.74530968569));
#13896=CARTESIAN_POINT('Ctrl Pts',(-51.4570089590119,-18.472296203581,173.973986288395));
#13897=CARTESIAN_POINT('Ctrl Pts',(-52.5367755134872,-18.4465314340497,
175.076321400051));
#13898=CARTESIAN_POINT('Ctrl Pts',(-52.7461464663159,-18.3691716102472,
175.928004990245));
#13899=CARTESIAN_POINT('Ctrl Pts',(-52.3166330239091,-18.0526500335514,
177.376965544067));
#13900=CARTESIAN_POINT('Ctrl Pts',(-51.6857211698905,-17.8130496454,177.945754508989));
#13901=CARTESIAN_POINT('Ctrl Pts',(-50.2465394893753,-17.3007990625156,
178.194297846636));
#13902=CARTESIAN_POINT('Ctrl Pts',(-49.4703000985441,-17.0343670318334,
177.871754882023));
#13903=CARTESIAN_POINT('Ctrl Pts',(-48.6088763818932,-16.6321365971318,
176.648991214725));
#13904=CARTESIAN_POINT('Ctrl Pts',(-48.5409020769561,-16.5028432711256,
175.78526591443));
#13905=CARTESIAN_POINT('Ctrl Pts',(-49.2164515058916,-16.3991203888251,
174.401518908745));
#13906=CARTESIAN_POINT('Ctrl Pts',(-49.9496118192587,-16.4227354715302,
173.914202886417));
#13907=CARTESIAN_POINT('Ctrl Pts',(-51.4902606534728,-16.4861638259448,
173.836744887307));
#13908=CARTESIAN_POINT('Ctrl Pts',(-52.2697075969923,-16.5185243960147,
174.249627738192));
#13909=CARTESIAN_POINT('Ctrl Pts',(-53.0792623986938,-16.4399376212412,
175.566241461313));
#13910=CARTESIAN_POINT('Ctrl Pts',(-53.0958608617722,-16.3264383488088,
176.440260240546));
#13911=CARTESIAN_POINT('Ctrl Pts',(-52.3498924896565,-15.9464100326616,
177.743856795072));
#13912=CARTESIAN_POINT('Ctrl Pts',(-51.6136771994172,-15.6882407493956,
178.142477224647));
#13913=CARTESIAN_POINT('Ctrl Pts',(-50.1619939854693,-15.1743526813971,
178.045393567771));
#13914=CARTESIAN_POINT('Ctrl Pts',(-49.479535393056,-14.9249532161513,177.547481856475));
#13915=CARTESIAN_POINT('Ctrl Pts',(-48.9083003859244,-14.5811172796918,
176.154888290848));
#13916=CARTESIAN_POINT('Ctrl Pts',(-49.032687325759,-14.4872017268269,175.286386043965));
#13917=CARTESIAN_POINT('Ctrl Pts',(-50.002899927607,-14.4395306566209,174.08106638639));
#13918=CARTESIAN_POINT('Ctrl Pts',(-50.8258619899905,-14.4815667576624,
173.768688449528));
#13919=CARTESIAN_POINT('Ctrl Pts',(-52.3490472247602,-14.5391579602322,
174.044477097964));
#13920=CARTESIAN_POINT('Ctrl Pts',(-53.0108480437211,-14.5505369630929,
174.618897762295));
#13921=CARTESIAN_POINT('Ctrl Pts',(-53.508606726061,-14.41258118913,176.072854784516));
#13922=CARTESIAN_POINT('Ctrl Pts',(-53.3308496256547,-14.2605010523332,
176.92211652172));
#13923=CARTESIAN_POINT('Ctrl Pts',(-52.3234046589676,-13.8325238003689,
178.011250192421));
#13924=CARTESIAN_POINT('Ctrl Pts',(-51.5138129382755,-13.5585438056648,
178.229366209696));
#13925=CARTESIAN_POINT('Ctrl Pts',(-50.1182607249297,-13.0546721198729,
177.788098654291));
#13926=CARTESIAN_POINT('Ctrl Pts',(-49.5630188185408,-12.8308644828691,
177.140857971114));
#13927=CARTESIAN_POINT('Ctrl Pts',(-49.3219040202974,-12.5483689245281,
175.637957478437));
#13928=CARTESIAN_POINT('Ctrl Pts',(-49.6365594730894,-12.4926951709364,
174.821179942866));
#13929=CARTESIAN_POINT('Ctrl Pts',(-50.8450351424658,-12.4918253386163,
173.862170041067));
#13930=CARTESIAN_POINT('Ctrl Pts',(-51.7160671936879,-12.5420406725331,
173.742988789581));
#13931=CARTESIAN_POINT('Ctrl Pts',(-53.1380531234061,-12.5824907099911,
174.344563971126));
#13932=CARTESIAN_POINT('Ctrl Pts',(-53.661497991413,-12.565516429584,175.054752397452));
#13933=CARTESIAN_POINT('Ctrl Pts',(-53.8242077932451,-12.3622912981454,
176.579637740953));
#13934=CARTESIAN_POINT('Ctrl Pts',(-53.4635573374974,-12.1759538811977,
177.362604506387));
#13935=CARTESIAN_POINT('Ctrl Pts',(-52.2358756182636,-11.7031645393402,
178.179207046235));
#13936=CARTESIAN_POINT('Ctrl Pts',(-51.404471480006,-11.4266005921062,178.198059647233));
#13937=CARTESIAN_POINT('Ctrl Pts',(-50.1465877134854,-10.9499764840513,
177.440684540534));
#13938=CARTESIAN_POINT('Ctrl Pts',(-49.7512566691313,-10.7559713173261,
176.677961727673));
#13939=CARTESIAN_POINT('Ctrl Pts',(-49.8442980389787,-10.5402489724976,
175.152069846099));
#13940=CARTESIAN_POINT('Ctrl Pts',(-50.3336227209985,-10.5166703329192,
174.417963751365));
#13941=CARTESIAN_POINT('Ctrl Pts',(-51.729412313951,-10.5511670115394,173.750914008412));
#13942=CARTESIAN_POINT('Ctrl Pts',(-52.6055357660183,-10.6034581645062,
173.829125569603));
#13943=CARTESIAN_POINT('Ctrl Pts',(-53.8591972775733,-10.6090268187652,
174.739479897504));
#13944=CARTESIAN_POINT('Ctrl Pts',(-54.2075655427863,-10.559958422732,175.542285446703));
#13945=CARTESIAN_POINT('Ctrl Pts',(-54.0309723767407,-10.2919570312328,
177.05153449857));
#13946=CARTESIAN_POINT('Ctrl Pts',(-53.5065211660476,-10.0729835636969,
177.724885949439));
#13947=CARTESIAN_POINT('Ctrl Pts',(-52.1359327706082,-9.57501150980407,
178.231990439602));
#13948=CARTESIAN_POINT('Ctrl Pts',(-51.3168725161042,-9.29919601638729,
178.055337178134));
#13949=CARTESIAN_POINT('Ctrl Pts',(-50.258716477129,-8.86039345968628,177.014257444883));
#13950=CARTESIAN_POINT('Ctrl Pts',(-50.0419858596938,-8.70190296068798,
176.174822144773));
#13951=CARTESIAN_POINT('Ctrl Pts',(-50.4788136762356,-8.55014763089762,
174.697436550109));
#13952=CARTESIAN_POINT('Ctrl Pts',(-51.1165600370436,-8.55674976323144,
174.095019459488));
#13953=CARTESIAN_POINT('Ctrl Pts',(-52.6206590619166,-8.6128620697194,173.755704628284));
#13954=CARTESIAN_POINT('Ctrl Pts',(-53.456626592603,-8.65630954771657,174.029197443714));
#13955=CARTESIAN_POINT('Ctrl Pts',(-54.4781193003427,-8.6195332279715,175.187078119489));
#13956=CARTESIAN_POINT('Ctrl Pts',(-54.643602443466,-8.53353572012608,176.04949882023));
#13957=CARTESIAN_POINT('Ctrl Pts',(-54.1354947853707,-8.20096498746117,
177.472181687833));
#13958=CARTESIAN_POINT('Ctrl Pts',(-53.4760203027823,-7.95706608118669,
178.003825172765));
#13959=CARTESIAN_POINT('Ctrl Pts',(-52.0249165538012,-7.441132564782,178.167825277993));
#13960=CARTESIAN_POINT('Ctrl Pts',(-51.2723007652614,-7.17976116760829,
177.802466009854));
#13961=CARTESIAN_POINT('Ctrl Pts',(-50.4742318046734,-6.79179686888332,
176.539214575509));
#13962=CARTESIAN_POINT('Ctrl Pts',(-50.4508393849021,-6.66952799804251,
175.667365550039));
#13963=CARTESIAN_POINT('Ctrl Pts',(-51.1982775200671,-6.57992894303025,
174.318931761547));
#13964=CARTESIAN_POINT('Ctrl Pts',(-51.9567203354133,-6.60831910752051,
173.869388776842));
#13965=CARTESIAN_POINT('Ctrl Pts',(-53.5030461170827,-6.67180659392302,
173.876188814802));
#13966=CARTESIAN_POINT('Ctrl Pts',(-54.2579318048227,-6.70074853854407,
174.329266762268));
#13967=CARTESIAN_POINT('Ctrl Pts',(-54.9950541895712,-6.6067812144727,175.688231083653));
#13968=CARTESIAN_POINT('Ctrl Pts',(-54.9633937640365,-6.48434226598442,
176.556150922255));
#13969=CARTESIAN_POINT('Ctrl Pts',(-54.1573516980127,-6.0949735677162,177.812809342709));
#13970=CARTESIAN_POINT('Ctrl Pts',(-53.3979887985791,-5.83073710308303,
178.172806822259));
#13971=CARTESIAN_POINT('Ctrl Pts',(-51.9519097716579,-5.31810666795101,
177.994568269632));
#13972=CARTESIAN_POINT('Ctrl Pts',(-51.2952074816856,-5.0735953089356,177.458800517348));
#13973=CARTESIAN_POINT('Ctrl Pts',(-50.7993635736617,-4.74342220821161,
176.031468409862));
#13974=CARTESIAN_POINT('Ctrl Pts',(-50.9692613848378,-4.65940397939939,
175.170313217647));
#13975=CARTESIAN_POINT('Ctrl Pts',(-52.0040245669764,-4.62293999106357,
174.01934301833));
#13976=CARTESIAN_POINT('Ctrl Pts',(-52.8385688131003,-4.66759138415716,
173.754231358386));
#13977=CARTESIAN_POINT('Ctrl Pts',(-54.3414847379305,-4.72329909029368,
174.103969484305));
#13978=CARTESIAN_POINT('Ctrl Pts',(-54.9761466933045,-4.72791014175074,
174.714716972292));
#13979=CARTESIAN_POINT('Ctrl Pts',(-55.3975165431988,-4.57549651155636,
176.192173272167));
#13980=CARTESIAN_POINT('Ctrl Pts',(-55.1760506072609,-4.4148786220368,177.03103539143));
#13981=CARTESIAN_POINT('Ctrl Pts',(-54.1093043232961,-3.97451188101218,
178.061753391873));
#13982=CARTESIAN_POINT('Ctrl Pts',(-53.2902925544343,-3.69995792969149,
178.233822626392));
#13983=CARTESIAN_POINT('Ctrl Pts',(-51.9203920380846,-3.19963469730891,
177.711493690972));
#13984=CARTESIAN_POINT('Ctrl Pts',(-51.4044324721558,-2.98383265912278,
177.036002564632));
#13985=CARTESIAN_POINT('Ctrl Pts',(-51.237949425703,-2.71774512370317,175.525044339462));
#13986=CARTESIAN_POINT('Ctrl Pts',(-51.5957499271559,-2.66894330374766,
174.721509320474));
#13987=CARTESIAN_POINT('Ctrl Pts',(-52.8541051305037,-2.67783999801612,
173.825937213487));
#13988=CARTESIAN_POINT('Ctrl Pts',(-53.7315999697276,-2.7292086653859,173.7525048498));
#13989=CARTESIAN_POINT('Ctrl Pts',(-55.1208667949195,-2.76252327401043,
174.431246184642));
#13990=CARTESIAN_POINT('Ctrl Pts',(-55.6054709668258,-2.73893798071373,
175.167402226862));
#13991=CARTESIAN_POINT('Ctrl Pts',(-55.6603171863937,-2.58869274068622,
176.211840888345));
#13992=CARTESIAN_POINT('Ctrl Pts',(-55.6210463302226,-2.5392081864434,176.490448482462));
#13993=CARTESIAN_POINT('Ctrl Pts',(-55.4836397365907,-2.4479441182576,176.880586390838));
#13994=CARTESIAN_POINT('Ctrl Pts',(-55.4253285390117,-2.41535251334816,
177.005027857449));
#13995=CARTESIAN_POINT('Ctrl Pts',(-55.321414213033,-2.36345060131236,177.180440236558));
#13996=CARTESIAN_POINT('Ctrl Pts',(-55.2840225057543,-2.34563722905757,
177.23703696138));
#13997=CARTESIAN_POINT('Ctrl Pts',(-55.2039936793606,-2.30896761153951,
177.345998347345));
#13998=CARTESIAN_POINT('Ctrl Pts',(-55.1587206712145,-2.28906361698866,
177.401367187303));
#13999=CARTESIAN_POINT('Ctrl Pts',(-55.1161897096451,-2.27071607222657,
177.448351373365));
#14000=CARTESIAN_POINT('Ctrl Pts',(-47.8886718415116,-31.6995536639001,
175.585485069079));
#14001=CARTESIAN_POINT('Ctrl Pts',(-47.9424090991571,-31.4208895534118,
175.585485069079));
#14002=CARTESIAN_POINT('Ctrl Pts',(-48.0165136638412,-31.142217631488,175.587595470504));
#14003=CARTESIAN_POINT('Ctrl Pts',(-48.206190379979,-30.6092681473582,175.5992945923));
#14004=CARTESIAN_POINT('Ctrl Pts',(-48.3219855416571,-30.3543443720961,
175.608895409754));
#14005=CARTESIAN_POINT('Ctrl Pts',(-48.7193595355016,-29.6463117438825,
175.654781597023));
#14006=CARTESIAN_POINT('Ctrl Pts',(-49.0545911241397,-29.252967076522,175.707428551708));
#14007=CARTESIAN_POINT('Ctrl Pts',(-49.5445318563166,-28.7861739714513,
175.852028081795));
#14008=CARTESIAN_POINT('Ctrl Pts',(-49.6987397911889,-28.6436248452838,
175.911397856293));
#14009=CARTESIAN_POINT('Ctrl Pts',(-49.9262155871255,-28.4691236019893,
176.025260422827));
#14010=CARTESIAN_POINT('Ctrl Pts',(-50.0186861454797,-28.4371266816906,
176.06691518842));
#14011=CARTESIAN_POINT('Ctrl Pts',(-50.1842299781189,-28.3689363752761,
176.173317219728));
#14012=CARTESIAN_POINT('Ctrl Pts',(-50.2569026354171,-28.3307458842207,
176.235836425973));
#14013=CARTESIAN_POINT('Ctrl Pts',(-50.4390882192945,-28.20291241382,176.455121758264));
#14014=CARTESIAN_POINT('Ctrl Pts',(-50.5079392950738,-28.0960057551614,
176.657103040121));
#14015=CARTESIAN_POINT('Ctrl Pts',(-50.4672993044493,-27.9634501974094,
176.968869644582));
#14016=CARTESIAN_POINT('Ctrl Pts',(-50.4326818607288,-27.9245995634275,
177.070967051899));
#14017=CARTESIAN_POINT('Ctrl Pts',(-50.3339110252539,-27.8569369682875,
177.264936028611));
#14018=CARTESIAN_POINT('Ctrl Pts',(-50.2683927599471,-27.8299386004748,
177.362186354007));
#14019=CARTESIAN_POINT('Ctrl Pts',(-50.193114320713,-27.8005016688432,177.448440461337));
#14020=CARTESIAN_POINT('Ctrl Pts',(-47.1031441589869,-31.5480734342088,
175.585485069079));
#14021=CARTESIAN_POINT('Ctrl Pts',(-47.1603662041614,-31.2513383379729,
175.585485069079));
#14022=CARTESIAN_POINT('Ctrl Pts',(-47.2482359974308,-30.9149655772776,
175.587875715227));
#14023=CARTESIAN_POINT('Ctrl Pts',(-47.4670950242505,-30.3000308864083,
175.601419934118));
#14024=CARTESIAN_POINT('Ctrl Pts',(-47.6018961077871,-30.0028542362142,
175.612574303893));
#14025=CARTESIAN_POINT('Ctrl Pts',(-48.06625584225,-29.1754899206181,175.666311941427));
#14026=CARTESIAN_POINT('Ctrl Pts',(-48.4618683742085,-28.7136853353929,
175.729732505271));
#14027=CARTESIAN_POINT('Ctrl Pts',(-49.0063756293611,-28.1949480459011,
175.890763292055));
#14028=CARTESIAN_POINT('Ctrl Pts',(-49.1677731230246,-28.0480163131157,
175.972468320302));
#14029=CARTESIAN_POINT('Ctrl Pts',(-49.3965343491423,-27.8703147335455,
176.056354650694));
#14030=CARTESIAN_POINT('Ctrl Pts',(-49.5042735598544,-27.8224509492496,
176.029622920355));
#14031=CARTESIAN_POINT('Ctrl Pts',(-49.714154138436,-27.7365778903946,176.021696276872));
#14032=CARTESIAN_POINT('Ctrl Pts',(-49.8092250008766,-27.6958009021663,
176.040400247712));
#14033=CARTESIAN_POINT('Ctrl Pts',(-50.0526599599857,-27.5670382667944,
176.149507116298));
#14034=CARTESIAN_POINT('Ctrl Pts',(-50.1573360552302,-27.4697774585579,
176.29868387691));
#14035=CARTESIAN_POINT('Ctrl Pts',(-50.1883082447542,-27.3362137867349,
176.557013250615));
#14036=CARTESIAN_POINT('Ctrl Pts',(-50.1794299894878,-27.2944646349798,
176.647304730812));
#14037=CARTESIAN_POINT('Ctrl Pts',(-50.1311335533471,-27.2163290407286,
176.829965813571));
#14038=CARTESIAN_POINT('Ctrl Pts',(-50.0905156624001,-27.1753600677279,
176.937389673553));
#14039=CARTESIAN_POINT('Ctrl Pts',(-50.0383214665825,-27.1440081492037,
177.018259765604));
#14040=CARTESIAN_POINT('Ctrl Pts',(-47.1031441589869,-31.5480734342088,
176.385485069079));
#14041=CARTESIAN_POINT('Ctrl Pts',(-47.1599854936771,-31.2533125799253,
176.385485069079));
#14042=CARTESIAN_POINT('Ctrl Pts',(-47.2462550636215,-30.9240508319461,
176.387855155919));
#14043=CARTESIAN_POINT('Ctrl Pts',(-47.460249087206,-30.3229192382893,176.401096636113));
#14044=CARTESIAN_POINT('Ctrl Pts',(-47.5913742255291,-30.0344018731676,
176.411980487031));
#14045=CARTESIAN_POINT('Ctrl Pts',(-48.0375122982338,-29.2397387684011,
176.463601555155));
#14046=CARTESIAN_POINT('Ctrl Pts',(-48.4124469809922,-28.8074108937189,
176.525602813253));
#14047=CARTESIAN_POINT('Ctrl Pts',(-48.8848496853331,-28.3577893519108,
176.665278154737));
#14048=CARTESIAN_POINT('Ctrl Pts',(-49.026848150992,-28.2513597906944,176.736022770841));
#14049=CARTESIAN_POINT('Ctrl Pts',(-49.1705854582322,-28.1079648662814,
176.786782875481));
#14050=CARTESIAN_POINT('Ctrl Pts',(-49.2060240792629,-28.0278386987345,
176.747088553392));
#14051=CARTESIAN_POINT('Ctrl Pts',(-49.2810889004422,-27.9003322593211,
176.67860791329));
#14052=CARTESIAN_POINT('Ctrl Pts',(-49.3144205003265,-27.8541778608178,
176.654181717029));
#14053=CARTESIAN_POINT('Ctrl Pts',(-49.3895778283813,-27.7529515714288,
176.588058724708));
#14054=CARTESIAN_POINT('Ctrl Pts',(-49.4143850760995,-27.7397337398683,
176.533088088996));
#14055=CARTESIAN_POINT('Ctrl Pts',(-49.4653959512805,-27.6892053509014,
176.504625861351));
#14056=CARTESIAN_POINT('Ctrl Pts',(-49.480846052191,-27.6666966453102,176.508814220202));
#14057=CARTESIAN_POINT('Ctrl Pts',(-49.4871117159947,-27.6078471194517,
176.551208753368));
#14058=CARTESIAN_POINT('Ctrl Pts',(-49.4794905861727,-27.5632681966532,
176.593760604048));
#14059=CARTESIAN_POINT('Ctrl Pts',(-49.4509304485228,-27.5317240793367,
176.63793339336));
#14060=CARTESIAN_POINT('Ctrl Pts',(-47.8886718415116,-31.6995536639001,
176.385485069079));
#14061=CARTESIAN_POINT('Ctrl Pts',(-47.9420283886728,-31.4228637953642,
176.385485069079));
#14062=CARTESIAN_POINT('Ctrl Pts',(-48.014532730032,-31.1513028861565,176.387574911196));
#14063=CARTESIAN_POINT('Ctrl Pts',(-48.1993444429345,-30.6321564992392,
176.398971294295));
#14064=CARTESIAN_POINT('Ctrl Pts',(-48.3114636593991,-30.3858920090494,
176.408301592892));
#14065=CARTESIAN_POINT('Ctrl Pts',(-48.6906159914853,-29.7105605916654,
176.452071210751));
#14066=CARTESIAN_POINT('Ctrl Pts',(-49.0051697309234,-29.3466926348484,
176.50329885969));
#14067=CARTESIAN_POINT('Ctrl Pts',(-49.4230059122887,-28.9490152774608,
176.626542944478));
#14068=CARTESIAN_POINT('Ctrl Pts',(-49.5578148191563,-28.8469683228627,
176.674952306832));
#14069=CARTESIAN_POINT('Ctrl Pts',(-49.7002666962155,-28.7067737347251,
176.755688647613));
#14070=CARTESIAN_POINT('Ctrl Pts',(-49.7204366648883,-28.6425144311754,
176.784380821457));
#14071=CARTESIAN_POINT('Ctrl Pts',(-49.7511647401251,-28.5326907442027,
176.830228856146));
#14072=CARTESIAN_POINT('Ctrl Pts',(-49.7620981348669,-28.4891228428723,
176.849617895289));
#14073=CARTESIAN_POINT('Ctrl Pts',(-49.7760060876902,-28.3888257184543,
176.893673366674));
#14074=CARTESIAN_POINT('Ctrl Pts',(-49.764988315943,-28.3659620364717,176.891507252207));
#14075=CARTESIAN_POINT('Ctrl Pts',(-49.7443870109756,-28.3164417615759,
176.916482255318));
#14076=CARTESIAN_POINT('Ctrl Pts',(-49.7340979234319,-28.2968315737579,
176.932476541289));
#14077=CARTESIAN_POINT('Ctrl Pts',(-49.6898891879014,-28.2484550470107,
176.986178968408));
#14078=CARTESIAN_POINT('Ctrl Pts',(-49.6573676837196,-28.2178467294001,
177.018557284502));
#14079=CARTESIAN_POINT('Ctrl Pts',(-49.6057233026532,-28.1882175989763,
177.068114089093));
#14080=CARTESIAN_POINT('Ctrl Pts',(-48.6741995240363,-31.8510338935913,
176.385485069079));
#14081=CARTESIAN_POINT('Ctrl Pts',(-48.7240712836685,-31.5924150108031,
176.385485069079));
#14082=CARTESIAN_POINT('Ctrl Pts',(-48.7828103964424,-31.3785549403669,
176.387294666473));
#14083=CARTESIAN_POINT('Ctrl Pts',(-48.9384397986629,-30.941393760189,176.396845952478));
#14084=CARTESIAN_POINT('Ctrl Pts',(-49.0315530932691,-30.7373821449313,
176.404622698753));
#14085=CARTESIAN_POINT('Ctrl Pts',(-49.3437196847369,-30.1813824149298,
176.440540866346));
#14086=CARTESIAN_POINT('Ctrl Pts',(-49.5978924808545,-29.8859743759779,
176.480994906127));
#14087=CARTESIAN_POINT('Ctrl Pts',(-49.9611621392443,-29.5402412030108,
176.587807734218));
#14088=CARTESIAN_POINT('Ctrl Pts',(-50.0887814873205,-29.442576855031,176.613881842823));
#14089=CARTESIAN_POINT('Ctrl Pts',(-50.2299479341988,-29.3055826031689,
176.724594419746));
#14090=CARTESIAN_POINT('Ctrl Pts',(-50.2348492505137,-29.2571901636164,
176.821673089522));
#14091=CARTESIAN_POINT('Ctrl Pts',(-50.221240579808,-29.1650492290843,176.981849799003));
#14092=CARTESIAN_POINT('Ctrl Pts',(-50.2097757694073,-29.1240678249268,
177.04505407355));
#14093=CARTESIAN_POINT('Ctrl Pts',(-50.162434346999,-29.0246998654798,177.199288008639));
#14094=CARTESIAN_POINT('Ctrl Pts',(-50.1155915557866,-28.9921903330752,
177.249926415417));
#14095=CARTESIAN_POINT('Ctrl Pts',(-50.0233780706706,-28.9436781722504,
177.328338649285));
#14096=CARTESIAN_POINT('Ctrl Pts',(-49.9873497946729,-28.9269665022055,
177.356138862376));
#14097=CARTESIAN_POINT('Ctrl Pts',(-49.8926666598081,-28.8890629745697,
177.421149183448));
#14098=CARTESIAN_POINT('Ctrl Pts',(-49.8352447812666,-28.872425262147,177.443353964955));
#14099=CARTESIAN_POINT('Ctrl Pts',(-49.7605161567837,-28.8447111186158,
177.498294784826));
#14100=CARTESIAN_POINT('Ctrl Pts',(-48.6741995240363,-31.8510338935913,
175.585485069079));
#14101=CARTESIAN_POINT('Ctrl Pts',(-48.7244519941528,-31.5904407688506,
175.585485069079));
#14102=CARTESIAN_POINT('Ctrl Pts',(-48.7847913302516,-31.3694696856984,
175.587315225781));
#14103=CARTESIAN_POINT('Ctrl Pts',(-48.9452857357075,-30.918505408308,175.597169250483));
#14104=CARTESIAN_POINT('Ctrl Pts',(-49.042074975527,-30.7058345079779,175.605216515615));
#14105=CARTESIAN_POINT('Ctrl Pts',(-49.3724632287533,-30.1171335671469,
175.643251252618));
#14106=CARTESIAN_POINT('Ctrl Pts',(-49.6473138740709,-29.7922488176511,
175.685124598145));
#14107=CARTESIAN_POINT('Ctrl Pts',(-50.0826880832722,-29.3773998970014,
175.813292871536));
#14108=CARTESIAN_POINT('Ctrl Pts',(-50.2297064593532,-29.239233377452,175.850327392284));
#14109=CARTESIAN_POINT('Ctrl Pts',(-50.4558968251088,-29.0679324704331,
175.99416619496));
#14110=CARTESIAN_POINT('Ctrl Pts',(-50.5330987311051,-29.0518024141316,
176.104207456485));
#14111=CARTESIAN_POINT('Ctrl Pts',(-50.6543058178018,-29.0012948601576,
176.324938162585));
#14112=CARTESIAN_POINT('Ctrl Pts',(-50.7045802699575,-28.9656908662752,
176.431272604233));
#14113=CARTESIAN_POINT('Ctrl Pts',(-50.8255164786033,-28.8387865608456,
176.760736400229));
#14114=CARTESIAN_POINT('Ctrl Pts',(-50.8585425349173,-28.722234051765,177.015522203332));
#14115=CARTESIAN_POINT('Ctrl Pts',(-50.7462903641443,-28.5906866080838,
177.38072603855));
#14116=CARTESIAN_POINT('Ctrl Pts',(-50.6859337319697,-28.5547344918753,
177.494629372986));
#14117=CARTESIAN_POINT('Ctrl Pts',(-50.5366884971606,-28.4975448958465,
177.699906243651));
#14118=CARTESIAN_POINT('Ctrl Pts',(-50.446269857494,-28.4845171332217,177.786983034461));
#14119=CARTESIAN_POINT('Ctrl Pts',(-50.3479071748434,-28.4569951884828,
177.87862115707));
#14120=CARTESIAN_POINT('Ctrl Pts',(-47.8886718415116,-31.6995536639001,
175.585485069079));
#14121=CARTESIAN_POINT('Ctrl Pts',(-47.9424090991571,-31.4208895534118,
175.585485069079));
#14122=CARTESIAN_POINT('Ctrl Pts',(-48.0165136638412,-31.142217631488,175.587595470504));
#14123=CARTESIAN_POINT('Ctrl Pts',(-48.206190379979,-30.6092681473582,175.5992945923));
#14124=CARTESIAN_POINT('Ctrl Pts',(-48.3219855416571,-30.3543443720961,
175.608895409754));
#14125=CARTESIAN_POINT('Ctrl Pts',(-48.7193595355016,-29.6463117438825,
175.654781597023));
#14126=CARTESIAN_POINT('Ctrl Pts',(-49.0545911241397,-29.252967076522,175.707428551708));
#14127=CARTESIAN_POINT('Ctrl Pts',(-49.5445318563166,-28.7861739714513,
175.852028081795));
#14128=CARTESIAN_POINT('Ctrl Pts',(-49.6987397911889,-28.6436248452838,
175.911397856293));
#14129=CARTESIAN_POINT('Ctrl Pts',(-49.9262155871255,-28.4691236019893,
176.025260422827));
#14130=CARTESIAN_POINT('Ctrl Pts',(-50.0186861454797,-28.4371266816906,
176.06691518842));
#14131=CARTESIAN_POINT('Ctrl Pts',(-50.1842299781189,-28.3689363752761,
176.173317219728));
#14132=CARTESIAN_POINT('Ctrl Pts',(-50.2569026354171,-28.3307458842207,
176.235836425973));
#14133=CARTESIAN_POINT('Ctrl Pts',(-50.4390882192945,-28.20291241382,176.455121758264));
#14134=CARTESIAN_POINT('Ctrl Pts',(-50.5079392950738,-28.0960057551614,
176.657103040121));
#14135=CARTESIAN_POINT('Ctrl Pts',(-50.4672993044493,-27.9634501974094,
176.968869644582));
#14136=CARTESIAN_POINT('Ctrl Pts',(-50.4326818607288,-27.9245995634275,
177.070967051899));
#14137=CARTESIAN_POINT('Ctrl Pts',(-50.3339110252539,-27.8569369682875,
177.264936028611));
#14138=CARTESIAN_POINT('Ctrl Pts',(-50.2683927599471,-27.8299386004748,
177.362186354007));
#14139=CARTESIAN_POINT('Ctrl Pts',(-50.193114320713,-27.8005016688432,177.448440461337));
#14140=CARTESIAN_POINT('',(-47.8886718415116,-31.6995536639001,176.385485069079));
#14141=CARTESIAN_POINT('',(-47.8886718415116,-31.6995536639001,175.585485069079));
#14142=CARTESIAN_POINT('Origin',(-47.8886718415116,-31.6995536639001,175.985485069079));
#14143=CARTESIAN_POINT('Ctrl Pts',(-47.8886718415116,-31.6995536639001,
176.385485069079));
#14144=CARTESIAN_POINT('Ctrl Pts',(-47.9420283886728,-31.4228637953642,
176.385485069079));
#14145=CARTESIAN_POINT('Ctrl Pts',(-48.014532730032,-31.1513028861565,176.387574911196));
#14146=CARTESIAN_POINT('Ctrl Pts',(-48.1993444429345,-30.6321564992392,
176.398971294295));
#14147=CARTESIAN_POINT('Ctrl Pts',(-48.3114636593991,-30.3858920090494,
176.408301592892));
#14148=CARTESIAN_POINT('Ctrl Pts',(-48.6906159914853,-29.7105605916654,
176.452071210751));
#14149=CARTESIAN_POINT('Ctrl Pts',(-49.0051697309234,-29.3466926348484,
176.50329885969));
#14150=CARTESIAN_POINT('Ctrl Pts',(-49.4230059122887,-28.9490152774608,
176.626542944478));
#14151=CARTESIAN_POINT('Ctrl Pts',(-49.5578148191563,-28.8469683228627,
176.674952306832));
#14152=CARTESIAN_POINT('Ctrl Pts',(-49.7002666962155,-28.7067737347251,
176.755688647613));
#14153=CARTESIAN_POINT('Ctrl Pts',(-49.7204366648883,-28.6425144311754,
176.784380821457));
#14154=CARTESIAN_POINT('Ctrl Pts',(-49.7511647401251,-28.5326907442027,
176.830228856146));
#14155=CARTESIAN_POINT('Ctrl Pts',(-49.7620981348669,-28.4891228428723,
176.849617895289));
#14156=CARTESIAN_POINT('Ctrl Pts',(-49.7760060876902,-28.3888257184543,
176.893673366674));
#14157=CARTESIAN_POINT('Ctrl Pts',(-49.764988315943,-28.3659620364717,176.891507252207));
#14158=CARTESIAN_POINT('Ctrl Pts',(-49.7443870109756,-28.3164417615759,
176.916482255318));
#14159=CARTESIAN_POINT('Ctrl Pts',(-49.7340979234319,-28.2968315737579,
176.932476541289));
#14160=CARTESIAN_POINT('Ctrl Pts',(-49.6898891879014,-28.2484550470107,
176.986178968408));
#14161=CARTESIAN_POINT('Ctrl Pts',(-49.6573676837196,-28.2178467294001,
177.018557284502));
#14162=CARTESIAN_POINT('Ctrl Pts',(-49.6057233026533,-28.1882175989763,
177.068114089093));
#14163=CARTESIAN_POINT('Ctrl Pts',(-47.8886718415116,-31.6995536639001,
175.585485069079));
#14164=CARTESIAN_POINT('Ctrl Pts',(-47.9424090991571,-31.4208895534118,
175.585485069079));
#14165=CARTESIAN_POINT('Ctrl Pts',(-48.0165136638412,-31.142217631488,175.587595470504));
#14166=CARTESIAN_POINT('Ctrl Pts',(-48.206190379979,-30.6092681473582,175.5992945923));
#14167=CARTESIAN_POINT('Ctrl Pts',(-48.3219855416571,-30.3543443720961,
175.608895409754));
#14168=CARTESIAN_POINT('Ctrl Pts',(-48.7193595355016,-29.6463117438825,
175.654781597023));
#14169=CARTESIAN_POINT('Ctrl Pts',(-49.0545911241397,-29.252967076522,175.707428551708));
#14170=CARTESIAN_POINT('Ctrl Pts',(-49.5445318563166,-28.7861739714513,
175.852028081795));
#14171=CARTESIAN_POINT('Ctrl Pts',(-49.6987397911889,-28.6436248452838,
175.911397856293));
#14172=CARTESIAN_POINT('Ctrl Pts',(-49.9262155871255,-28.4691236019893,
176.025260422827));
#14173=CARTESIAN_POINT('Ctrl Pts',(-50.0186861454797,-28.4371266816906,
176.06691518842));
#14174=CARTESIAN_POINT('Ctrl Pts',(-50.1842299781189,-28.3689363752761,
176.173317219728));
#14175=CARTESIAN_POINT('Ctrl Pts',(-50.2569026354171,-28.3307458842207,
176.235836425973));
#14176=CARTESIAN_POINT('Ctrl Pts',(-50.4390882192945,-28.20291241382,176.455121758264));
#14177=CARTESIAN_POINT('Ctrl Pts',(-50.5079392950738,-28.0960057551614,
176.657103040121));
#14178=CARTESIAN_POINT('Ctrl Pts',(-50.4672993044493,-27.9634501974094,
176.968869644582));
#14179=CARTESIAN_POINT('Ctrl Pts',(-50.4326818607288,-27.9245995634275,
177.070967051899));
#14180=CARTESIAN_POINT('Ctrl Pts',(-50.3339110252539,-27.8569369682875,
177.264936028611));
#14181=CARTESIAN_POINT('Ctrl Pts',(-50.2683927599471,-27.8299386004748,
177.362186354007));
#14182=CARTESIAN_POINT('Ctrl Pts',(-50.193114320713,-27.8005016688432,177.448440461337));
#14183=CARTESIAN_POINT('Origin',(-47.8413342697331,-31.9450310646891,175.985485069079));
#14184=CARTESIAN_POINT('',(-47.8413342697331,-31.9450310646891,175.585485069079));
#14185=CARTESIAN_POINT('Origin',(-47.8886718415116,-31.6995536639001,175.985485069079));
#14186=CARTESIAN_POINT('Ctrl Pts',(-55.1161897096451,-2.27071607222657,
177.448351373365));
#14187=CARTESIAN_POINT('Ctrl Pts',(-55.0544324803005,-2.24407445661358,
177.516574922684));
#14188=CARTESIAN_POINT('Ctrl Pts',(-55.0031840696463,-2.2159075942787,177.564829510218));
#14189=CARTESIAN_POINT('Ctrl Pts',(-54.8981614763103,-2.14735807337978,
177.649345866972));
#14190=CARTESIAN_POINT('Ctrl Pts',(-54.848196955649,-2.10845499517373,177.68122338125));
#14191=CARTESIAN_POINT('Ctrl Pts',(-54.7062455015458,-1.97869616397794,
177.747598981208));
#14192=CARTESIAN_POINT('Ctrl Pts',(-54.6230552819493,-1.87505607340526,
177.751980177594));
#14193=CARTESIAN_POINT('Ctrl Pts',(-54.4781164600507,-1.64599936204779,
177.704020550018));
#14194=CARTESIAN_POINT('Ctrl Pts',(-54.4161687409529,-1.52036398038793,
177.652507519121));
#14195=CARTESIAN_POINT('Ctrl Pts',(-54.3240884061122,-1.31623292778147,
177.552502738263));
#14196=CARTESIAN_POINT('Ctrl Pts',(-54.2900300114527,-1.2450809441322,177.5168693343));
#14197=CARTESIAN_POINT('Ctrl Pts',(-54.2388806708887,-1.10092476185966,
177.429650782512));
#14198=CARTESIAN_POINT('Ctrl Pts',(-54.2230625419579,-1.02814126447079,
177.378422455576));
#14199=CARTESIAN_POINT('Ctrl Pts',(-54.1687570862725,-0.661100958902222,
177.107656526019));
#14200=CARTESIAN_POINT('Ctrl Pts',(-54.1632550913909,-0.344986943697024,
176.855601626641));
#14201=CARTESIAN_POINT('Ctrl Pts',(-54.1894883174704,0.100428951784895,
176.57062132681));
#14202=CARTESIAN_POINT('Ctrl Pts',(-54.2038650968969,0.243821813285216,
176.491645489995));
#14203=CARTESIAN_POINT('Ctrl Pts',(-54.2289503028814,0.435912884592043,
176.413053638658));
#14204=CARTESIAN_POINT('Ctrl Pts',(-54.2378694870404,0.495988408430007,
176.393461416067));
#14205=CARTESIAN_POINT('Ctrl Pts',(-54.2511575637744,0.57777536525398,176.374426535183));
#14206=CARTESIAN_POINT('Ctrl Pts',(-54.2555861991508,0.603644576350343,
176.369782059628));
#14207=CARTESIAN_POINT('Ctrl Pts',(-54.2642818917577,0.652365455860021,
176.363705099944));
#14208=CARTESIAN_POINT('Ctrl Pts',(-54.2669281652524,0.666814619551347,
176.362269083675));
#14209=CARTESIAN_POINT('Ctrl Pts',(-54.2726708967805,0.696594575640996,
176.362269083675));
#14210=CARTESIAN_POINT('Ctrl Pts',(-54.9611536226478,-1.61438316700751,
177.018013216499));
#14211=CARTESIAN_POINT('Ctrl Pts',(-54.9292844549615,-1.59689979741686,
177.061501366048));
#14212=CARTESIAN_POINT('Ctrl Pts',(-54.9347169869457,-1.59513306644644,
177.059466012753));
#14213=CARTESIAN_POINT('Ctrl Pts',(-54.9393829236175,-1.59207559169288,
177.070205982371));
#14214=CARTESIAN_POINT('Ctrl Pts',(-54.9521671405265,-1.59794122115585,
177.067981920184));
#14215=CARTESIAN_POINT('Ctrl Pts',(-55.0007420885566,-1.63157855374127,
177.067321317852));
#14216=CARTESIAN_POINT('Ctrl Pts',(-55.035179086296,-1.66960295600012,177.085015349648));
#14217=CARTESIAN_POINT('Ctrl Pts',(-55.0396054390644,-1.63669166623166,
177.119603765033));
#14218=CARTESIAN_POINT('Ctrl Pts',(-55.0210115508064,-1.57122240422777,
177.125346825549));
#14219=CARTESIAN_POINT('Ctrl Pts',(-54.9916258301057,-1.40601129473046,
177.119012727072));
#14220=CARTESIAN_POINT('Ctrl Pts',(-54.9808143890584,-1.33515491542406,
177.122292216748));
#14221=CARTESIAN_POINT('Ctrl Pts',(-54.95716312305,-1.20146912437994,177.090609934045));
#14222=CARTESIAN_POINT('Ctrl Pts',(-54.9459301778233,-1.14025139494389,
177.054154311007));
#14223=CARTESIAN_POINT('Ctrl Pts',(-54.9010485418089,-0.837221085805294,
176.830475957374));
#14224=CARTESIAN_POINT('Ctrl Pts',(-54.8933924651384,-0.543523047070829,
176.59567568837));
#14225=CARTESIAN_POINT('Ctrl Pts',(-54.9188659939004,-0.109419407590943,
176.317655840143));
#14226=CARTESIAN_POINT('Ctrl Pts',(-54.9330773739472,0.0346181647599921,
176.23753447689));
#14227=CARTESIAN_POINT('Ctrl Pts',(-54.9598081399055,0.239682185419695,
176.153510553493));
#14228=CARTESIAN_POINT('Ctrl Pts',(-54.9696067027056,0.306181698359097,
176.131488679163));
#14229=CARTESIAN_POINT('Ctrl Pts',(-54.985167831776,0.402075433542801,176.109129772912));
#14230=CARTESIAN_POINT('Ctrl Pts',(-54.9905018003277,0.433390482627809,
176.103410426781));
#14231=CARTESIAN_POINT('Ctrl Pts',(-55.0013966992521,0.494658609580997,
176.095691012754));
#14232=CARTESIAN_POINT('Ctrl Pts',(-55.0061011366799,0.520171112552638,
176.093689066957));
#14233=CARTESIAN_POINT('Ctrl Pts',(-55.012606581275,0.553906252953576,176.093689066957));
#14234=CARTESIAN_POINT('Ctrl Pts',(-54.3738267566562,-2.00237092626598,
176.637865020199));
#14235=CARTESIAN_POINT('Ctrl Pts',(-54.3525463517218,-1.98561856641678,
176.665739674622));
#14236=CARTESIAN_POINT('Ctrl Pts',(-54.3544769039845,-1.9794317280201,176.664843524849));
#14237=CARTESIAN_POINT('Ctrl Pts',(-54.3701639946021,-1.97656111293176,
176.660021126843));
#14238=CARTESIAN_POINT('Ctrl Pts',(-54.3898340629218,-1.98406009722412,
176.649873028566));
#14239=CARTESIAN_POINT('Ctrl Pts',(-54.4615150878692,-2.02680400188237,
176.627416363355));
#14240=CARTESIAN_POINT('Ctrl Pts',(-54.5129888400511,-2.0757703324506,176.634526145744));
#14241=CARTESIAN_POINT('Ctrl Pts',(-54.5552784049148,-2.06122690211322,
176.64442773024));
#14242=CARTESIAN_POINT('Ctrl Pts',(-54.5578076149692,-2.0038135240127,176.634785085717));
#14243=CARTESIAN_POINT('Ctrl Pts',(-54.5892177302657,-1.85411233048761,
176.591889300217));
#14244=CARTESIAN_POINT('Ctrl Pts',(-54.610530702465,-1.78996529622254,176.577740776828));
#14245=CARTESIAN_POINT('Ctrl Pts',(-54.6268123436843,-1.66507238716025,
176.528080652247));
#14246=CARTESIAN_POINT('Ctrl Pts',(-54.6208424301061,-1.60549754243094,
176.490359176158));
#14247=CARTESIAN_POINT('Ctrl Pts',(-54.5752745689856,-1.29850461246565,
176.263815183543));
#14248=CARTESIAN_POINT('Ctrl Pts',(-54.5643152196599,-0.983878310891091,
176.010083812441));
#14249=CARTESIAN_POINT('Ctrl Pts',(-54.5948528025329,-0.459382509277473,
175.674365954678));
#14250=CARTESIAN_POINT('Ctrl Pts',(-54.6123879900288,-0.274694122222572,
175.56925971577));
#14251=CARTESIAN_POINT('Ctrl Pts',(-54.6518354905867,0.0289042342998165,
175.444989413561));
#14252=CARTESIAN_POINT('Ctrl Pts',(-54.6672255747517,0.134792609497288,
175.409177545969));
#14253=CARTESIAN_POINT('Ctrl Pts',(-54.6945480274656,0.303452837912914,
175.369907772329));
#14254=CARTESIAN_POINT('Ctrl Pts',(-54.7043366789371,0.361315642399545,
175.359237745269));
#14255=CARTESIAN_POINT('Ctrl Pts',(-54.7254408307236,0.480524258303587,
175.344341053851));
#14256=CARTESIAN_POINT('Ctrl Pts',(-54.7391421008419,0.554236948300629,
175.340121037765));
#14257=CARTESIAN_POINT('Ctrl Pts',(-54.7488852836436,0.604761956232279,
175.340121037765));
#14258=CARTESIAN_POINT('Ctrl Pts',(-54.5288628436534,-2.65870383148503,
177.068203177065));
#14259=CARTESIAN_POINT('Ctrl Pts',(-54.4776943770608,-2.6327932256135,177.120813231257));
#14260=CARTESIAN_POINT('Ctrl Pts',(-54.4229439866851,-2.60020625585236,
177.170207022314));
#14261=CARTESIAN_POINT('Ctrl Pts',(-54.3289425472948,-2.53184359461866,
177.239161011444));
#14262=CARTESIAN_POINT('Ctrl Pts',(-54.2858638780443,-2.494573871242,177.263114489632));
#14263=CARTESIAN_POINT('Ctrl Pts',(-54.1670185008584,-2.37392161211904,
177.307694026711));
#14264=CARTESIAN_POINT('Ctrl Pts',(-54.1008650357044,-2.28122344985573,
177.30149097369));
#14265=CARTESIAN_POINT('Ctrl Pts',(-53.9937894259011,-2.07053459792936,
177.228844515225));
#14266=CARTESIAN_POINT('Ctrl Pts',(-53.9529648051158,-1.95295510017287,
177.161945779289));
#14267=CARTESIAN_POINT('Ctrl Pts',(-53.9216803062721,-1.76433396353862,
177.025379311408));
#14268=CARTESIAN_POINT('Ctrl Pts',(-53.9197463248593,-1.6998913249307,176.97231789438));
#14269=CARTESIAN_POINT('Ctrl Pts',(-53.9085298915231,-1.56452802463996,
176.867121500714));
#14270=CARTESIAN_POINT('Ctrl Pts',(-53.8979747942407,-1.4933874119578,176.814627320727));
#14271=CARTESIAN_POINT('Ctrl Pts',(-53.8429831134493,-1.12238448556273,
176.540995752188));
#14272=CARTESIAN_POINT('Ctrl Pts',(-53.8341778459125,-0.785342207517119,
176.270009750712));
#14273=CARTESIAN_POINT('Ctrl Pts',(-53.8654751261029,-0.249534149901716,
175.927331441344));
#14274=CARTESIAN_POINT('Ctrl Pts',(-53.8831757129786,-0.0654904736973553,
175.823370728875));
#14275=CARTESIAN_POINT('Ctrl Pts',(-53.9209776535626,0.225134933472168,
175.704532498726));
#14276=CARTESIAN_POINT('Ctrl Pts',(-53.9354883590865,0.324599319568198,
175.671150282872));
#14277=CARTESIAN_POINT('Ctrl Pts',(-53.960537759464,0.479152769624093,175.6352045346));
#14278=CARTESIAN_POINT('Ctrl Pts',(-53.9694210777602,0.531569736122078,
175.625609378116));
#14279=CARTESIAN_POINT('Ctrl Pts',(-53.9883260232292,0.638231104582612,
175.612355141042));
#14280=CARTESIAN_POINT('Ctrl Pts',(-53.9999691294144,0.700880455299337,
175.608701054484));
#14281=CARTESIAN_POINT('Ctrl Pts',(-54.0089495991491,0.747450278919698,
175.608701054484));
#14282=CARTESIAN_POINT('Ctrl Pts',(-54.6838989306507,-3.31503673670408,
177.498541333932));
#14283=CARTESIAN_POINT('Ctrl Pts',(-54.6028424023999,-3.27996788481022,
177.575886787893));
#14284=CARTESIAN_POINT('Ctrl Pts',(-54.4914110693857,-3.22098078368462,
177.675570519779));
#14285=CARTESIAN_POINT('Ctrl Pts',(-54.2877210999876,-3.08712607630556,
177.818300896045));
#14286=CARTESIAN_POINT('Ctrl Pts',(-54.1818936931668,-3.00508764525988,
177.876355950698));
#14287=CARTESIAN_POINT('Ctrl Pts',(-53.8725219138475,-2.7210392223557,177.987971690067));
#14288=CARTESIAN_POINT('Ctrl Pts',(-53.6887412313577,-2.48667656726087,
177.968455801636));
#14289=CARTESIAN_POINT('Ctrl Pts',(-53.4323004468874,-2.07984229374549,
177.81326130021));
#14290=CARTESIAN_POINT('Ctrl Pts',(-53.3481219952623,-1.90209667633303,
177.689106472861));
#14291=CARTESIAN_POINT('Ctrl Pts',(-53.2541428822785,-1.67455559658963,
177.4588693226));
#14292=CARTESIAN_POINT('Ctrl Pts',(-53.2289619472537,-1.60981735363885,
177.366895011932));
#14293=CARTESIAN_POINT('Ctrl Pts',(-53.1902474393619,-1.46398366211967,
177.206162349181));
#14294=CARTESIAN_POINT('Ctrl Pts',(-53.1751071583752,-1.38127728148465,
177.138895465296));
#14295=CARTESIAN_POINT('Ctrl Pts',(-53.1106916579129,-0.946264358659819,
176.818176320833));
#14296=CARTESIAN_POINT('Ctrl Pts',(-53.104040472165,-0.586806104143147,
176.529935688984));
#14297=CARTESIAN_POINT('Ctrl Pts',(-53.1360974496729,-0.0396857905259603,
176.18029692801));
#14298=CARTESIAN_POINT('Ctrl Pts',(-53.1539634359283,0.143713174827862,
176.077481741979));
#14299=CARTESIAN_POINT('Ctrl Pts',(-53.1901198165385,0.421365632644519,
175.964075583891));
#14300=CARTESIAN_POINT('Ctrl Pts',(-53.2037511434212,0.514406029639107,
175.933123019776));
#14301=CARTESIAN_POINT('Ctrl Pts',(-53.2265274914624,0.654852701335273,
175.900501296871));
#14302=CARTESIAN_POINT('Ctrl Pts',(-53.2345054765832,0.701823829844612,
175.891981010963));
#14303=CARTESIAN_POINT('Ctrl Pts',(-53.2512112157347,0.795937950861637,
175.880369228233));
#14304=CARTESIAN_POINT('Ctrl Pts',(-53.2607961579869,0.847523962298047,
175.877281071202));
#14305=CARTESIAN_POINT('Ctrl Pts',(-53.2690139146546,0.890138601607118,
175.877281071202));
#14306=CARTESIAN_POINT('Ctrl Pts',(-55.2712257966423,-2.92704897744562,
177.878689530232));
#14307=CARTESIAN_POINT('Ctrl Pts',(-55.1795805056396,-2.8912491158103,177.971648479319));
#14308=CARTESIAN_POINT('Ctrl Pts',(-55.071651152347,-2.83668212211097,178.070193007683));
#14309=CARTESIAN_POINT('Ctrl Pts',(-54.8569400290031,-2.70264055506668,
178.228485751573));
#14310=CARTESIAN_POINT('Ctrl Pts',(-54.7442267707714,-2.61896876919161,
178.294464842316));
#14311=CARTESIAN_POINT('Ctrl Pts',(-54.411748914535,-2.3258137742146,178.427876644564));
#14312=CARTESIAN_POINT('Ctrl Pts',(-54.2109314776027,-2.08050919081039,
178.41894500554));
#14313=CARTESIAN_POINT('Ctrl Pts',(-53.916627481037,-1.65530705786393,178.288437335003));
#14314=CARTESIAN_POINT('Ctrl Pts',(-53.8113259310995,-1.4695055565481,178.179668212693));
#14315=CARTESIAN_POINT('Ctrl Pts',(-53.6565509821185,-1.22645456083248,
177.985992749455));
#14316=CARTESIAN_POINT('Ctrl Pts',(-53.5992456338471,-1.15500697284035,
177.911446451852));
#14317=CARTESIAN_POINT('Ctrl Pts',(-53.5205982187275,-1.00038039933938,
177.768691630978));
#14318=CARTESIAN_POINT('Ctrl Pts',(-53.5001949060925,-0.916031133997679,
177.702690600146));
#14319=CARTESIAN_POINT('Ctrl Pts',(-53.4364656307362,-0.484980831999149,
177.384837094664));
#14320=CARTESIAN_POINT('Ctrl Pts',(-53.4331177176434,-0.146450840323217,
177.115527564913));
#14321=CARTESIAN_POINT('Ctrl Pts',(-53.4601106410404,0.310277311160734,
176.823586813476));
#14322=CARTESIAN_POINT('Ctrl Pts',(-53.4746528198466,0.453025461810439,
176.745756503099));
#14323=CARTESIAN_POINT('Ctrl Pts',(-53.4980924658573,0.632143583764391,
176.672596723823));
#14324=CARTESIAN_POINT('Ctrl Pts',(-53.5061322713752,0.685795118500917,
176.65543415297));
#14325=CARTESIAN_POINT('Ctrl Pts',(-53.5171472957729,0.75347529696516,176.639723297454));
#14326=CARTESIAN_POINT('Ctrl Pts',(-53.5206705979738,0.773898670072877,
176.636153692475));
#14327=CARTESIAN_POINT('Ctrl Pts',(-53.5271670842632,0.810072302139046,
176.631719187135));
#14328=CARTESIAN_POINT('Ctrl Pts',(-53.5277551938249,0.813458126550056,
176.630849100393));
#14329=CARTESIAN_POINT('Ctrl Pts',(-53.532735212286,0.839282898328416,176.630849100393));
#14330=CARTESIAN_POINT('Ctrl Pts',(-55.1161897096451,-2.27071607222657,
177.448351373365));
#14331=CARTESIAN_POINT('Ctrl Pts',(-55.0544324803005,-2.24407445661358,
177.516574922684));
#14332=CARTESIAN_POINT('Ctrl Pts',(-55.0031840696463,-2.2159075942787,177.564829510218));
#14333=CARTESIAN_POINT('Ctrl Pts',(-54.8981614763103,-2.14735807337978,
177.649345866972));
#14334=CARTESIAN_POINT('Ctrl Pts',(-54.848196955649,-2.10845499517373,177.68122338125));
#14335=CARTESIAN_POINT('Ctrl Pts',(-54.7062455015458,-1.97869616397794,
177.747598981208));
#14336=CARTESIAN_POINT('Ctrl Pts',(-54.6230552819493,-1.87505607340526,
177.751980177594));
#14337=CARTESIAN_POINT('Ctrl Pts',(-54.4781164600507,-1.64599936204779,
177.704020550018));
#14338=CARTESIAN_POINT('Ctrl Pts',(-54.4161687409529,-1.52036398038793,
177.652507519121));
#14339=CARTESIAN_POINT('Ctrl Pts',(-54.3240884061122,-1.31623292778147,
177.552502738263));
#14340=CARTESIAN_POINT('Ctrl Pts',(-54.2900300114527,-1.2450809441322,177.5168693343));
#14341=CARTESIAN_POINT('Ctrl Pts',(-54.2388806708887,-1.10092476185966,
177.429650782512));
#14342=CARTESIAN_POINT('Ctrl Pts',(-54.2230625419579,-1.02814126447079,
177.378422455576));
#14343=CARTESIAN_POINT('Ctrl Pts',(-54.1687570862725,-0.661100958902222,
177.107656526019));
#14344=CARTESIAN_POINT('Ctrl Pts',(-54.1632550913909,-0.344986943697024,
176.855601626641));
#14345=CARTESIAN_POINT('Ctrl Pts',(-54.1894883174704,0.100428951784895,
176.57062132681));
#14346=CARTESIAN_POINT('Ctrl Pts',(-54.2038650968969,0.243821813285216,
176.491645489995));
#14347=CARTESIAN_POINT('Ctrl Pts',(-54.2289503028814,0.435912884592043,
176.413053638658));
#14348=CARTESIAN_POINT('Ctrl Pts',(-54.2378694870404,0.495988408430007,
176.393461416067));
#14349=CARTESIAN_POINT('Ctrl Pts',(-54.2511575637744,0.57777536525398,176.374426535183));
#14350=CARTESIAN_POINT('Ctrl Pts',(-54.2555861991508,0.603644576350343,
176.369782059628));
#14351=CARTESIAN_POINT('Ctrl Pts',(-54.2642818917577,0.652365455860021,
176.363705099944));
#14352=CARTESIAN_POINT('Ctrl Pts',(-54.2669281652524,0.666814619551347,
176.362269083675));
#14353=CARTESIAN_POINT('Ctrl Pts',(-54.2726708967805,0.696594575640996,
176.362269083675));
#14354=CARTESIAN_POINT('Origin',(-54.8225262766493,-2.4647099518558,177.258277275215));
#14355=CARTESIAN_POINT('Ctrl Pts',(-50.193114320713,-27.8005016688432,177.448440461337));
#14356=CARTESIAN_POINT('Ctrl Pts',(-50.1356777281885,-27.7780416249781,
177.514251363723));
#14357=CARTESIAN_POINT('Ctrl Pts',(-50.0768656935625,-27.751543311514,177.569181845458));
#14358=CARTESIAN_POINT('Ctrl Pts',(-49.9502510673185,-27.7006718917524,
177.678131488152));
#14359=CARTESIAN_POINT('Ctrl Pts',(-49.8836384545372,-27.6746069642733,
177.728584647058));
#14360=CARTESIAN_POINT('Ctrl Pts',(-49.6751767137455,-27.5945945456976,
177.866776279515));
#14361=CARTESIAN_POINT('Ctrl Pts',(-49.5241175159801,-27.5384622401806,
177.941191651987));
#14362=CARTESIAN_POINT('Ctrl Pts',(-49.052722448706,-27.3677108924734,178.102046365205));
#14363=CARTESIAN_POINT('Ctrl Pts',(-48.713006227557,-27.2491092781452,178.126053652285));
#14364=CARTESIAN_POINT('Ctrl Pts',(-47.7382795874562,-26.9019657740439,
177.942209528285));
#14365=CARTESIAN_POINT('Ctrl Pts',(-47.1597470877608,-26.6842880122364,
177.461567693823));
#14366=CARTESIAN_POINT('Ctrl Pts',(-46.658904710499,-26.3725604903201,176.179580952166));
#14367=CARTESIAN_POINT('Ctrl Pts',(-46.744016732095,-26.2835354545934,175.410971277798));
#14368=CARTESIAN_POINT('Ctrl Pts',(-47.5354179070377,-26.2224078706935,
174.242909311213));
#14369=CARTESIAN_POINT('Ctrl Pts',(-48.2245449656354,-26.2493771368743,
173.87343933243));
#14370=CARTESIAN_POINT('Ctrl Pts',(-49.6317089464608,-26.3060463238627,
173.871895146128));
#14371=CARTESIAN_POINT('Ctrl Pts',(-50.3230600395606,-26.332977077053,174.238655026377));
#14372=CARTESIAN_POINT('Ctrl Pts',(-51.1153496063116,-26.2743348509258,
175.387691644257));
#14373=CARTESIAN_POINT('Ctrl Pts',(-51.2096393582444,-26.1855070701005,
176.164686974611));
#14374=CARTESIAN_POINT('Ctrl Pts',(-50.7213268039385,-25.8775623946772,
177.442968877094));
#14375=CARTESIAN_POINT('Ctrl Pts',(-50.1473617008829,-25.6602454668112,
177.932812658479));
#14376=CARTESIAN_POINT('Ctrl Pts',(-48.8451246534299,-25.1962898596545,
178.190564242377));
#14377=CARTESIAN_POINT('Ctrl Pts',(-48.1356293396501,-24.9529458243571,
177.955714348281));
#14378=CARTESIAN_POINT('Ctrl Pts',(-47.2268076672755,-24.5631416907191,
176.954286183848));
#14379=CARTESIAN_POINT('Ctrl Pts',(-47.0395646158613,-24.4209960169422,
176.20954077848));
#14380=CARTESIAN_POINT('Ctrl Pts',(-47.370313215787,-24.2726666068476,174.855768290097));
#14381=CARTESIAN_POINT('Ctrl Pts',(-47.8845545017147,-24.265674947158,174.26583855031));
#14382=CARTESIAN_POINT('Ctrl Pts',(-49.1994460468846,-24.3046603227726,
173.764180115318));
#14383=CARTESIAN_POINT('Ctrl Pts',(-49.9762257647407,-24.3480555327739,
173.861039734223));
#14384=CARTESIAN_POINT('Ctrl Pts',(-51.1285193941288,-24.3574791486806,
174.66646218052));
#14385=CARTESIAN_POINT('Ctrl Pts',(-51.4882290443068,-24.3203491702665,
175.364132112564));
#14386=CARTESIAN_POINT('Ctrl Pts',(-51.4777341832408,-24.1036300286494,
176.755680066459));
#14387=CARTESIAN_POINT('Ctrl Pts',(-51.1141102527119,-23.9275319100486,
177.423612084264));
#14388=CARTESIAN_POINT('Ctrl Pts',(-49.9940329966114,-23.4994535030053,
178.148719290634));
#14389=CARTESIAN_POINT('Ctrl Pts',(-49.2531996565364,-23.2503850964097,
178.195074921104));
#14390=CARTESIAN_POINT('Ctrl Pts',(-48.0540724826088,-22.804580182732,177.607487959387));
#14391=CARTESIAN_POINT('Ctrl Pts',(-47.6174629086983,-22.6140260251447,
176.985139741962));
#14392=CARTESIAN_POINT('Ctrl Pts',(-47.4549919432363,-22.3698803060775,
175.609945370482));
#14393=CARTESIAN_POINT('Ctrl Pts',(-47.7329522193418,-22.3169255939418,
174.876470615888));
#14394=CARTESIAN_POINT('Ctrl Pts',(-48.8440385240951,-22.3059754149369,
173.902867041218));
#14395=CARTESIAN_POINT('Ctrl Pts',(-49.7035599970344,-22.3554674780819,
173.739637329099));
#14396=CARTESIAN_POINT('Ctrl Pts',(-51.1531706356154,-22.4011313967338,
174.265066374312));
#14397=CARTESIAN_POINT('Ctrl Pts',(-51.7115054154064,-22.3910761212842,
174.945624054023));
#14398=CARTESIAN_POINT('Ctrl Pts',(-51.9563259347572,-22.2045289991918,
176.459132103654));
#14399=CARTESIAN_POINT('Ctrl Pts',(-51.63765119649,-22.0251559400258,177.262331468575));
#14400=CARTESIAN_POINT('Ctrl Pts',(-50.4571461815608,-21.5627984935069,
178.149907937338));
#14401=CARTESIAN_POINT('Ctrl Pts',(-49.6222512854117,-21.2849471395443,
178.217719280236));
#14402=CARTESIAN_POINT('Ctrl Pts',(-48.3256452005116,-20.7988977065915,
177.525255091295));
#14403=CARTESIAN_POINT('Ctrl Pts',(-47.8935170509031,-20.5993012814682,
176.78942555283));
#14404=CARTESIAN_POINT('Ctrl Pts',(-47.9069259765589,-20.3679964193449,
175.264267840625));
#14405=CARTESIAN_POINT('Ctrl Pts',(-48.3565963500671,-20.33698501403,174.508050023486));
#14406=CARTESIAN_POINT('Ctrl Pts',(-49.7115395236169,-20.3645147337819,
173.767258025586));
#14407=CARTESIAN_POINT('Ctrl Pts',(-50.5919963646361,-20.4163759449694,
173.798730113887));
#14408=CARTESIAN_POINT('Ctrl Pts',(-51.8921615926268,-20.4324111199544,
174.637786957993));
#14409=CARTESIAN_POINT('Ctrl Pts',(-52.2870845316673,-20.391715494119,175.425932171935));
#14410=CARTESIAN_POINT('Ctrl Pts',(-52.1845249551972,-20.1359343420921,
176.949348485014));
#14411=CARTESIAN_POINT('Ctrl Pts',(-51.6978717551623,-19.9258306519252,
177.647217385389));
#14412=CARTESIAN_POINT('Ctrl Pts',(-50.3567743114224,-19.4332812849397,
178.229888643815));
#14413=CARTESIAN_POINT('Ctrl Pts',(-49.531482093434,-19.1564117811874,178.098575810452));
#14414=CARTESIAN_POINT('Ctrl Pts',(-48.4209526978951,-18.7085233315365,
177.123331466978));
#14415=CARTESIAN_POINT('Ctrl Pts',(-48.1597795720535,-18.5402167412103,
176.29718764283));
#14416=CARTESIAN_POINT('Ctrl Pts',(-48.5145782694716,-18.3739619700934,
174.800216258582));
#14417=CARTESIAN_POINT('Ctrl Pts',(-49.1216168980297,-18.3741927637648,
174.159897255644));
#14418=CARTESIAN_POINT('Ctrl Pts',(-50.6124880467131,-18.4256628314289,
173.74530968569));
#14419=CARTESIAN_POINT('Ctrl Pts',(-51.4570089590119,-18.472296203581,173.973986288395));
#14420=CARTESIAN_POINT('Ctrl Pts',(-52.5367755134872,-18.4465314340497,
175.076321400051));
#14421=CARTESIAN_POINT('Ctrl Pts',(-52.7461464663159,-18.3691716102472,
175.928004990245));
#14422=CARTESIAN_POINT('Ctrl Pts',(-52.3166330239091,-18.0526500335514,
177.376965544067));
#14423=CARTESIAN_POINT('Ctrl Pts',(-51.6857211698905,-17.8130496454,177.945754508989));
#14424=CARTESIAN_POINT('Ctrl Pts',(-50.2465394893753,-17.3007990625156,
178.194297846636));
#14425=CARTESIAN_POINT('Ctrl Pts',(-49.4703000985441,-17.0343670318334,
177.871754882023));
#14426=CARTESIAN_POINT('Ctrl Pts',(-48.6088763818932,-16.6321365971318,
176.648991214725));
#14427=CARTESIAN_POINT('Ctrl Pts',(-48.5409020769561,-16.5028432711256,
175.78526591443));
#14428=CARTESIAN_POINT('Ctrl Pts',(-49.2164515058916,-16.3991203888251,
174.401518908745));
#14429=CARTESIAN_POINT('Ctrl Pts',(-49.9496118192587,-16.4227354715302,
173.914202886417));
#14430=CARTESIAN_POINT('Ctrl Pts',(-51.4902606534728,-16.4861638259448,
173.836744887307));
#14431=CARTESIAN_POINT('Ctrl Pts',(-52.2697075969923,-16.5185243960147,
174.249627738192));
#14432=CARTESIAN_POINT('Ctrl Pts',(-53.0792623986938,-16.4399376212412,
175.566241461313));
#14433=CARTESIAN_POINT('Ctrl Pts',(-53.0958608617722,-16.3264383488088,
176.440260240546));
#14434=CARTESIAN_POINT('Ctrl Pts',(-52.3498924896565,-15.9464100326616,
177.743856795072));
#14435=CARTESIAN_POINT('Ctrl Pts',(-51.6136771994172,-15.6882407493956,
178.142477224647));
#14436=CARTESIAN_POINT('Ctrl Pts',(-50.1619939854693,-15.1743526813971,
178.045393567771));
#14437=CARTESIAN_POINT('Ctrl Pts',(-49.479535393056,-14.9249532161513,177.547481856475));
#14438=CARTESIAN_POINT('Ctrl Pts',(-48.9083003859244,-14.5811172796918,
176.154888290848));
#14439=CARTESIAN_POINT('Ctrl Pts',(-49.032687325759,-14.4872017268269,175.286386043965));
#14440=CARTESIAN_POINT('Ctrl Pts',(-50.002899927607,-14.4395306566209,174.08106638639));
#14441=CARTESIAN_POINT('Ctrl Pts',(-50.8258619899905,-14.4815667576624,
173.768688449528));
#14442=CARTESIAN_POINT('Ctrl Pts',(-52.3490472247602,-14.5391579602322,
174.044477097964));
#14443=CARTESIAN_POINT('Ctrl Pts',(-53.0108480437211,-14.5505369630929,
174.618897762295));
#14444=CARTESIAN_POINT('Ctrl Pts',(-53.508606726061,-14.41258118913,176.072854784516));
#14445=CARTESIAN_POINT('Ctrl Pts',(-53.3308496256547,-14.2605010523332,
176.92211652172));
#14446=CARTESIAN_POINT('Ctrl Pts',(-52.3234046589676,-13.8325238003689,
178.011250192421));
#14447=CARTESIAN_POINT('Ctrl Pts',(-51.5138129382755,-13.5585438056648,
178.229366209696));
#14448=CARTESIAN_POINT('Ctrl Pts',(-50.1182607249297,-13.0546721198729,
177.788098654291));
#14449=CARTESIAN_POINT('Ctrl Pts',(-49.5630188185408,-12.8308644828691,
177.140857971114));
#14450=CARTESIAN_POINT('Ctrl Pts',(-49.3219040202974,-12.5483689245281,
175.637957478437));
#14451=CARTESIAN_POINT('Ctrl Pts',(-49.6365594730894,-12.4926951709364,
174.821179942866));
#14452=CARTESIAN_POINT('Ctrl Pts',(-50.8450351424658,-12.4918253386163,
173.862170041067));
#14453=CARTESIAN_POINT('Ctrl Pts',(-51.7160671936879,-12.5420406725331,
173.742988789581));
#14454=CARTESIAN_POINT('Ctrl Pts',(-53.1380531234061,-12.5824907099911,
174.344563971126));
#14455=CARTESIAN_POINT('Ctrl Pts',(-53.661497991413,-12.565516429584,175.054752397452));
#14456=CARTESIAN_POINT('Ctrl Pts',(-53.8242077932451,-12.3622912981454,
176.579637740953));
#14457=CARTESIAN_POINT('Ctrl Pts',(-53.4635573374974,-12.1759538811977,
177.362604506387));
#14458=CARTESIAN_POINT('Ctrl Pts',(-52.2358756182636,-11.7031645393402,
178.179207046235));
#14459=CARTESIAN_POINT('Ctrl Pts',(-51.404471480006,-11.4266005921062,178.198059647233));
#14460=CARTESIAN_POINT('Ctrl Pts',(-50.1465877134854,-10.9499764840513,
177.440684540534));
#14461=CARTESIAN_POINT('Ctrl Pts',(-49.7512566691313,-10.7559713173261,
176.677961727673));
#14462=CARTESIAN_POINT('Ctrl Pts',(-49.8442980389787,-10.5402489724976,
175.152069846099));
#14463=CARTESIAN_POINT('Ctrl Pts',(-50.3336227209985,-10.5166703329192,
174.417963751365));
#14464=CARTESIAN_POINT('Ctrl Pts',(-51.729412313951,-10.5511670115394,173.750914008412));
#14465=CARTESIAN_POINT('Ctrl Pts',(-52.6055357660183,-10.6034581645062,
173.829125569603));
#14466=CARTESIAN_POINT('Ctrl Pts',(-53.8591972775733,-10.6090268187652,
174.739479897504));
#14467=CARTESIAN_POINT('Ctrl Pts',(-54.2075655427863,-10.559958422732,175.542285446703));
#14468=CARTESIAN_POINT('Ctrl Pts',(-54.0309723767407,-10.2919570312328,
177.05153449857));
#14469=CARTESIAN_POINT('Ctrl Pts',(-53.5065211660476,-10.0729835636969,
177.724885949439));
#14470=CARTESIAN_POINT('Ctrl Pts',(-52.1359327706082,-9.57501150980407,
178.231990439602));
#14471=CARTESIAN_POINT('Ctrl Pts',(-51.3168725161042,-9.29919601638729,
178.055337178134));
#14472=CARTESIAN_POINT('Ctrl Pts',(-50.258716477129,-8.86039345968628,177.014257444883));
#14473=CARTESIAN_POINT('Ctrl Pts',(-50.0419858596938,-8.70190296068798,
176.174822144773));
#14474=CARTESIAN_POINT('Ctrl Pts',(-50.4788136762356,-8.55014763089762,
174.697436550109));
#14475=CARTESIAN_POINT('Ctrl Pts',(-51.1165600370436,-8.55674976323144,
174.095019459488));
#14476=CARTESIAN_POINT('Ctrl Pts',(-52.6206590619166,-8.6128620697194,173.755704628284));
#14477=CARTESIAN_POINT('Ctrl Pts',(-53.456626592603,-8.65630954771657,174.029197443714));
#14478=CARTESIAN_POINT('Ctrl Pts',(-54.4781193003427,-8.6195332279715,175.187078119489));
#14479=CARTESIAN_POINT('Ctrl Pts',(-54.643602443466,-8.53353572012608,176.04949882023));
#14480=CARTESIAN_POINT('Ctrl Pts',(-54.1354947853707,-8.20096498746117,
177.472181687833));
#14481=CARTESIAN_POINT('Ctrl Pts',(-53.4760203027823,-7.95706608118669,
178.003825172765));
#14482=CARTESIAN_POINT('Ctrl Pts',(-52.0249165538012,-7.441132564782,178.167825277993));
#14483=CARTESIAN_POINT('Ctrl Pts',(-51.2723007652614,-7.17976116760829,
177.802466009854));
#14484=CARTESIAN_POINT('Ctrl Pts',(-50.4742318046734,-6.79179686888332,
176.539214575509));
#14485=CARTESIAN_POINT('Ctrl Pts',(-50.4508393849021,-6.66952799804251,
175.667365550039));
#14486=CARTESIAN_POINT('Ctrl Pts',(-51.1982775200671,-6.57992894303025,
174.318931761547));
#14487=CARTESIAN_POINT('Ctrl Pts',(-51.9567203354133,-6.60831910752051,
173.869388776842));
#14488=CARTESIAN_POINT('Ctrl Pts',(-53.5030461170827,-6.67180659392302,
173.876188814802));
#14489=CARTESIAN_POINT('Ctrl Pts',(-54.2579318048227,-6.70074853854407,
174.329266762268));
#14490=CARTESIAN_POINT('Ctrl Pts',(-54.9950541895712,-6.6067812144727,175.688231083653));
#14491=CARTESIAN_POINT('Ctrl Pts',(-54.9633937640365,-6.48434226598442,
176.556150922255));
#14492=CARTESIAN_POINT('Ctrl Pts',(-54.1573516980127,-6.0949735677162,177.812809342709));
#14493=CARTESIAN_POINT('Ctrl Pts',(-53.3979887985791,-5.83073710308303,
178.172806822259));
#14494=CARTESIAN_POINT('Ctrl Pts',(-51.9519097716579,-5.31810666795101,
177.994568269632));
#14495=CARTESIAN_POINT('Ctrl Pts',(-51.2952074816856,-5.0735953089356,177.458800517348));
#14496=CARTESIAN_POINT('Ctrl Pts',(-50.7993635736617,-4.74342220821161,
176.031468409862));
#14497=CARTESIAN_POINT('Ctrl Pts',(-50.9692613848378,-4.65940397939939,
175.170313217647));
#14498=CARTESIAN_POINT('Ctrl Pts',(-52.0040245669764,-4.62293999106357,
174.01934301833));
#14499=CARTESIAN_POINT('Ctrl Pts',(-52.8385688131003,-4.66759138415716,
173.754231358386));
#14500=CARTESIAN_POINT('Ctrl Pts',(-54.3414847379305,-4.72329909029368,
174.103969484305));
#14501=CARTESIAN_POINT('Ctrl Pts',(-54.9761466933045,-4.72791014175074,
174.714716972292));
#14502=CARTESIAN_POINT('Ctrl Pts',(-55.3975165431988,-4.57549651155636,
176.192173272167));
#14503=CARTESIAN_POINT('Ctrl Pts',(-55.1760506072609,-4.4148786220368,177.03103539143));
#14504=CARTESIAN_POINT('Ctrl Pts',(-54.1093043232961,-3.97451188101218,
178.061753391873));
#14505=CARTESIAN_POINT('Ctrl Pts',(-53.2902925544343,-3.69995792969149,
178.233822626392));
#14506=CARTESIAN_POINT('Ctrl Pts',(-51.9203920380846,-3.19963469730891,
177.711493690972));
#14507=CARTESIAN_POINT('Ctrl Pts',(-51.4044324721558,-2.98383265912278,
177.036002564632));
#14508=CARTESIAN_POINT('Ctrl Pts',(-51.237949425703,-2.71774512370317,175.525044339462));
#14509=CARTESIAN_POINT('Ctrl Pts',(-51.5957499271559,-2.66894330374766,
174.721509320474));
#14510=CARTESIAN_POINT('Ctrl Pts',(-52.8541051305037,-2.67783999801612,
173.825937213487));
#14511=CARTESIAN_POINT('Ctrl Pts',(-53.7315999697276,-2.7292086653859,173.7525048498));
#14512=CARTESIAN_POINT('Ctrl Pts',(-55.1208667949195,-2.76252327401043,
174.431246184642));
#14513=CARTESIAN_POINT('Ctrl Pts',(-55.6054709668258,-2.73893798071373,
175.167402226862));
#14514=CARTESIAN_POINT('Ctrl Pts',(-55.6603171863937,-2.58869274068622,
176.211840888345));
#14515=CARTESIAN_POINT('Ctrl Pts',(-55.6210463302226,-2.5392081864434,176.490448482462));
#14516=CARTESIAN_POINT('Ctrl Pts',(-55.4836397365907,-2.4479441182576,176.880586390838));
#14517=CARTESIAN_POINT('Ctrl Pts',(-55.4253285390117,-2.41535251334816,
177.005027857449));
#14518=CARTESIAN_POINT('Ctrl Pts',(-55.321414213033,-2.36345060131236,177.180440236558));
#14519=CARTESIAN_POINT('Ctrl Pts',(-55.2840225057543,-2.34563722905757,
177.23703696138));
#14520=CARTESIAN_POINT('Ctrl Pts',(-55.2039936793606,-2.30896761153951,
177.345998347345));
#14521=CARTESIAN_POINT('Ctrl Pts',(-55.1587206712145,-2.28906361698866,
177.401367187303));
#14522=CARTESIAN_POINT('Ctrl Pts',(-55.1161897096451,-2.27071607222657,
177.448351373365));
#14523=CARTESIAN_POINT('Ctrl Pts',(-50.0383214665825,-27.1440081492037,
177.018259765604));
#14524=CARTESIAN_POINT('Ctrl Pts',(-49.9984978891038,-27.1200869921306,
177.079962725598));
#14525=CARTESIAN_POINT('Ctrl Pts',(-49.9575055461974,-27.1020674615118,
177.117111982701));
#14526=CARTESIAN_POINT('Ctrl Pts',(-49.8677888002033,-27.0582153119246,
177.208150208202));
#14527=CARTESIAN_POINT('Ctrl Pts',(-49.8200811333233,-27.0356913176731,
177.250904604008));
#14528=CARTESIAN_POINT('Ctrl Pts',(-49.6696339972988,-26.9667169890279,
177.369319858048));
#14529=CARTESIAN_POINT('Ctrl Pts',(-49.5596041625372,-26.9190141211719,
177.434440092329));
#14530=CARTESIAN_POINT('Ctrl Pts',(-49.2118492777513,-26.7720570333375,
177.585359994682));
#14531=CARTESIAN_POINT('Ctrl Pts',(-48.9561313182544,-26.6696252716912,
177.624018992736));
#14532=CARTESIAN_POINT('Ctrl Pts',(-48.2061347626312,-26.3651189875991,
177.541325063495));
#14533=CARTESIAN_POINT('Ctrl Pts',(-47.7414452899411,-26.1688071749961,
177.206816180124));
#14534=CARTESIAN_POINT('Ctrl Pts',(-47.2997616792461,-25.8707230428421,
176.259912393579));
#14535=CARTESIAN_POINT('Ctrl Pts',(-47.3254088075791,-25.7696878441865,
175.668385446485));
#14536=CARTESIAN_POINT('Ctrl Pts',(-47.8755348089008,-25.6608852645148,
174.730075629747));
#14537=CARTESIAN_POINT('Ctrl Pts',(-48.3883745667453,-25.6533154874374,
174.409130171609));
#14538=CARTESIAN_POINT('Ctrl Pts',(-49.4697935970405,-25.6493947609597,
174.331547147859));
#14539=CARTESIAN_POINT('Ctrl Pts',(-50.0242338430418,-25.649381701477,174.571983854445));
#14540=CARTESIAN_POINT('Ctrl Pts',(-50.7048786270563,-25.5680766842178,
175.408205503607));
#14541=CARTESIAN_POINT('Ctrl Pts',(-50.8241348799264,-25.4835527568238,
175.999504945815));
#14542=CARTESIAN_POINT('Ctrl Pts',(-50.5299373615978,-25.2151761375736,
177.003363164347));
#14543=CARTESIAN_POINT('Ctrl Pts',(-50.1239438073276,-25.0297634587285,
177.413176265946));
#14544=CARTESIAN_POINT('Ctrl Pts',(-49.1505246752548,-24.6280758402134,
177.688626402201));
#14545=CARTESIAN_POINT('Ctrl Pts',(-48.5986534337901,-24.4145815428545,
177.549736774231));
#14546=CARTESIAN_POINT('Ctrl Pts',(-47.8611459428243,-24.0600384609719,
176.839550282587));
#14547=CARTESIAN_POINT('Ctrl Pts',(-47.6799485846058,-23.9185188665616,
176.282427966132));
#14548=CARTESIAN_POINT('Ctrl Pts',(-47.8667875018081,-23.7413010936383,
175.228664295839));
#14549=CARTESIAN_POINT('Ctrl Pts',(-48.2335406641398,-23.7053609783786,
174.748651320702));
#14550=CARTESIAN_POINT('Ctrl Pts',(-49.2178139490401,-23.6827183215843,
174.294936194443));
#14551=CARTESIAN_POINT('Ctrl Pts',(-49.8219962257384,-23.6923479099038,
174.323992647469));
#14552=CARTESIAN_POINT('Ctrl Pts',(-50.7591498572879,-23.6591435932359,
174.876124371948));
#14553=CARTESIAN_POINT('Ctrl Pts',(-51.077522753783,-23.6134950148359,175.39172485521));
#14554=CARTESIAN_POINT('Ctrl Pts',(-51.1535820381579,-23.415693423287,176.455061557909));
#14555=CARTESIAN_POINT('Ctrl Pts',(-50.918643706726,-23.2638702537623,176.988610346676));
#14556=CARTESIAN_POINT('Ctrl Pts',(-50.1109113395739,-22.8948872174005,
177.611393006538));
#14557=CARTESIAN_POINT('Ctrl Pts',(-49.550353441179,-22.680074585543,177.689808241912));
#14558=CARTESIAN_POINT('Ctrl Pts',(-48.6137447048011,-22.28702457331,177.311258226648));
#14559=CARTESIAN_POINT('Ctrl Pts',(-48.2490117887893,-22.1098470443037,
176.862573175931));
#14560=CARTESIAN_POINT('Ctrl Pts',(-48.0569364843034,-21.8588516971627,
175.821098220226));
#14561=CARTESIAN_POINT('Ctrl Pts',(-48.2348449020816,-21.7860567828884,
175.244332219005));
#14562=CARTESIAN_POINT('Ctrl Pts',(-49.0386897150743,-21.7181941257994,
174.442583421401));
#14563=CARTESIAN_POINT('Ctrl Pts',(-49.6927278496366,-21.7268807239962,
174.267611662058));
#14564=CARTESIAN_POINT('Ctrl Pts',(-50.8411043798997,-21.7141199241716,
174.588524908528));
#14565=CARTESIAN_POINT('Ctrl Pts',(-51.3094013702521,-21.6876269507243,
175.077312328235));
#14566=CARTESIAN_POINT('Ctrl Pts',(-51.5921855585383,-21.5071481278118,
176.224756535618));
#14567=CARTESIAN_POINT('Ctrl Pts',(-51.3974806497779,-21.3525654190584,
176.857134695111));
#14568=CARTESIAN_POINT('Ctrl Pts',(-50.5541169969121,-20.9549536496367,
177.606432421015));
#14569=CARTESIAN_POINT('Ctrl Pts',(-49.9226700094089,-20.7151144402318,
177.707627413831));
#14570=CARTESIAN_POINT('Ctrl Pts',(-48.9071810235129,-20.2857229365746,
177.254800594979));
#14571=CARTESIAN_POINT('Ctrl Pts',(-48.539258060867,-20.0973264562627,176.718436772752));
#14572=CARTESIAN_POINT('Ctrl Pts',(-48.475069365768,-19.8507243142978,175.553477519371));
#14573=CARTESIAN_POINT('Ctrl Pts',(-48.7817617425817,-19.793065331538,174.952184411851));
#14574=CARTESIAN_POINT('Ctrl Pts',(-49.7883433018784,-19.7521647995451,
174.308551222089));
#14575=CARTESIAN_POINT('Ctrl Pts',(-50.4672686416896,-19.7660480884512,
174.284275257332));
#14576=CARTESIAN_POINT('Ctrl Pts',(-51.5185621567429,-19.7338211938064,
174.853733695028));
#14577=CARTESIAN_POINT('Ctrl Pts',(-51.8704305933054,-19.6836035315617,
175.436932234299));
#14578=CARTESIAN_POINT('Ctrl Pts',(-51.8843323266907,-19.4527281797322,
176.606134032902));
#14579=CARTESIAN_POINT('Ctrl Pts',(-51.5571193795133,-19.2721887380014,
177.170821269618));
#14580=CARTESIAN_POINT('Ctrl Pts',(-50.5738822832083,-18.8483164964054,
177.696322750616));
#14581=CARTESIAN_POINT('Ctrl Pts',(-49.9420101663495,-18.6096692642048,
177.644259926591));
#14582=CARTESIAN_POINT('Ctrl Pts',(-49.0472024681392,-18.2021277928874,
176.964465534643));
#14583=CARTESIAN_POINT('Ctrl Pts',(-48.8080140865945,-18.0389468515475,
176.349664596734));
#14584=CARTESIAN_POINT('Ctrl Pts',(-49.0066488397389,-17.8423059144124,
175.186793179499));
#14585=CARTESIAN_POINT('Ctrl Pts',(-49.4421820059815,-17.8082452535064,
174.661978305101));
#14586=CARTESIAN_POINT('Ctrl Pts',(-50.56604357313,-17.7913894148755,174.265152819574));
#14587=CARTESIAN_POINT('Ctrl Pts',(-51.2311395254822,-17.8022399917982,
174.391161445375));
#14588=CARTESIAN_POINT('Ctrl Pts',(-52.1286453083844,-17.7409968363402,
175.174698745784));
#14589=CARTESIAN_POINT('Ctrl Pts',(-52.340061283037,-17.6649540872478,175.813880719354));
#14590=CARTESIAN_POINT('Ctrl Pts',(-52.1027685307223,-17.384247754716,176.951110854015));
#14591=CARTESIAN_POINT('Ctrl Pts',(-51.6569691297711,-17.1812314095055,
177.42208876923));
#14592=CARTESIAN_POINT('Ctrl Pts',(-50.5803007618318,-16.7386138153048,
177.697510231007));
#14593=CARTESIAN_POINT('Ctrl Pts',(-49.9722430688612,-16.5033958825231,
177.495874655633));
#14594=CARTESIAN_POINT('Ctrl Pts',(-49.2598451033921,-16.1323520825764,
176.614580397518));
#14595=CARTESIAN_POINT('Ctrl Pts',(-49.1633964478354,-15.9963838869222,
175.958557394859));
#14596=CARTESIAN_POINT('Ctrl Pts',(-49.6135825845651,-15.8488720097956,
174.863627023648));
#14597=CARTESIAN_POINT('Ctrl Pts',(-50.1513088289339,-15.8357216637453,
174.451396860398));
#14598=CARTESIAN_POINT('Ctrl Pts',(-51.3373123393945,-15.8295083514664,
174.304991255183));
#14599=CARTESIAN_POINT('Ctrl Pts',(-51.9598057434752,-15.8324905082382,
174.577589691682));
#14600=CARTESIAN_POINT('Ctrl Pts',(-52.662356604517,-15.7329936013494,175.540542955831));
#14601=CARTESIAN_POINT('Ctrl Pts',(-52.7287365437827,-15.6278770852026,
176.211335092655));
#14602=CARTESIAN_POINT('Ctrl Pts',(-52.2404503570114,-15.2999892249187,
177.248966419092));
#14603=CARTESIAN_POINT('Ctrl Pts',(-51.7049290320028,-15.079336195701,177.599407337456));
#14604=CARTESIAN_POINT('Ctrl Pts',(-50.599341197491,-14.6318604318474,177.611289749054));
#14605=CARTESIAN_POINT('Ctrl Pts',(-50.0563698831837,-14.4102803084529,
177.271399907022));
#14606=CARTESIAN_POINT('Ctrl Pts',(-49.5511866458666,-14.0779293284932,
176.24060069501));
#14607=CARTESIAN_POINT('Ctrl Pts',(-49.604058679892,-13.971112568136,175.571774049481));
#14608=CARTESIAN_POINT('Ctrl Pts',(-50.2895824050587,-13.8682646399117,
174.596554366676));
#14609=CARTESIAN_POINT('Ctrl Pts',(-50.9089033822508,-13.8698152300494,
174.310925422501));
#14610=CARTESIAN_POINT('Ctrl Pts',(-52.0945937584551,-13.8647732522077,
174.438441317441));
#14611=CARTESIAN_POINT('Ctrl Pts',(-52.6396705452532,-13.8524570813917,
174.840092836798));
#14612=CARTESIAN_POINT('Ctrl Pts',(-53.1114861845869,-13.7091720746061,
175.926135983292));
#14613=CARTESIAN_POINT('Ctrl Pts',(-53.0273981908184,-13.5760746720968,
176.585468457757));
#14614=CARTESIAN_POINT('Ctrl Pts',(-52.3273047331872,-13.2061141571923,
177.480731662196));
#14615=CARTESIAN_POINT('Ctrl Pts',(-51.7260689896615,-12.9732036309654,
177.694033962224));
#14616=CARTESIAN_POINT('Ctrl Pts',(-50.6444965881338,-12.5296009109336,
177.439340266607));
#14617=CARTESIAN_POINT('Ctrl Pts',(-50.1880101288259,-12.323622761024,176.975929902189));
#14618=CARTESIAN_POINT('Ctrl Pts',(-49.9332603826239,-12.0409453485109,
175.846473225312));
#14619=CARTESIAN_POINT('Ctrl Pts',(-50.1325085529845,-11.9618298866148,
175.20357102314));
#14620=CARTESIAN_POINT('Ctrl Pts',(-51.0139495749547,-11.8975707104174,
174.402850839007));
#14621=CARTESIAN_POINT('Ctrl Pts',(-51.6770380739026,-11.9086053392238,
174.263669429449));
#14622=CARTESIAN_POINT('Ctrl Pts',(-52.8102442474793,-11.89211453585,174.644220443453));
#14623=CARTESIAN_POINT('Ctrl Pts',(-53.2534129688289,-11.860550625243,175.158200214442));
#14624=CARTESIAN_POINT('Ctrl Pts',(-53.4727724514858,-11.667970777174,176.317676214963));
#14625=CARTESIAN_POINT('Ctrl Pts',(-53.2447122957938,-11.5059876351892,
176.940267405791));
#14626=CARTESIAN_POINT('Ctrl Pts',(-52.3630606041574,-11.1023742765951,
177.633671542876));
#14627=CARTESIAN_POINT('Ctrl Pts',(-51.7328063873735,-10.863413150139,177.698996091772));
#14628=CARTESIAN_POINT('Ctrl Pts',(-50.7387975664535,-10.4373493069837,
177.194617067458));
#14629=CARTESIAN_POINT('Ctrl Pts',(-50.4003959556136,-10.2552411513015,
176.636362249629));
#14630=CARTESIAN_POINT('Ctrl Pts',(-50.3964887911414,-10.0195709762704,
175.464836254896));
#14631=CARTESIAN_POINT('Ctrl Pts',(-50.7352645697859,-9.96785241001128,
174.878086269107));
#14632=CARTESIAN_POINT('Ctrl Pts',(-51.7761584941716,-9.93363014738946,
174.290073576044));
#14633=CARTESIAN_POINT('Ctrl Pts',(-52.4578743221659,-9.94721824196466,
174.301034748671));
#14634=CARTESIAN_POINT('Ctrl Pts',(-53.4723487166264,-9.90911175935534,
174.927224952557));
#14635=CARTESIAN_POINT('Ctrl Pts',(-53.7905639694071,-9.85304000489839,
175.522456262626));
#14636=CARTESIAN_POINT('Ctrl Pts',(-53.7495974866252,-9.61086987508902,
176.689642787431));
#14637=CARTESIAN_POINT('Ctrl Pts',(-53.3913473444599,-9.42486391207369,
177.234457154129));
#14638=CARTESIAN_POINT('Ctrl Pts',(-52.3804909291071,-8.9950096827268,177.705080880716));
#14639=CARTESIAN_POINT('Ctrl Pts',(-51.7506169575959,-8.75656955580448,
177.617528508224));
#14640=CARTESIAN_POINT('Ctrl Pts',(-50.8938217209944,-8.35631416012115,
176.884644400558));
#14641=CARTESIAN_POINT('Ctrl Pts',(-50.686386739593,-8.19840449522365,176.254364811283));
#14642=CARTESIAN_POINT('Ctrl Pts',(-50.9496816541175,-8.01563271032117,
175.10646784668));
#14643=CARTESIAN_POINT('Ctrl Pts',(-51.4086597834924,-7.98657238824085,
174.608429324338));
#14644=CARTESIAN_POINT('Ctrl Pts',(-52.5506583028891,-7.97253715897243,
174.264721414109));
#14645=CARTESIAN_POINT('Ctrl Pts',(-53.2085070979977,-7.98255305121696,
174.427141629608));
#14646=CARTESIAN_POINT('Ctrl Pts',(-54.0661826067832,-7.91293346685192,
175.257046778597));
#14647=CARTESIAN_POINT('Ctrl Pts',(-54.2443196068901,-7.83026930904402,
175.907383805075));
#14648=CARTESIAN_POINT('Ctrl Pts',(-53.9449265679421,-7.53766373675317,
177.027297077911));
#14649=CARTESIAN_POINT('Ctrl Pts',(-53.4737144264175,-7.32885697968307,
177.474235384447));
#14650=CARTESIAN_POINT('Ctrl Pts',(-52.3866301268079,-6.88556912331281,
177.682767568372));
#14651=CARTESIAN_POINT('Ctrl Pts',(-51.7946034524202,-6.6539762900198,177.44919290535));
#14652=CARTESIAN_POINT('Ctrl Pts',(-51.1242376556131,-6.29031677842802,
176.53135144958));
#14653=CARTESIAN_POINT('Ctrl Pts',(-51.0636455015902,-6.16179111781231,
175.868699032101));
#14654=CARTESIAN_POINT('Ctrl Pts',(-51.5708785507503,-6.02461835391231,
174.795021951807));
#14655=CARTESIAN_POINT('Ctrl Pts',(-52.1305414737447,-6.01557067494389,
174.410384417273));
#14656=CARTESIAN_POINT('Ctrl Pts',(-53.3239707675344,-6.01072022664985,
174.329110015938));
#14657=CARTESIAN_POINT('Ctrl Pts',(-53.9334177584311,-6.01040522494539,
174.634606029695));
#14658=CARTESIAN_POINT('Ctrl Pts',(-54.5783977308191,-5.90111793801205,
175.631553651875));
#14659=CARTESIAN_POINT('Ctrl Pts',(-54.6093650217473,-5.78956533803437,
176.299320421659));
#14660=CARTESIAN_POINT('Ctrl Pts',(-54.0728671794864,-5.45185644429227,
177.309544041851));
#14661=CARTESIAN_POINT('Ctrl Pts',(-53.5182109168208,-5.22801082267814,
177.628618080665));
#14662=CARTESIAN_POINT('Ctrl Pts',(-52.4111095558568,-4.77949537513279,
177.578747218087));
#14663=CARTESIAN_POINT('Ctrl Pts',(-51.8857104064777,-4.56119881916171,
177.207895099161));
#14664=CARTESIAN_POINT('Ctrl Pts',(-51.4375681932236,-4.23993965724606,
176.147216345704));
#14665=CARTESIAN_POINT('Ctrl Pts',(-51.5255341013567,-4.13891120462634,
175.478088476179));
#14666=CARTESIAN_POINT('Ctrl Pts',(-52.2621121714531,-4.04739311840896,
174.545543255356));
#14667=CARTESIAN_POINT('Ctrl Pts',(-52.8911810801,-4.05123090724587,174.294043710706));
#14668=CARTESIAN_POINT('Ctrl Pts',(-54.0705541410016,-4.04422766004653,
174.477498952297));
#14669=CARTESIAN_POINT('Ctrl Pts',(-54.593284417315,-4.02816934534973,174.908686002258));
#14670=CARTESIAN_POINT('Ctrl Pts',(-55.0092587601974,-3.87346271742067,
176.018250487428));
#14671=CARTESIAN_POINT('Ctrl Pts',(-54.8907029615328,-3.73358556412494,
176.67236673678));
#14672=CARTESIAN_POINT('Ctrl Pts',(-54.1422797098421,-3.35431610458726,
177.524634651606));
#14673=CARTESIAN_POINT('Ctrl Pts',(-53.5287781394068,-3.11818277146878,
177.704881014433));
#14674=CARTESIAN_POINT('Ctrl Pts',(-52.4666030700143,-2.67965003658039,
177.385814188219));
#14675=CARTESIAN_POINT('Ctrl Pts',(-52.037952109723,-2.47949238143003,176.900644117435));
#14676=CARTESIAN_POINT('Ctrl Pts',(-51.8369606432704,-2.20643344946428,
175.75693673757));
#14677=CARTESIAN_POINT('Ctrl Pts',(-52.0709636415419,-2.13467360272607,
175.124746251973));
#14678=CARTESIAN_POINT('Ctrl Pts',(-52.9948906247979,-2.07782438513344,
174.368185237747));
#14679=CARTESIAN_POINT('Ctrl Pts',(-53.6658603596095,-2.09023021076396,
174.26394539811));
#14680=CARTESIAN_POINT('Ctrl Pts',(-54.7763899734937,-2.0695796979931,174.705748499134));
#14681=CARTESIAN_POINT('Ctrl Pts',(-55.193636646253,-2.03216929631525,175.243747077929));
#14682=CARTESIAN_POINT('Ctrl Pts',(-55.2990804121262,-1.89289436927212,
176.038719570758));
#14683=CARTESIAN_POINT('Ctrl Pts',(-55.2875271080061,-1.8476232285876,176.255654667139));
#14684=CARTESIAN_POINT('Ctrl Pts',(-55.2062064365128,-1.76817883590891,
176.561034862255));
#14685=CARTESIAN_POINT('Ctrl Pts',(-55.1692797902087,-1.73965218400568,
176.660101738528));
#14686=CARTESIAN_POINT('Ctrl Pts',(-55.100781391479,-1.69439363416682,176.801019080259));
#14687=CARTESIAN_POINT('Ctrl Pts',(-55.0757487692566,-1.67889591755103,
176.846705834293));
#14688=CARTESIAN_POINT('Ctrl Pts',(-55.0215162671022,-1.64716827604208,
176.934897450488));
#14689=CARTESIAN_POINT('Ctrl Pts',(-54.9831012773678,-1.62642361195712,
176.988063802692));
#14690=CARTESIAN_POINT('Ctrl Pts',(-54.9611536226478,-1.61438316700751,
177.018013216499));
#14691=CARTESIAN_POINT('Ctrl Pts',(-49.4509304485228,-27.5317240793367,
176.63793339336));
#14692=CARTESIAN_POINT('Ctrl Pts',(-49.4291393884885,-27.5076562767722,
176.671636728953));
#14693=CARTESIAN_POINT('Ctrl Pts',(-49.4023252814003,-27.49622653535,176.696313164424));
#14694=CARTESIAN_POINT('Ctrl Pts',(-49.3476504462613,-27.4590129437169,
176.750465273433));
#14695=CARTESIAN_POINT('Ctrl Pts',(-49.3184236390985,-27.4399206811032,
176.775937697594));
#14696=CARTESIAN_POINT('Ctrl Pts',(-49.2266057058354,-27.3820561699738,
176.84602259684));
#14697=CARTESIAN_POINT('Ctrl Pts',(-49.1608892759397,-27.3435420466437,
176.883532818161));
#14698=CARTESIAN_POINT('Ctrl Pts',(-48.9520433277106,-27.2233369569446,
176.969216598557));
#14699=CARTESIAN_POINT('Ctrl Pts',(-48.7994772773074,-27.140753695473,176.988359561004));
#14700=CARTESIAN_POINT('Ctrl Pts',(-48.3519200751284,-26.8936813947759,
176.923562975379));
#14701=CARTESIAN_POINT('Ctrl Pts',(-48.0823456895327,-26.734263465041,176.708580257885));
#14702=CARTESIAN_POINT('Ctrl Pts',(-47.8449430900585,-26.4783672905687,
176.126725989992));
#14703=CARTESIAN_POINT('Ctrl Pts',(-47.8767939676907,-26.3778568396964,
175.764012928805));
#14704=CARTESIAN_POINT('Ctrl Pts',(-48.2463197375522,-26.2327937589041,
175.197492946021));
#14705=CARTESIAN_POINT('Ctrl Pts',(-48.5747178643875,-26.1889682126354,
175.01137731386));
#14706=CARTESIAN_POINT('Ctrl Pts',(-49.2462054467177,-26.1087803247027,
174.981703215741));
#14707=CARTESIAN_POINT('Ctrl Pts',(-49.5907543357586,-26.0676212071441,
175.137035562833));
#14708=CARTESIAN_POINT('Ctrl Pts',(-50.009388927793,-25.9343746307825,175.661646016755));
#14709=CARTESIAN_POINT('Ctrl Pts',(-50.0783027352647,-25.8394975457309,
176.025761110018));
#14710=CARTESIAN_POINT('Ctrl Pts',(-49.8988780633176,-25.5959204367964,
176.628597112503));
#14711=CARTESIAN_POINT('Ctrl Pts',(-49.6518990744916,-25.4405710050954,
176.873652740602));
#14712=CARTESIAN_POINT('Ctrl Pts',(-49.0655102948359,-25.1120926941016,
177.024416386827));
#14713=CARTESIAN_POINT('Ctrl Pts',(-48.7382306499136,-24.9412172473198,
176.927283980104));
#14714=CARTESIAN_POINT('Ctrl Pts',(-48.31783324883,-24.6506072191097,176.48408449858));
#14715=CARTESIAN_POINT('Ctrl Pts',(-48.2223197693695,-24.5249427903147,
176.139359044285));
#14716=CARTESIAN_POINT('Ctrl Pts',(-48.3708320195333,-24.3389138358785,
175.495466335841));
#14717=CARTESIAN_POINT('Ctrl Pts',(-48.6129161956615,-24.2782922597527,
175.208867671322));
#14718=CARTESIAN_POINT('Ctrl Pts',(-49.2318343995499,-24.18785243492,174.949625492768));
#14719=CARTESIAN_POINT('Ctrl Pts',(-49.6097264895464,-24.153250081799,174.976039603467));
#14720=CARTESIAN_POINT('Ctrl Pts',(-50.1907740657023,-24.0499499019578,
175.330958269522));
#14721=CARTESIAN_POINT('Ctrl Pts',(-50.3830787723347,-23.9792981329734,
175.653008106489));
#14722=CARTESIAN_POINT('Ctrl Pts',(-50.427159666228,-23.7781136900229,176.297852422263));
#14723=CARTESIAN_POINT('Ctrl Pts',(-50.2832787288339,-23.643180828803,176.621446326487));
#14724=CARTESIAN_POINT('Ctrl Pts',(-49.7924641893585,-23.3338917128074,
176.988303084673));
#14725=CARTESIAN_POINT('Ctrl Pts',(-49.455479895244,-23.1615506277796,177.024112028042));
#14726=CARTESIAN_POINT('Ctrl Pts',(-48.9089639726264,-22.8463871647641,
176.778406765063));
#14727=CARTESIAN_POINT('Ctrl Pts',(-48.699448601228,-22.6985448431478,176.497595410894));
#14728=CARTESIAN_POINT('Ctrl Pts',(-48.6153144001997,-22.4669397150842,
175.854418703293));
#14729=CARTESIAN_POINT('Ctrl Pts',(-48.7438560906085,-22.3839338201049,
175.504557803726));
#14730=CARTESIAN_POINT('Ctrl Pts',(-49.2595227997445,-22.2634194140522,
175.031489327737));
#14731=CARTESIAN_POINT('Ctrl Pts',(-49.6731287428438,-22.2242903845664,
174.93387435438));
#14732=CARTESIAN_POINT('Ctrl Pts',(-50.3871280758708,-22.1273049999089,
175.149675576275));
#14733=CARTESIAN_POINT('Ctrl Pts',(-50.6724659987737,-22.0667095289654,
175.454257853488));
#14734=CARTESIAN_POINT('Ctrl Pts',(-50.8432291330538,-21.8630647724227,
176.162580877915));
#14735=CARTESIAN_POINT('Ctrl Pts',(-50.7223573298116,-21.7238000115757,
176.543315008655));
#14736=CARTESIAN_POINT('Ctrl Pts',(-50.2109398093855,-21.3899066275767,
176.985840165295));
#14737=CARTESIAN_POINT('Ctrl Pts',(-49.8297406934723,-21.1967740899633,
177.034608068765));
#14738=CARTESIAN_POINT('Ctrl Pts',(-49.2383022679982,-20.8522162432738,
176.742643808163));
#14739=CARTESIAN_POINT('Ctrl Pts',(-49.0288695410029,-20.692930608689,176.406589078903));
#14740=CARTESIAN_POINT('Ctrl Pts',(-49.026421127215,-20.4577766282769,175.692082743004));
#14741=CARTESIAN_POINT('Ctrl Pts',(-49.2307435857662,-20.3815547180372,
175.331094438645));
#14742=CARTESIAN_POINT('Ctrl Pts',(-49.8766835352141,-20.269544445424,174.953525304613));
#14743=CARTESIAN_POINT('Ctrl Pts',(-50.2982947167721,-20.234888952096,174.950394529643));
#14744=CARTESIAN_POINT('Ctrl Pts',(-50.9484787003876,-20.125016744292,175.316388781725));
#14745=CARTESIAN_POINT('Ctrl Pts',(-51.1618775184403,-20.046547250015,175.681463428659));
#14746=CARTESIAN_POINT('Ctrl Pts',(-51.1680956128,-19.8172503157992,176.389348367045));
#14747=CARTESIAN_POINT('Ctrl Pts',(-50.9669054157941,-19.6595598406301,
176.731136037536));
#14748=CARTESIAN_POINT('Ctrl Pts',(-50.3735191706099,-19.3104097045359,
177.03446439702));
#14749=CARTESIAN_POINT('Ctrl Pts',(-49.9983681415115,-19.122445314997,176.992069263085));
#14750=CARTESIAN_POINT('Ctrl Pts',(-49.4783291859613,-18.7856098039383,
176.558083132201));
#14751=CARTESIAN_POINT('Ctrl Pts',(-49.3516920035876,-18.6452157185327,
176.179591346513));
#14752=CARTESIAN_POINT('Ctrl Pts',(-49.5099669630901,-18.4404938180664,
175.471248155379));
#14753=CARTESIAN_POINT('Ctrl Pts',(-49.7966826107081,-18.3761869903911,
175.157298861455));
#14754=CARTESIAN_POINT('Ctrl Pts',(-50.5005002255267,-18.2813908051205,
174.934848239897));
#14755=CARTESIAN_POINT('Ctrl Pts',(-50.9163195448478,-18.2427172185017,
175.022527695559));
#14756=CARTESIAN_POINT('Ctrl Pts',(-51.4689900750814,-18.1145211614547,
175.516882458909));
#14757=CARTESIAN_POINT('Ctrl Pts',(-51.5957313663424,-18.0233261232984,
175.908710828391));
#14758=CARTESIAN_POINT('Ctrl Pts',(-51.4475718943418,-17.7582443007608,
176.601404917962));
#14759=CARTESIAN_POINT('Ctrl Pts',(-51.1767645681398,-17.5900571721881,
176.879541091562));
#14760=CARTESIAN_POINT('Ctrl Pts',(-50.5307383316194,-17.2301836239675,
177.028185493998));
#14761=CARTESIAN_POINT('Ctrl Pts',(-50.1698955770676,-17.0410908031352,
176.891376748831));
#14762=CARTESIAN_POINT('Ctrl Pts',(-49.7689671613288,-16.733171977968,176.344861065041));
#14763=CARTESIAN_POINT('Ctrl Pts',(-49.7283236820348,-16.606509721343,175.939499115166));
#14764=CARTESIAN_POINT('Ctrl Pts',(-50.039329025483,-16.4317046321664,175.276913396961));
#14765=CARTESIAN_POINT('Ctrl Pts',(-50.3811663065111,-16.3819545297351,
175.034692629757));
#14766=CARTESIAN_POINT('Ctrl Pts',(-51.1285550225506,-16.289595439286,174.965429755586));
#14767=CARTESIAN_POINT('Ctrl Pts',(-51.5107791504261,-16.247329788901,175.141829956289));
#14768=CARTESIAN_POINT('Ctrl Pts',(-51.9410271179475,-16.0950193648309,
175.742297045045));
#14769=CARTESIAN_POINT('Ctrl Pts',(-51.9772772372669,-15.9825461483302,
176.155328152494));
#14770=CARTESIAN_POINT('Ctrl Pts',(-51.6813604170028,-15.6948169276305,
176.775145838897));
#14771=CARTESIAN_POINT('Ctrl Pts',(-51.3553093740791,-15.5131006527082,
176.981869312707));
#14772=CARTESIAN_POINT('Ctrl Pts',(-50.6958293220101,-15.1512003838696,
176.968860943967));
#14773=CARTESIAN_POINT('Ctrl Pts',(-50.3793004471536,-14.974461104635,176.752883253889));
#14774=CARTESIAN_POINT('Ctrl Pts',(-50.1044053585231,-14.6849545931669,
176.110550614429));
#14775=CARTESIAN_POINT('Ctrl Pts',(-50.1562892256051,-14.5790344049375,
175.704381183727));
#14776=CARTESIAN_POINT('Ctrl Pts',(-50.6091148636379,-14.4310075872896,
175.119365593043));
#14777=CARTESIAN_POINT('Ctrl Pts',(-51.0040002342342,-14.3877335732316,
174.956144468714));
#14778=CARTESIAN_POINT('Ctrl Pts',(-51.7368765161625,-14.2984333198446,
175.052400920313));
#14779=CARTESIAN_POINT('Ctrl Pts',(-52.0746787278137,-14.2446881736679,
175.307721150405));
#14780=CARTESIAN_POINT('Ctrl Pts',(-52.3618029222314,-14.0653384618121,
175.979593696432));
#14781=CARTESIAN_POINT('Ctrl Pts',(-52.3085224478133,-13.9393545956389,
176.378830696363));
#14782=CARTESIAN_POINT('Ctrl Pts',(-51.8806097785072,-13.6203167705008,
176.914733769747));
#14783=CARTESIAN_POINT('Ctrl Pts',(-51.5196766160896,-13.4348339691437,
177.033422941425));
#14784=CARTESIAN_POINT('Ctrl Pts',(-50.8796650354229,-13.0760747213028,
176.857816848924));
#14785=CARTESIAN_POINT('Ctrl Pts',(-50.6171262914928,-12.905954023484,176.563294278628));
#14786=CARTESIAN_POINT('Ctrl Pts',(-50.4974416512911,-12.6523824704848,
175.874038771655));
#14787=CARTESIAN_POINT('Ctrl Pts',(-50.6384867622314,-12.5605842376971,
175.481424733232));
#14788=CARTESIAN_POINT('Ctrl Pts',(-51.2082627201524,-12.4357774521296,
175.006422958104));
#14789=CARTESIAN_POINT('Ctrl Pts',(-51.6220204445227,-12.3999030775176,
174.932310130414));
#14790=CARTESIAN_POINT('Ctrl Pts',(-52.3278760969134,-12.2994377602634,
175.185413156184));
#14791=CARTESIAN_POINT('Ctrl Pts',(-52.5969267492371,-12.2353856775628,
175.505423112887));
#14792=CARTESIAN_POINT('Ctrl Pts',(-52.7283564524999,-12.0255423744405,
176.2175433277));
#14793=CARTESIAN_POINT('Ctrl Pts',(-52.5846730379872,-11.8782873041682,
176.594912064781));
#14794=CARTESIAN_POINT('Ctrl Pts',(-52.0559417647627,-11.5457913524836,
176.999632681105));
#14795=CARTESIAN_POINT('Ctrl Pts',(-51.6759748702359,-11.3536364027873,
177.029489895259));
#14796=CARTESIAN_POINT('Ctrl Pts',(-51.0935427887116,-11.0064931497742,
176.702663500826));
#14797=CARTESIAN_POINT('Ctrl Pts',(-50.9048767955961,-10.8544314216914,
176.357244031546));
#14798=CARTESIAN_POINT('Ctrl Pts',(-50.9399834898308,-10.6247204655602,
175.63759182164));
#14799=CARTESIAN_POINT('Ctrl Pts',(-51.1643267174014,-10.5520247194105,
175.286394351447));
#14800=CARTESIAN_POINT('Ctrl Pts',(-51.827873009513,-10.4447251212865,174.944424130566));
#14801=CARTESIAN_POINT('Ctrl Pts',(-52.2552179028772,-10.4077182802165,
174.964702471846));
#14802=CARTESIAN_POINT('Ctrl Pts',(-52.8763669051787,-10.2968258721765,
175.360239151239));
#14803=CARTESIAN_POINT('Ctrl Pts',(-53.071683414474,-10.215593033151,175.73103698433));
#14804=CARTESIAN_POINT('Ctrl Pts',(-53.0437675059112,-9.97549498249197,
176.443487491333));
#14805=CARTESIAN_POINT('Ctrl Pts',(-52.825568431635,-9.81766629245078,176.768582048511));
#14806=CARTESIAN_POINT('Ctrl Pts',(-52.2143534856381,-9.46331409552581,
177.038351228206));
#14807=CARTESIAN_POINT('Ctrl Pts',(-51.8411412849432,-9.27545967967225,
176.973585868646));
#14808=CARTESIAN_POINT('Ctrl Pts',(-51.3467118649778,-8.94477024831946,
176.509526159241));
#14809=CARTESIAN_POINT('Ctrl Pts',(-51.2404836863797,-8.80483732687828,
176.117599105019));
#14810=CARTESIAN_POINT('Ctrl Pts',(-51.4349583516297,-8.61185430488912,
175.425788146171));
#14811=CARTESIAN_POINT('Ctrl Pts',(-51.7335486000159,-8.55040314694308,
175.126384517701));
#14812=CARTESIAN_POINT('Ctrl Pts',(-52.4549196826756,-8.45481293341497,
174.935526629257));
#14813=CARTESIAN_POINT('Ctrl Pts',(-52.8607223331575,-8.41739346719437,
175.04474867484));
#14814=CARTESIAN_POINT('Ctrl Pts',(-53.3897252776085,-8.28282809274167,
175.568595073035));
#14815=CARTESIAN_POINT('Ctrl Pts',(-53.4952826969923,-8.1872595086965,175.966830212787));
#14816=CARTESIAN_POINT('Ctrl Pts',(-53.3101642867802,-7.91637813164073,
176.645610777581));
#14817=CARTESIAN_POINT('Ctrl Pts',(-53.02056762136,-7.74105352934409,176.910070201754));
#14818=CARTESIAN_POINT('Ctrl Pts',(-52.3751524190461,-7.38599804306437,
177.017607675131));
#14819=CARTESIAN_POINT('Ctrl Pts',(-52.0232566558232,-7.19924964083975,
176.864225220861));
#14820=CARTESIAN_POINT('Ctrl Pts',(-51.6458284953554,-6.89163712519652,
176.29020971736));
#14821=CARTESIAN_POINT('Ctrl Pts',(-51.6277644578821,-6.7724816775637,175.885858382765));
#14822=CARTESIAN_POINT('Ctrl Pts',(-51.9747906942483,-6.6028499237395,175.235443151034));
#14823=CARTESIAN_POINT('Ctrl Pts',(-52.3299962525585,-6.55546850196264,
175.011060208135));
#14824=CARTESIAN_POINT('Ctrl Pts',(-53.0782096175287,-6.46444741567071,
174.9816560919));
#14825=CARTESIAN_POINT('Ctrl Pts',(-53.4553178435249,-6.41778988524295,
175.181401713961));
#14826=CARTESIAN_POINT('Ctrl Pts',(-53.8466529433518,-6.26265155715774,
175.795420851333));
#14827=CARTESIAN_POINT('Ctrl Pts',(-53.864188958285,-6.14704492720176,176.206287912404));
#14828=CARTESIAN_POINT('Ctrl Pts',(-53.5358416511927,-5.84903598495515,
176.813977641948));
#14829=CARTESIAN_POINT('Ctrl Pts',(-53.2017653978813,-5.66889429660941,
176.99856451113));
#14830=CARTESIAN_POINT('Ctrl Pts',(-52.5405403606902,-5.30479587533914,
176.947248559284));
#14831=CARTESIAN_POINT('Ctrl Pts',(-52.2356929075399,-5.13012364220884,
176.712058308829));
#14832=CARTESIAN_POINT('Ctrl Pts',(-51.9967219623743,-4.84888631606004,
176.054758979681));
#14833=CARTESIAN_POINT('Ctrl Pts',(-52.0727509238964,-4.74401755802611,
175.645031481929));
#14834=CARTESIAN_POINT('Ctrl Pts',(-52.5505176724514,-4.6056507589775,175.091566392661));
#14835=CARTESIAN_POINT('Ctrl Pts',(-52.9499574883172,-4.56374410570602,
174.946492448473));
#14836=CARTESIAN_POINT('Ctrl Pts',(-53.685231908784,-4.47066113931358,175.078743542747));
#14837=CARTESIAN_POINT('Ctrl Pts',(-54.0046084640979,-4.41655583760205,
175.349203817777));
#14838=CARTESIAN_POINT('Ctrl Pts',(-54.2577428662421,-4.2288827567675,176.036685454146));
#14839=CARTESIAN_POINT('Ctrl Pts',(-54.1828214302285,-4.09851492101137,
176.431966849275));
#14840=CARTESIAN_POINT('Ctrl Pts',(-53.7276699197103,-3.77548143923658,
176.939160233154));
#14841=CARTESIAN_POINT('Ctrl Pts',(-53.3559275609679,-3.58443131799679,
177.036850521868));
#14842=CARTESIAN_POINT('Ctrl Pts',(-52.7340684542075,-3.23387064793483,
176.825149499914));
#14843=CARTESIAN_POINT('Ctrl Pts',(-52.4865052787647,-3.06716804391598,
176.519600526728));
#14844=CARTESIAN_POINT('Ctrl Pts',(-52.4000162427049,-2.81575249291398,
175.815720536334));
#14845=CARTESIAN_POINT('Ctrl Pts',(-52.5606356723736,-2.73100846880393,
175.434725535823));
#14846=CARTESIAN_POINT('Ctrl Pts',(-53.1578253291134,-2.60958353788362,
174.986380686329));
#14847=CARTESIAN_POINT('Ctrl Pts',(-53.575919582614,-2.57427864177586,174.934476257966));
#14848=CARTESIAN_POINT('Ctrl Pts',(-54.2645385526377,-2.47204238084449,
175.223470220004));
#14849=CARTESIAN_POINT('Ctrl Pts',(-54.5189943505689,-2.4021627120238,175.561903562137));
#14850=CARTESIAN_POINT('Ctrl Pts',(-54.5814297773468,-2.25612793931688,
176.045419377677));
#14851=CARTESIAN_POINT('Ctrl Pts',(-54.5735173041519,-2.21013144506474,
176.178993521001));
#14852=CARTESIAN_POINT('Ctrl Pts',(-54.5239654997844,-2.13806319233694,
176.36226950621));
#14853=CARTESIAN_POINT('Ctrl Pts',(-54.5010361022764,-2.1121733501921,176.42270110964));
#14854=CARTESIAN_POINT('Ctrl Pts',(-54.4586925003588,-2.07172971741335,
176.508171829538));
#14855=CARTESIAN_POINT('Ctrl Pts',(-54.4432559654462,-2.05799768545568,
176.53580222906));
#14856=CARTESIAN_POINT('Ctrl Pts',(-54.410122331684,-2.03029642349882,176.588723178982));
#14857=CARTESIAN_POINT('Ctrl Pts',(-54.3884821434676,-2.0139079395113,176.618668306411));
#14858=CARTESIAN_POINT('Ctrl Pts',(-54.3738267566562,-2.00237092626598,
176.637865020199));
#14859=CARTESIAN_POINT('Ctrl Pts',(-49.6057233026533,-28.1882175989763,
177.068114089093));
#14860=CARTESIAN_POINT('Ctrl Pts',(-49.5663192275732,-28.1656109096198,
177.105925367078));
#14861=CARTESIAN_POINT('Ctrl Pts',(-49.5216854287654,-28.1457023853521,
177.148383027181));
#14862=CARTESIAN_POINT('Ctrl Pts',(-49.4301127133764,-28.1014695235449,
177.220446553382));
#14863=CARTESIAN_POINT('Ctrl Pts',(-49.3819809603125,-28.0788363277035,
177.253617740645));
#14864=CARTESIAN_POINT('Ctrl Pts',(-49.2321484222821,-28.0099337266433,
177.343479018307));
#14865=CARTESIAN_POINT('Ctrl Pts',(-49.1254026293825,-27.9629901656525,
177.390284377819));
#14866=CARTESIAN_POINT('Ctrl Pts',(-48.7929164986652,-27.8189908160803,
177.48590296908));
#14867=CARTESIAN_POINT('Ctrl Pts',(-48.55635218661,-27.7202377019268,177.490394220553));
#14868=CARTESIAN_POINT('Ctrl Pts',(-47.8840648999533,-27.4305281812212,
177.324447440169));
#14869=CARTESIAN_POINT('Ctrl Pts',(-47.5006474873523,-27.2497443022818,
176.963331771584));
#14870=CARTESIAN_POINT('Ctrl Pts',(-47.2040861213115,-26.9802047380462,
176.046394548579));
#14871=CARTESIAN_POINT('Ctrl Pts',(-47.2954018922066,-26.8917044501032,
175.506598760119));
#14872=CARTESIAN_POINT('Ctrl Pts',(-47.9062028356891,-26.7943163650827,
174.710326627486));
#14873=CARTESIAN_POINT('Ctrl Pts',(-48.4108882632775,-26.7850298620733,
174.47568647468));
#14874=CARTESIAN_POINT('Ctrl Pts',(-49.4081207961382,-26.7654318876047,
174.522051214009));
#14875=CARTESIAN_POINT('Ctrl Pts',(-49.8895805322777,-26.7512165827191,
174.803706734764));
#14876=CARTESIAN_POINT('Ctrl Pts',(-50.419859907048,-26.6406327974915,175.641132157405));
#14877=CARTESIAN_POINT('Ctrl Pts',(-50.4638072135826,-26.5414518590087,
176.190943138814));
#14878=CARTESIAN_POINT('Ctrl Pts',(-50.0902675056585,-26.258306693899,177.06820282525));
#14879=CARTESIAN_POINT('Ctrl Pts',(-49.6753169680471,-26.0710530131776,
177.393289133135));
#14880=CARTESIAN_POINT('Ctrl Pts',(-48.760110273011,-25.6803067135432,177.526354227003));
#14881=CARTESIAN_POINT('Ctrl Pts',(-48.2752065557733,-25.4795815288234,
177.333261554155));
#14882=CARTESIAN_POINT('Ctrl Pts',(-47.6834949732814,-25.1537104488559,
176.598820399841));
#14883=CARTESIAN_POINT('Ctrl Pts',(-47.581935800625,-25.0274199406948,176.066471856633));
#14884=CARTESIAN_POINT('Ctrl Pts',(-47.8743577335121,-24.8702793490883,
175.122570330099));
#14885=CARTESIAN_POINT('Ctrl Pts',(-48.2639300332364,-24.8386062285325,
174.72605490093));
#14886=CARTESIAN_POINT('Ctrl Pts',(-49.2134664973944,-24.8097944361078,
174.418869413643));
#14887=CARTESIAN_POINT('Ctrl Pts',(-49.7639560285487,-24.8089577046691,
174.513086690221));
#14888=CARTESIAN_POINT('Ctrl Pts',(-50.5601436025432,-24.7482854574026,
175.121296078095));
#14889=CARTESIAN_POINT('Ctrl Pts',(-50.7937850628585,-24.6861522884041,
175.625415363842));
#14890=CARTESIAN_POINT('Ctrl Pts',(-50.7513118113109,-24.4660502953853,
176.598470930813));
#14891=CARTESIAN_POINT('Ctrl Pts',(-50.4787452748198,-24.3068424850894,
177.056448064075));
#14892=CARTESIAN_POINT('Ctrl Pts',(-49.6755858463959,-23.9384579984121,
177.525629368769));
#14893=CARTESIAN_POINT('Ctrl Pts',(-49.1583261106009,-23.7318611386462,
177.529378707235));
#14894=CARTESIAN_POINT('Ctrl Pts',(-48.3492917504345,-23.3639427741862,
177.074636497803));
#14895=CARTESIAN_POINT('Ctrl Pts',(-48.0678997211374,-23.2027238239874,
176.620161976926));
#14896=CARTESIAN_POINT('Ctrl Pts',(-48.0133698591323,-22.9779683240005,
175.643265853549));
#14897=CARTESIAN_POINT('Ctrl Pts',(-48.2419634078688,-22.9148026311583,
175.13669620061));
#14898=CARTESIAN_POINT('Ctrl Pts',(-49.0648716087653,-22.8512007031896,
174.491772947554));
#14899=CARTESIAN_POINT('Ctrl Pts',(-49.6839608902416,-22.8528771386521,
174.405900021421));
#14900=CARTESIAN_POINT('Ctrl Pts',(-50.6991943315865,-22.8143164724711,
174.826217042058));
#14901=CARTESIAN_POINT('Ctrl Pts',(-51.0745700439279,-22.7701586995258,
175.322569579276));
#14902=CARTESIAN_POINT('Ctrl Pts',(-51.2073695092728,-22.5604456438022,
176.396956445951));
#14903=CARTESIAN_POINT('Ctrl Pts',(-50.9625278765238,-22.3963905325425,
176.94851178212));
#14904=CARTESIAN_POINT('Ctrl Pts',(-50.1139689940341,-21.9977514714476,
177.529315681618));
#14905=CARTESIAN_POINT('Ctrl Pts',(-49.5293219694751,-21.7666067892758,
177.544699935169));
#14906=CARTESIAN_POINT('Ctrl Pts',(-48.6567664449969,-21.3653910132907,
177.013098304479));
#14907=CARTESIAN_POINT('Ctrl Pts',(-48.383128531039,-21.1949054338945,176.477577858981));
#14908=CARTESIAN_POINT('Ctrl Pts',(-48.4582777380059,-20.975048733324,175.402873064259));
#14909=CARTESIAN_POINT('Ctrl Pts',(-48.8055781932514,-20.9254744005303,
174.886960050279));
#14910=CARTESIAN_POINT('Ctrl Pts',(-49.7998797569528,-20.8818943796597,
174.412232108109));
#14911=CARTESIAN_POINT('Ctrl Pts',(-50.4230224397188,-20.885216808613,174.464849386198));
#14912=CARTESIAN_POINT('Ctrl Pts',(-51.3220781362712,-20.8236066704411,
175.100442044691));
#14913=CARTESIAN_POINT('Ctrl Pts',(-51.5785314568021,-20.7546592125729,
175.670463366294));
#14914=CARTESIAN_POINT('Ctrl Pts',(-51.4682882413066,-20.5004564781585,
176.732562819156));
#14915=CARTESIAN_POINT('Ctrl Pts',(-51.1076577914431,-20.313201754554,177.207532153307));
#14916=CARTESIAN_POINT('Ctrl Pts',(-50.156411198824,-19.8953744930702,177.56803029022));
#14917=CARTESIAN_POINT('Ctrl Pts',(-49.5878400685962,-19.6691878319784,
177.446385146947));
#14918=CARTESIAN_POINT('Ctrl Pts',(-48.852079415717,-19.2920053425884,176.716949064536));
#14919=CARTESIAN_POINT('Ctrl Pts',(-48.7034574890464,-19.1464856081966,
176.127114392609));
#14920=CARTESIAN_POINT('Ctrl Pts',(-49.017896392823,-18.9721498737463,175.084671234462));
#14921=CARTESIAN_POINT('Ctrl Pts',(-49.4761175027563,-18.9421345006494,
174.655217811997));
#14922=CARTESIAN_POINT('Ctrl Pts',(-50.5469446991098,-18.915664221674,174.415005106013));
#14923=CARTESIAN_POINT('Ctrl Pts',(-51.1421889783774,-18.9127734302845,
174.605352538579));
#14924=CARTESIAN_POINT('Ctrl Pts',(-51.8771202801842,-18.8200557591642,
175.418505113175));
#14925=CARTESIAN_POINT('Ctrl Pts',(-52.0018165496213,-18.7275436462981,
176.022835099282));
#14926=CARTESIAN_POINT('Ctrl Pts',(-51.6614363875286,-18.4266465795959,
177.027259608014));
#14927=CARTESIAN_POINT('Ctrl Pts',(-51.2055166082591,-18.2218754080822,
177.403206831321));
#14928=CARTESIAN_POINT('Ctrl Pts',(-50.1969770591628,-17.7923688711786,
177.524973109627));
#14929=CARTESIAN_POINT('Ctrl Pts',(-49.6679526067506,-17.5720619524455,
177.267256975221));
#14930=CARTESIAN_POINT('Ctrl Pts',(-49.1179984398299,-17.2329564925234,
176.379271882249));
#14931=CARTESIAN_POINT('Ctrl Pts',(-49.1058293111544,-17.1129691055462,
175.766207634738));
#14932=CARTESIAN_POINT('Ctrl Pts',(-49.6421979468107,-16.981953011196,174.814805282058));
#14933=CARTESIAN_POINT('Ctrl Pts',(-50.1794692968359,-16.96896833752,174.497498655776));
#14934=CARTESIAN_POINT('Ctrl Pts',(-51.2815033366288,-16.9462509137644,
174.497183387712));
#14935=CARTESIAN_POINT('Ctrl Pts',(-51.8206810039433,-16.9333636766774,
174.813868002799));
#14936=CARTESIAN_POINT('Ctrl Pts',(-52.3579329121243,-16.8019633847227,
175.767995550527));
#14937=CARTESIAN_POINT('Ctrl Pts',(-52.3444015552563,-16.6811074119364,
176.384253300385));
#14938=CARTESIAN_POINT('Ctrl Pts',(-51.7908025496479,-16.3412377353734,
177.270036214878));
#14939=CARTESIAN_POINT('Ctrl Pts',(-51.2640575414935,-16.1220052064028,
177.524939199898));
#14940=CARTESIAN_POINT('Ctrl Pts',(-50.2584821099884,-15.6936926334193,
177.402964762685));
#14941=CARTESIAN_POINT('Ctrl Pts',(-49.8024659570259,-15.4891340123335,
177.028965203342));
#14942=CARTESIAN_POINT('Ctrl Pts',(-49.4615190985809,-15.1881425443655,
176.024838210267));
#14943=CARTESIAN_POINT('Ctrl Pts',(-49.584917871472,-15.0951235636284,175.418993178211));
#14944=CARTESIAN_POINT('Ctrl Pts',(-50.3224323861862,-15.0022736039987,
174.603877612758));
#14945=CARTESIAN_POINT('Ctrl Pts',(-50.9209588419739,-14.9994851008446,
174.413907495741));
#14946=CARTESIAN_POINT('Ctrl Pts',(-51.9913299824675,-14.9728180278691,
174.658436700836));
#14947=CARTESIAN_POINT('Ctrl Pts',(-52.4458562262816,-14.942768055369,175.086526075902));
#14948=CARTESIAN_POINT('Ctrl Pts',(-52.7589234637054,-14.768747576336,176.126312497655));
#14949=CARTESIAN_POINT('Ctrl Pts',(-52.6119738826496,-14.6237809758753,
176.715478760326));
#14950=CARTESIAN_POINT('Ctrl Pts',(-51.8767097042875,-14.2467264136774,
177.445252299972));
#14951=CARTESIAN_POINT('Ctrl Pts',(-51.3074205647036,-14.0201741438431,
177.568755188896));
#14952=CARTESIAN_POINT('Ctrl Pts',(-50.3534291722187,-13.6011459302421,
177.20657523661));
#14953=CARTESIAN_POINT('Ctrl Pts',(-49.9921349812078,-13.4131957453291,
176.728222347554));
#14954=CARTESIAN_POINT('Ctrl Pts',(-49.8860852889645,-13.159806046502,175.66552302478));
#14955=CARTESIAN_POINT('Ctrl Pts',(-50.1425376823364,-13.0914495220188,
175.099033652958));
#14956=CARTESIAN_POINT('Ctrl Pts',(-51.0393482876635,-13.0300320803285,
174.465742160163));
#14957=CARTESIAN_POINT('Ctrl Pts',(-51.661049564308,-13.0333384108268,174.411629490546));
#14958=CARTESIAN_POINT('Ctrl Pts',(-52.6556849728402,-12.9898139344045,
174.885756683857));
#14959=CARTESIAN_POINT('Ctrl Pts',(-53.0050117718212,-12.9403514819039,
175.401975295897));
#14960=CARTESIAN_POINT('Ctrl Pts',(-53.0797917942593,-12.7198628954119,
176.47950485369));
#14961=CARTESIAN_POINT('Ctrl Pts',(-52.8035180796908,-12.5482535501767,
177.017249165378));
#14962=CARTESIAN_POINT('Ctrl Pts',(-51.928756778869,-12.1465816152287,177.545168184464));
#14963=CARTESIAN_POINT('Ctrl Pts',(-51.3476399628683,-11.9168238447545,
177.52855345072));
#14964=CARTESIAN_POINT('Ctrl Pts',(-50.5013329357435,-11.5191203268418,
176.948730973903));
#14965=CARTESIAN_POINT('Ctrl Pts',(-50.2557375091139,-11.3551615877155,
176.398843509589));
#14966=CARTESIAN_POINT('Ctrl Pts',(-50.3877927376681,-11.145398461788,175.324825412843));
#14967=CARTESIAN_POINT('Ctrl Pts',(-50.762684868614,-11.1008426423184,174.826271833705));
#14968=CARTESIAN_POINT('Ctrl Pts',(-51.7811268292925,-11.0622619854364,
174.405264562934));
#14969=CARTESIAN_POINT('Ctrl Pts',(-52.4028793467296,-11.063958202758,174.492793292778));
#14970=CARTESIAN_POINT('Ctrl Pts',(-53.2632154661256,-10.9967409315864,
175.172494096186));
#14971=CARTESIAN_POINT('Ctrl Pts',(-53.4886849878534,-10.9225114509841,
175.750866168407));
#14972=CARTESIAN_POINT('Ctrl Pts',(-53.3251423960266,-10.6565821386363,
176.805379202472));
#14973=CARTESIAN_POINT('Ctrl Pts',(-52.9407422532226,-10.465785944074,177.259010843821));
#14974=CARTESIAN_POINT('Ctrl Pts',(-51.9697953271392,-10.0433159226031,
177.565260787091));
#14975=CARTESIAN_POINT('Ctrl Pts',(-51.4073968434514,-9.81808614025534,
177.411394538556));
#14976=CARTESIAN_POINT('Ctrl Pts',(-50.7116066211125,-9.44884954788431,
176.639139203566));
#14977=CARTESIAN_POINT('Ctrl Pts',(-50.5960828064805,-9.30833579234248,
176.038056438509));
#14978=CARTESIAN_POINT('Ctrl Pts',(-50.9640903737478,-9.14636922546571,
175.0167568496));
#14979=CARTESIAN_POINT('Ctrl Pts',(-51.4414488535671,-9.12058052193367,
174.612974652851));
#14980=CARTESIAN_POINT('Ctrl Pts',(-52.5249204417031,-9.09513784416194,
174.426509843431));
#14981=CARTESIAN_POINT('Ctrl Pts',(-53.1088418277628,-9.09114996369398,
174.646804488947));
#14982=CARTESIAN_POINT('Ctrl Pts',(-53.801661971168,-8.98942785386125,175.498626413927));
#14983=CARTESIAN_POINT('Ctrl Pts',(-53.8945655335682,-8.89052591977855,
176.108945227942));
#14984=CARTESIAN_POINT('Ctrl Pts',(-53.5007325042087,-8.57967938234873,
177.090495387502));
#14985=CARTESIAN_POINT('Ctrl Pts',(-53.0228734977247,-8.36926263084827,
177.439659990072));
#14986=CARTESIAN_POINT('Ctrl Pts',(-52.0134388460396,-7.941561484533,177.502665384752));
#14987=CARTESIAN_POINT('Ctrl Pts',(-51.5009539686643,-7.72503451842822,
177.217498325365));
#14988=CARTESIAN_POINT('Ctrl Pts',(-50.9958226444158,-7.39311721565184,
176.298072843289));
#14989=CARTESIAN_POINT('Ctrl Pts',(-51.0149583411939,-7.28021855779389,
175.684524900703));
#14990=CARTESIAN_POINT('Ctrl Pts',(-51.602189663565,-7.15816051285745,174.759352960774));
#14991=CARTESIAN_POINT('Ctrl Pts',(-52.1561751142271,-7.14821693453925,
174.470064567704));
#14992=CARTESIAN_POINT('Ctrl Pts',(-53.257284967077,-7.12553378294388,174.528734890764));
#14993=CARTESIAN_POINT('Ctrl Pts',(-53.7798318899166,-7.10813319884164,
174.876062446534));
#14994=CARTESIAN_POINT('Ctrl Pts',(-54.263309402104,-6.96831483361839,175.852098283111));
#14995=CARTESIAN_POINT('Ctrl Pts',(-54.2182177005742,-6.84182185515181,
176.463118413));
#14996=CARTESIAN_POINT('Ctrl Pts',(-53.620326169719,-6.49215310837908,177.317242942806));
#14997=CARTESIAN_POINT('Ctrl Pts',(-53.0815432796407,-6.27162057701451,
177.542753252723));
#14998=CARTESIAN_POINT('Ctrl Pts',(-52.0813405764902,-5.84340716815714,
177.363069610828));
#14999=CARTESIAN_POINT('Ctrl Pts',(-51.6451899827477,-5.64252013198273,
176.962963727015));
#15000=CARTESIAN_POINT('Ctrl Pts',(-51.3585173428123,-5.35236886702559,
175.939011043839));
#15001=CARTESIAN_POINT('Ctrl Pts',(-51.5164782073777,-5.2645103327986,175.337256223397));
#15002=CARTESIAN_POINT('Ctrl Pts',(-52.2924300679745,-5.18119763163266,
174.565366155634));
#15003=CARTESIAN_POINT('Ctrl Pts',(-52.8973452213176,-5.1801045826173,174.406680096152));
#15004=CARTESIAN_POINT('Ctrl Pts',(-53.956162505713,-5.14973256956073,174.705214074754));
#15005=CARTESIAN_POINT('Ctrl Pts',(-54.3874707400874,-5.11629663400306,
175.155234787811));
#15006=CARTESIAN_POINT('Ctrl Pts',(-54.6460006492434,-4.93091655090319,
176.210608238885));
#15007=CARTESIAN_POINT('Ctrl Pts',(-54.4681690759566,-4.77980797892323,
176.790635503925));
#15008=CARTESIAN_POINT('Ctrl Pts',(-53.6946945331643,-4.3956772156615,177.47627897342));
#15009=CARTESIAN_POINT('Ctrl Pts',(-53.1174419759953,-4.16620647621949,
177.565792133827));
#15010=CARTESIAN_POINT('Ctrl Pts',(-52.1878574222778,-3.75385530866336,
177.150829002666));
#15011=CARTESIAN_POINT('Ctrl Pts',(-51.8529856411974,-3.5715083216093,176.654958973924));
#15012=CARTESIAN_POINT('Ctrl Pts',(-51.8010050251376,-3.32706416715232,
175.583828138226));
#15013=CARTESIAN_POINT('Ctrl Pts',(-52.0854219579878,-3.26527816982496,
175.031488604324));
#15014=CARTESIAN_POINT('Ctrl Pts',(-53.0170398348192,-3.20959915076688,
174.444132662069));
#15015=CARTESIAN_POINT('Ctrl Pts',(-53.6416591927321,-3.21325709639781,
174.423035709656));
#15016=CARTESIAN_POINT('Ctrl Pts',(-54.6090153740635,-3.16498595686182,
174.948967905512));
#15017=CARTESIAN_POINT('Ctrl Pts',(-54.9308286711417,-3.10893139642228,
175.48555871107));
#15018=CARTESIAN_POINT('Ctrl Pts',(-54.9426665516143,-2.95192631073098,
176.218540695264));
#15019=CARTESIAN_POINT('Ctrl Pts',(-54.9070365263685,-2.90171640292054,
176.413787336324));
#15020=CARTESIAN_POINT('Ctrl Pts',(-54.8013987998623,-2.81782847468563,
176.681821034794));
#15021=CARTESIAN_POINT('Ctrl Pts',(-54.7570848510793,-2.78787367953458,
176.767627228561));
#15022=CARTESIAN_POINT('Ctrl Pts',(-54.6793253219128,-2.74078668455889,
176.887592985838));
#15023=CARTESIAN_POINT('Ctrl Pts',(-54.651529701944,-2.72473899696222,176.926133356148));
#15024=CARTESIAN_POINT('Ctrl Pts',(-54.5925997439423,-2.69209575899625,
176.999824075839));
#15025=CARTESIAN_POINT('Ctrl Pts',(-54.5641015373143,-2.67654794454284,
177.031971691023));
#15026=CARTESIAN_POINT('Ctrl Pts',(-54.5288628436534,-2.65870383148503,
177.068203177065));
#15027=CARTESIAN_POINT('Ctrl Pts',(-49.7605161567837,-28.8447111186158,
177.498294784826));
#15028=CARTESIAN_POINT('Ctrl Pts',(-49.703499066658,-28.8235655424673,177.540214005203));
#15029=CARTESIAN_POINT('Ctrl Pts',(-49.6410455761305,-28.7951782353542,
177.600452889938));
#15030=CARTESIAN_POINT('Ctrl Pts',(-49.5125749804916,-28.7439261033728,
177.690427833332));
#15031=CARTESIAN_POINT('Ctrl Pts',(-49.4455382815264,-28.7177519743038,
177.731297783696));
#15032=CARTESIAN_POINT('Ctrl Pts',(-49.2376911387288,-28.6378112833129,
177.840935439774));
#15033=CARTESIAN_POINT('Ctrl Pts',(-49.0899159828253,-28.5824382846613,
177.897035937477));
#15034=CARTESIAN_POINT('Ctrl Pts',(-48.6337896696199,-28.4146446752159,
178.002589339604));
#15035=CARTESIAN_POINT('Ctrl Pts',(-48.3132270959126,-28.2997217083806,
177.992428880102));
#15036=CARTESIAN_POINT('Ctrl Pts',(-47.4162097247782,-27.9673749676665,
177.725331904959));
#15037=CARTESIAN_POINT('Ctrl Pts',(-46.9189492851719,-27.7652251395226,
177.218083285283));
#15038=CARTESIAN_POINT('Ctrl Pts',(-46.5632291525645,-27.4820421855238,
175.966063107167));
#15039=CARTESIAN_POINT('Ctrl Pts',(-46.7140098167225,-27.4055520605101,
175.249184591433));
#15040=CARTESIAN_POINT('Ctrl Pts',(-47.566085933826,-27.3558389712614,174.223160308952));
#15041=CARTESIAN_POINT('Ctrl Pts',(-48.2470586621674,-27.3810915115113,
173.939995635501));
#15042=CARTESIAN_POINT('Ctrl Pts',(-49.5700361455588,-27.4220834505067,
174.062399212278));
#15043=CARTESIAN_POINT('Ctrl Pts',(-50.1884067287968,-27.434811958294,174.470377906696));
#15044=CARTESIAN_POINT('Ctrl Pts',(-50.8303308863031,-27.3468909642006,
175.620618298056));
#15045=CARTESIAN_POINT('Ctrl Pts',(-50.8493116919004,-27.2434061722865,
176.356125167609));
#15046=CARTESIAN_POINT('Ctrl Pts',(-50.2816569479994,-26.9206929510016,
177.507808537998));
#15047=CARTESIAN_POINT('Ctrl Pts',(-49.6987348616025,-26.7015350212598,
177.912925525668));
#15048=CARTESIAN_POINT('Ctrl Pts',(-48.454710251186,-26.2485207329848,178.028292067179));
#15049=CARTESIAN_POINT('Ctrl Pts',(-47.8121824616331,-26.017945810327,177.739239128205));
#15050=CARTESIAN_POINT('Ctrl Pts',(-47.0491566977328,-25.6568136786021,
176.713556301102));
#15051=CARTESIAN_POINT('Ctrl Pts',(-46.9415518318806,-25.5298970910749,
175.993584668982));
#15052=CARTESIAN_POINT('Ctrl Pts',(-47.3778834474909,-25.4016448622981,
174.749674324357));
#15053=CARTESIAN_POINT('Ctrl Pts',(-47.9149438708112,-25.3989201973124,
174.243242130538));
#15054=CARTESIAN_POINT('Ctrl Pts',(-49.195098595239,-25.4317364372956,173.888113334518));
#15055=CARTESIAN_POINT('Ctrl Pts',(-49.918185567551,-25.4646653275392,174.050133776974));
#15056=CARTESIAN_POINT('Ctrl Pts',(-50.9295131393841,-25.4466210128473,
174.911633886668));
#15057=CARTESIAN_POINT('Ctrl Pts',(-51.2044913533823,-25.3930064438348,
175.597822621196));
#15058=CARTESIAN_POINT('Ctrl Pts',(-51.0754639563939,-25.1539869007477,
176.899089439364));
#15059=CARTESIAN_POINT('Ctrl Pts',(-50.6742118208058,-24.9705041413757,
177.491449801663));
#15060=CARTESIAN_POINT('Ctrl Pts',(-49.5587075034334,-24.5430242840169,
178.062955652865));
#15061=CARTESIAN_POINT('Ctrl Pts',(-48.8611723259578,-24.3021716495128,
178.034645386427));
#15062=CARTESIAN_POINT('Ctrl Pts',(-47.7896195282427,-23.8814983836082,
177.370866230542));
#15063=CARTESIAN_POINT('Ctrl Pts',(-47.4363508410467,-23.7069028048269,
176.742728542957));
#15064=CARTESIAN_POINT('Ctrl Pts',(-47.4114253180649,-23.4889969329168,
175.432113003805));
#15065=CARTESIAN_POINT('Ctrl Pts',(-47.740070725129,-23.4456714422117,174.768834597493));
#15066=CARTESIAN_POINT('Ctrl Pts',(-48.8702204177861,-23.4389819923271,
173.952056567371));
#15067=CARTESIAN_POINT('Ctrl Pts',(-49.6947930376395,-23.4814638927378,
173.877925688461));
#15068=CARTESIAN_POINT('Ctrl Pts',(-51.0112605873021,-23.5013279450334,
174.502758507842));
#15069=CARTESIAN_POINT('Ctrl Pts',(-51.4766740890821,-23.4736078700863,
175.190881305064));
#15070=CARTESIAN_POINT('Ctrl Pts',(-51.5715098854918,-23.2578265151817,
176.631332013987));
#15071=CARTESIAN_POINT('Ctrl Pts',(-51.2026984232359,-23.0689810535093,
177.353708555585));
#15072=CARTESIAN_POINT('Ctrl Pts',(-50.0169981786826,-22.6055963153184,
178.072791197941));
#15073=CARTESIAN_POINT('Ctrl Pts',(-49.2289032454779,-22.3364394885883,
178.054791801573));
#15074=CARTESIAN_POINT('Ctrl Pts',(-48.0752306219957,-21.8785657833076,
177.283552800795));
#15075=CARTESIAN_POINT('Ctrl Pts',(-47.7373875210752,-21.6968802590999,
176.548566639058));
#15076=CARTESIAN_POINT('Ctrl Pts',(-47.8901343487967,-21.492320838371,175.113663385513));
#15077=CARTESIAN_POINT('Ctrl Pts',(-48.3804128007365,-21.4693940830233,
174.442825661914));
#15078=CARTESIAN_POINT('Ctrl Pts',(-49.7230759786915,-21.4942443138953,
173.870938911605));
#15079=CARTESIAN_POINT('Ctrl Pts',(-50.5477501626655,-21.53554466513,173.979304242753));
#15080=CARTESIAN_POINT('Ctrl Pts',(-51.6956775721548,-21.5221965965903,
174.884495307656));
#15081=CARTESIAN_POINT('Ctrl Pts',(-51.995185395164,-21.4627711751308,175.65946330393));
#15082=CARTESIAN_POINT('Ctrl Pts',(-51.7684808698132,-21.1836626405178,
177.075777271268));
#15083=CARTESIAN_POINT('Ctrl Pts',(-51.248410167092,-20.9668436684778,177.683928269078));
#15084=CARTESIAN_POINT('Ctrl Pts',(-49.9393032270381,-20.4803392816045,
178.101596183419));
#15085=CARTESIAN_POINT('Ctrl Pts',(-49.1773119956809,-20.2159303489599,
177.900701030808));
#15086=CARTESIAN_POINT('Ctrl Pts',(-48.2258296454727,-19.7984008812386,
176.875814996871));
#15087=CARTESIAN_POINT('Ctrl Pts',(-48.0552229745052,-19.6477554978605,
176.074637438704));
#15088=CARTESIAN_POINT('Ctrl Pts',(-48.5258258225559,-19.5038059294262,
174.698094313544));
#15089=CARTESIAN_POINT('Ctrl Pts',(-49.1555523948045,-19.5080820109078,
174.15313676254));
#15090=CARTESIAN_POINT('Ctrl Pts',(-50.5933891726929,-19.5499376382275,
173.895161972129));
#15091=CARTESIAN_POINT('Ctrl Pts',(-51.368058411907,-19.5828296420673,174.188177381599));
#15092=CARTESIAN_POINT('Ctrl Pts',(-52.285250485287,-19.5255903568737,175.320127767442));
#15093=CARTESIAN_POINT('Ctrl Pts',(-52.4079017329002,-19.4317611692977,
176.136959370172));
#15094=CARTESIAN_POINT('Ctrl Pts',(-51.8753008807154,-19.0950488584311,
177.453114298066));
#15095=CARTESIAN_POINT('Ctrl Pts',(-51.2342686483785,-18.8536936439763,
177.926872571079));
#15096=CARTESIAN_POINT('Ctrl Pts',(-49.8632157867063,-18.3545541183897,
178.021760725256));
#15097=CARTESIAN_POINT('Ctrl Pts',(-49.1660096364335,-18.1030331017558,
177.643137201611));
#15098=CARTESIAN_POINT('Ctrl Pts',(-48.4670297183309,-17.7327410070788,
176.413682699456));
#15099=CARTESIAN_POINT('Ctrl Pts',(-48.483334940274,-17.6194284897493,175.592916154309));
#15100=CARTESIAN_POINT('Ctrl Pts',(-49.2450668681383,-17.5322013902257,
174.352697167155));
#15101=CARTESIAN_POINT('Ctrl Pts',(-49.9777722871607,-17.5559821453049,
173.960304681794));
#15102=CARTESIAN_POINT('Ctrl Pts',(-51.4344516507071,-17.6029063882428,
174.028937019837));
#15103=CARTESIAN_POINT('Ctrl Pts',(-52.1305828574604,-17.6193975644539,
174.485906049309));
#15104=CARTESIAN_POINT('Ctrl Pts',(-52.774838706301,-17.5089074046146,175.793694056009));
#15105=CARTESIAN_POINT('Ctrl Pts',(-52.7115258732458,-17.3796686755426,
176.613178448276));
#15106=CARTESIAN_POINT('Ctrl Pts',(-51.9002446822929,-16.9876585431162,
177.764926590858));
#15107=CARTESIAN_POINT('Ctrl Pts',(-51.1728057089079,-16.7309097600974,
178.068009087089));
#15108=CARTESIAN_POINT('Ctrl Pts',(-49.8211348979667,-16.2361848829689,
177.837068581403));
#15109=CARTESIAN_POINT('Ctrl Pts',(-49.2256314668982,-16.0038069200319,
177.305047152795));
#15110=CARTESIAN_POINT('Ctrl Pts',(-48.8186328386387,-15.691330495564,175.939125806104));
#15111=CARTESIAN_POINT('Ctrl Pts',(-49.013546517339,-15.6112127223192,175.133605172695));
#15112=CARTESIAN_POINT('Ctrl Pts',(-50.0357499087345,-15.5735396207079,
174.088389632472));
#15113=CARTESIAN_POINT('Ctrl Pts',(-50.8379174497137,-15.6112366284576,
173.871670522767));
#15114=CARTESIAN_POINT('Ctrl Pts',(-52.2457834487726,-15.6472027358935,
174.26447248136));
#15115=CARTESIAN_POINT('Ctrl Pts',(-52.8170337247495,-15.6408479370702,
174.8653310014));
#15116=CARTESIAN_POINT('Ctrl Pts',(-53.1560440051794,-15.4721566908598,
176.273031298879));
#15117=CARTESIAN_POINT('Ctrl Pts',(-52.9154253174859,-15.3082073561117,
177.052126824288));
#15118=CARTESIAN_POINT('Ctrl Pts',(-51.8728096300678,-14.8731360568539,
177.975770830197));
#15119=CARTESIAN_POINT('Ctrl Pts',(-51.0951645133176,-14.6055143185424,
178.104087436367));
#15120=CARTESIAN_POINT('Ctrl Pts',(-49.8271933090145,-14.1262171391814,
177.555333624295));
#15121=CARTESIAN_POINT('Ctrl Pts',(-49.3671436709228,-13.9204374671742,
176.893150416479));
#15122=CARTESIAN_POINT('Ctrl Pts',(-49.274728926638,-13.6672296225191,175.457007277905));
#15123=CARTESIAN_POINT('Ctrl Pts',(-49.6465886024413,-13.6223148063404,
174.716642572685));
#15124=CARTESIAN_POINT('Ctrl Pts',(-50.8704338551746,-13.6242867085274,
173.925061362222));
#15125=CARTESIAN_POINT('Ctrl Pts',(-51.7000786840932,-13.666773744136,173.890948850678));
#15126=CARTESIAN_POINT('Ctrl Pts',(-52.983493848767,-13.6801901085456,174.58610021153));
#15127=CARTESIAN_POINT('Ctrl Pts',(-53.4130967944053,-13.6453172862449,
175.298527478907));
#15128=CARTESIAN_POINT('Ctrl Pts',(-53.4312271360186,-13.4141834163833,
176.741466379681));
#15129=CARTESIAN_POINT('Ctrl Pts',(-53.0223631213944,-13.2182197961852,
177.439586265974));
#15130=CARTESIAN_POINT('Ctrl Pts',(-51.8015717929752,-12.7473718779738,
178.090703687822));
#15131=CARTESIAN_POINT('Ctrl Pts',(-51.0193050555008,-12.4800112867217,
178.027617006182));
#15132=CARTESIAN_POINT('Ctrl Pts',(-49.9091230827754,-12.0317475039094,
177.194798446979));
#15133=CARTESIAN_POINT('Ctrl Pts',(-49.6065982226317,-11.8558917537395,
176.440442987632));
#15134=CARTESIAN_POINT('Ctrl Pts',(-49.8356019855053,-11.6660764580159,
175.012059004046));
#15135=CARTESIAN_POINT('Ctrl Pts',(-50.3610430198266,-11.6496605652263,
174.366149315963));
#15136=CARTESIAN_POINT('Ctrl Pts',(-51.7343806490719,-11.6797988495863,
173.866104995302));
#15137=CARTESIAN_POINT('Ctrl Pts',(-52.550540790582,-11.7201981252995,174.02088411371));
#15138=CARTESIAN_POINT('Ctrl Pts',(-53.6500640270725,-11.6966559909963,
174.984749041133));
#15139=CARTESIAN_POINT('Ctrl Pts',(-53.9056865612328,-11.6294298688172,
175.770695352483));
#15140=CARTESIAN_POINT('Ctrl Pts',(-53.6065172861421,-11.3376692947806,
177.167270913611));
#15141=CARTESIAN_POINT('Ctrl Pts',(-53.0559160748103,-11.1139055956972,
177.749439639131));
#15142=CARTESIAN_POINT('Ctrl Pts',(-51.7252371686403,-10.6233177496803,
178.092170345976));
#15143=CARTESIAN_POINT('Ctrl Pts',(-50.9736524019596,-10.3607126008384,
177.849203208466));
#15144=CARTESIAN_POINT('Ctrl Pts',(-50.0765013772471,-9.95292884744916,
176.76875224789));
#15145=CARTESIAN_POINT('Ctrl Pts',(-49.9516819265813,-9.81183425780667,
175.958513771998));
#15146=CARTESIAN_POINT('Ctrl Pts',(-50.4932223958658,-9.68088414604229,
174.607725553029));
#15147=CARTESIAN_POINT('Ctrl Pts',(-51.1493491071183,-9.69075789692425,
174.099564788001));
#15148=CARTESIAN_POINT('Ctrl Pts',(-52.5949212007306,-9.73546275490891,
173.917493057606));
#15149=CARTESIAN_POINT('Ctrl Pts',(-53.3569613223681,-9.76490646019358,
174.248860303054));
#15150=CARTESIAN_POINT('Ctrl Pts',(-54.2135986647274,-9.69602761498083,
175.428657754819));
#15151=CARTESIAN_POINT('Ctrl Pts',(-54.293848370144,-9.59379233086061,176.251060243097));
#15152=CARTESIAN_POINT('Ctrl Pts',(-53.6913007216372,-9.24298063305673,
177.535379997424));
#15153=CARTESIAN_POINT('Ctrl Pts',(-53.0251793740895,-8.99747173235245,
177.96924977839));
#15154=CARTESIAN_POINT('Ctrl Pts',(-51.651725273033,-8.49712492600163,177.987723094373));
#15155=CARTESIAN_POINT('Ctrl Pts',(-50.9786512815054,-8.25081939601668,
177.570771429869));
#15156=CARTESIAN_POINT('Ctrl Pts',(-50.3458167934762,-7.89459730610716,
176.305935969218));
#15157=CARTESIAN_POINT('Ctrl Pts',(-50.4021522245058,-7.78795543802409,
175.483191418641));
#15158=CARTESIAN_POINT('Ctrl Pts',(-51.2295886328818,-7.71347110197539,
174.283262770515));
#15159=CARTESIAN_POINT('Ctrl Pts',(-51.9823539758956,-7.74096536711586,
173.929068927273));
#15160=CARTESIAN_POINT('Ctrl Pts',(-53.4363603166253,-7.78662015021704,
174.075813689628));
#15161=CARTESIAN_POINT('Ctrl Pts',(-54.1043459363082,-7.79847651244032,
174.570723179108));
#15162=CARTESIAN_POINT('Ctrl Pts',(-54.6799658608561,-7.67397811007903,
175.90877571489));
#15163=CARTESIAN_POINT('Ctrl Pts',(-54.5722464428634,-7.53659878310187,
176.719948913595));
#15164=CARTESIAN_POINT('Ctrl Pts',(-53.7048106882453,-7.13527023180301,
177.820508243663));
#15165=CARTESIAN_POINT('Ctrl Pts',(-52.9613211614002,-6.87434685741961,
178.086941994317));
#15166=CARTESIAN_POINT('Ctrl Pts',(-51.6221407922901,-6.38201846097514,
177.778890662373));
#15167=CARTESIAN_POINT('Ctrl Pts',(-51.0546870579556,-6.15491662175662,
177.213869145202));
#15168=CARTESIAN_POINT('Ctrl Pts',(-50.7203127232504,-5.85585141799114,
175.823263107997));
#15169=CARTESIAN_POINT('Ctrl Pts',(-50.9602054908589,-5.78500310757108,
175.029480964866));
#15170=CARTESIAN_POINT('Ctrl Pts',(-52.0343424634976,-5.75674450428783,
174.039165918607));
#15171=CARTESIAN_POINT('Ctrl Pts',(-52.8447329543179,-5.79646505952858,
173.866867743832));
#15172=CARTESIAN_POINT('Ctrl Pts',(-54.227093102642,-5.82880399980787,174.331684606762));
#15173=CARTESIAN_POINT('Ctrl Pts',(-54.7703330160768,-5.81603743040407,
174.961265757845));
#15174=CARTESIAN_POINT('Ctrl Pts',(-55.0342584322448,-5.63295034503888,
176.384531023624));
#15175=CARTESIAN_POINT('Ctrl Pts',(-54.7535167216846,-5.46110103683509,
177.149304158576));
#15176=CARTESIAN_POINT('Ctrl Pts',(-53.6617191466184,-5.01587299208642,
178.013397713687));
#15177=CARTESIAN_POINT('Ctrl Pts',(-52.8789563910228,-4.7479816344422,178.094733745787));
#15178=CARTESIAN_POINT('Ctrl Pts',(-51.6416463903481,-4.27383996939189,
177.476508505419));
#15179=CARTESIAN_POINT('Ctrl Pts',(-51.2194660036301,-4.07584859930261,
176.790317421121));
#15180=CARTESIAN_POINT('Ctrl Pts',(-51.2019938075703,-3.83837584139065,
175.351935740118));
#15181=CARTESIAN_POINT('Ctrl Pts',(-51.610208243602,-3.79954787084599,174.628251672824));
#15182=CARTESIAN_POINT('Ctrl Pts',(-52.8762543405249,-3.80961476365013,
173.901884637809));
#15183=CARTESIAN_POINT('Ctrl Pts',(-53.7073988028502,-3.85223555101975,
173.911595161346));
#15184=CARTESIAN_POINT('Ctrl Pts',(-54.9534921954892,-3.85792953287916,
174.67446559102));
#15185=CARTESIAN_POINT('Ctrl Pts',(-55.3426629917145,-3.81570008082077,
175.409213860003));
#15186=CARTESIAN_POINT('Ctrl Pts',(-55.3039033258818,-3.64772468214507,
176.391662012851));
#15187=CARTESIAN_POINT('Ctrl Pts',(-55.240555748585,-3.59330136077634,176.648581151648));
#15188=CARTESIAN_POINT('Ctrl Pts',(-55.0788320999402,-3.49759375703432,
177.001372563377));
#15189=CARTESIAN_POINT('Ctrl Pts',(-55.0131335998823,-3.46357400887706,
177.112553347482));
#15190=CARTESIAN_POINT('Ctrl Pts',(-54.8999581434668,-3.40984365170443,
177.267014142137));
#15191=CARTESIAN_POINT('Ctrl Pts',(-54.8598034384417,-3.39148030846876,
177.316464483235));
#15192=CARTESIAN_POINT('Ctrl Pts',(-54.7750771562006,-3.35389509449369,
177.410924972696));
#15193=CARTESIAN_POINT('Ctrl Pts',(-54.7397209311609,-3.33918794957438,
177.445275075635));
#15194=CARTESIAN_POINT('Ctrl Pts',(-54.6838989306507,-3.31503673670408,
177.498541333932));
#15195=CARTESIAN_POINT('Ctrl Pts',(-50.3479071748434,-28.4569951884828,
177.87862115707));
#15196=CARTESIAN_POINT('Ctrl Pts',(-50.2728575672733,-28.4359962578257,
177.948540001849));
#15197=CARTESIAN_POINT('Ctrl Pts',(-50.1962258409275,-28.4010191615162,
178.021251708215));
#15198=CARTESIAN_POINT('Ctrl Pts',(-50.0327133344336,-28.3431284715803,
178.148112768101));
#15199=CARTESIAN_POINT('Ctrl Pts',(-49.9471957757512,-28.3135226108735,
178.206264690109));
#15200=CARTESIAN_POINT('Ctrl Pts',(-49.6807194301921,-28.2224721023673,
178.364232700982));
#15201=CARTESIAN_POINT('Ctrl Pts',(-49.4886308694229,-28.1579103591893,
178.447943211646));
#15202=CARTESIAN_POINT('Ctrl Pts',(-48.8935956196606,-27.9633647516093,
178.618732735728));
#15203=CARTESIAN_POINT('Ctrl Pts',(-48.4698811368596,-27.8285932845993,
178.628088311833));
#15204=CARTESIAN_POINT('Ctrl Pts',(-47.2704244122812,-27.4388125604887,
178.343093993075));
#15205=CARTESIAN_POINT('Ctrl Pts',(-46.5780488855805,-27.1997688494767,
177.716319207522));
#15206=CARTESIAN_POINT('Ctrl Pts',(-46.0180477417519,-26.8743979377982,
176.099249510754));
#15207=CARTESIAN_POINT('Ctrl Pts',(-46.162624656611,-26.7973830650002,175.153557109113));
#15208=CARTESIAN_POINT('Ctrl Pts',(-47.1953010051746,-26.7839304768722,
173.755742992678));
#15209=CARTESIAN_POINT('Ctrl Pts',(-48.0607153645256,-26.8454387863112,
173.337748493251));
#15210=CARTESIAN_POINT('Ctrl Pts',(-49.7936242958811,-26.9626978867657,
173.412243144396));
#15211=CARTESIAN_POINT('Ctrl Pts',(-50.6218862360795,-27.016572452629,173.905326198308));
#15212=CARTESIAN_POINT('Ctrl Pts',(-51.5258205855669,-26.9805930176338,
175.367177784907));
#15213=CARTESIAN_POINT('Ctrl Pts',(-51.5951438365624,-26.8874613833773,
176.329869003407));
#15214=CARTESIAN_POINT('Ctrl Pts',(-50.9127162462792,-26.5399486517808,
177.882574589842));
#15215=CARTESIAN_POINT('Ctrl Pts',(-50.1707795944383,-26.2907274748939,
178.452449051012));
#15216=CARTESIAN_POINT('Ctrl Pts',(-48.5397246316051,-25.7645038790956,
178.692502082553));
#15217=CARTESIAN_POINT('Ctrl Pts',(-47.67260524551,-25.4913101058597,178.361691922331));
#15218=CARTESIAN_POINT('Ctrl Pts',(-46.5924693917267,-25.0662449204663,
177.069022085109));
#15219=CARTESIAN_POINT('Ctrl Pts',(-46.3991806471167,-24.9234731673228,
176.136653590829));
#15220=CARTESIAN_POINT('Ctrl Pts',(-46.8738389297659,-24.8040321200569,
174.482872284355));
#15221=CARTESIAN_POINT('Ctrl Pts',(-47.5355683392896,-24.8259889159373,
173.783025779917));
#15222=CARTESIAN_POINT('Ctrl Pts',(-49.181078144729,-24.926602323961,173.233424036193));
#15223=CARTESIAN_POINT('Ctrl Pts',(-50.130455303743,-25.0037631556439,173.398086820976));
#15224=CARTESIAN_POINT('Ctrl Pts',(-51.4978889309697,-25.0558147041254,
174.456799989093));
#15225=CARTESIAN_POINT('Ctrl Pts',(-51.8989353348306,-25.0272033256972,
175.336539369917));
#15226=CARTESIAN_POINT('Ctrl Pts',(-51.8018863283238,-24.7915666340119,
177.05629857501));
#15227=CARTESIAN_POINT('Ctrl Pts',(-51.3095767986978,-24.5911935663349,
177.858613821852));
#15228=CARTESIAN_POINT('Ctrl Pts',(-49.8771546536489,-24.10401978861,178.68604557473));
#15229=CARTESIAN_POINT('Ctrl Pts',(-48.9560458718938,-23.8206956072764,
178.700341600297));
#15230=CARTESIAN_POINT('Ctrl Pts',(-47.4944002604164,-23.3221357921539,
177.903717692127));
#15231=CARTESIAN_POINT('Ctrl Pts',(-46.9859140286074,-23.1182050059858,
177.107706307993));
#15232=CARTESIAN_POINT('Ctrl Pts',(-46.8530474021693,-22.8809089149922,
175.398792520737));
#15233=CARTESIAN_POINT('Ctrl Pts',(-47.231059536602,-22.8477944049951,174.508609012772));
#15234=CARTESIAN_POINT('Ctrl Pts',(-48.6493873331158,-22.8937567040743,
173.363150661036));
#15235=CARTESIAN_POINT('Ctrl Pts',(-49.7143921444323,-22.9840542321675,
173.211662996139));
#15236=CARTESIAN_POINT('Ctrl Pts',(-51.4652368913311,-23.0881428692961,
173.941607840096));
#15237=CARTESIAN_POINT('Ctrl Pts',(-52.1136094605607,-23.094525291844,174.813935779811));
#15238=CARTESIAN_POINT('Ctrl Pts',(-52.3204663109761,-22.9019098705719,
176.69350767169));
#15239=CARTESIAN_POINT('Ctrl Pts',(-51.877821743202,-22.6977464609932,177.66752824204));
#15240=CARTESIAN_POINT('Ctrl Pts',(-50.3601753662095,-22.1706433373772,
178.693383453661));
#15241=CARTESIAN_POINT('Ctrl Pts',(-49.3218325614145,-21.8547798388568,
178.72781114664));
#15242=CARTESIAN_POINT('Ctrl Pts',(-47.7441093775104,-21.3120724766084,
177.795709587611));
#15243=CARTESIAN_POINT('Ctrl Pts',(-47.2477760409393,-21.1012761066736,
176.860414332907));
#15244=CARTESIAN_POINT('Ctrl Pts',(-47.3387825873497,-20.8852685243919,
174.97505816188));
#15245=CARTESIAN_POINT('Ctrl Pts',(-47.9314309575524,-20.8809046965219,
174.063915635121));
#15246=CARTESIAN_POINT('Ctrl Pts',(-49.6347357453554,-20.9768646680186,
173.225964829082));
#15247=CARTESIAN_POINT('Ctrl Pts',(-50.7167240875825,-21.0667038014875,
173.313184970442));
#15248=CARTESIAN_POINT('Ctrl Pts',(-52.2657610285106,-21.1310010461024,
174.421840220958));
#15249=CARTESIAN_POINT('Ctrl Pts',(-52.7037384700293,-21.0998274566763,
175.41493210957));
#15250=CARTESIAN_POINT('Ctrl Pts',(-52.4847175837037,-20.8191405044519,
177.292562937125));
#15251=CARTESIAN_POINT('Ctrl Pts',(-51.8386241308113,-20.5794725658491,
178.12361350116));
#15252=CARTESIAN_POINT('Ctrl Pts',(-50.1396663396365,-20.018246073474,178.763454537015));
#15253=CARTESIAN_POINT('Ctrl Pts',(-49.1209540205185,-19.7031542981699,
178.552891694314));
#15254=CARTESIAN_POINT('Ctrl Pts',(-47.794702927651,-19.2149188701855,177.282197399313));
#15255=CARTESIAN_POINT('Ctrl Pts',(-47.5115450575125,-19.0414866308731,
176.244710688925));
#15256=CARTESIAN_POINT('Ctrl Pts',(-48.0225076992042,-18.9056180257745,
174.413639337664));
#15257=CARTESIAN_POINT('Ctrl Pts',(-48.8010517900779,-18.9401402740231,
173.657816206187));
#15258=CARTESIAN_POINT('Ctrl Pts',(-50.6589325202962,-19.0599362479824,
173.225466551806));
#15259=CARTESIAN_POINT('Ctrl Pts',(-51.6828783925415,-19.1423524153639,
173.556811131415));
#15260=CARTESIAN_POINT('Ctrl Pts',(-52.94490571859,-19.1520660317591,174.977944054317));
#15261=CARTESIAN_POINT('Ctrl Pts',(-53.1522316495948,-19.0733891332466,
176.042129261136));
#15262=CARTESIAN_POINT('Ctrl Pts',(-52.5304975170958,-18.7210523123868,
177.802820234119));
#15263=CARTESIAN_POINT('Ctrl Pts',(-51.7144732100097,-18.4448678812944,
178.469420248747));
#15264=CARTESIAN_POINT('Ctrl Pts',(-49.9127782169188,-17.8629843097264,
178.691085462265));
#15265=CARTESIAN_POINT('Ctrl Pts',(-48.9683571282271,-17.5653381811437,
178.247635108413));
#15266=CARTESIAN_POINT('Ctrl Pts',(-47.9579076603942,-17.1319211116872,
176.683402031933));
#15267=CARTESIAN_POINT('Ctrl Pts',(-47.9184077060768,-17.009302655329,175.611974434002));
#15268=CARTESIAN_POINT('Ctrl Pts',(-48.8193204272181,-16.9493687678545,
173.939410793842));
#15269=CARTESIAN_POINT('Ctrl Pts',(-49.7479148095836,-17.0097492793151,
173.377008912436));
#15270=CARTESIAN_POINT('Ctrl Pts',(-51.643208967551,-17.1428193004232,173.368498519432));
#15271=CARTESIAN_POINT('Ctrl Pts',(-52.5796094505093,-17.2045582837911,
173.921665784702));
#15272=CARTESIAN_POINT('Ctrl Pts',(-53.4961681928706,-17.1468816411331,
175.591939966795));
#15273=CARTESIAN_POINT('Ctrl Pts',(-53.4629851797616,-17.024999612415,176.669185388437));
#15274=CARTESIAN_POINT('Ctrl Pts',(-52.4593346223015,-16.5928308404044,
178.238747171052));
#15275=CARTESIAN_POINT('Ctrl Pts',(-51.5224253668316,-16.2971453030902,
178.685547111838));
#15276=CARTESIAN_POINT('Ctrl Pts',(-49.7246467734476,-15.7168449309467,
178.479497386489));
#15277=CARTESIAN_POINT('Ctrl Pts',(-48.9027009029283,-15.4396261238498,
177.823563805929));
#15278=CARTESIAN_POINT('Ctrl Pts',(-48.2654141259822,-15.0843052308904,
176.069175886686));
#15279=CARTESIAN_POINT('Ctrl Pts',(-48.4613159716259,-15.0032908855178,
175.000998038449));
#15280=CARTESIAN_POINT('Ctrl Pts',(-49.7162174501553,-15.01079667333,173.565578406105));
#15281=CARTESIAN_POINT('Ctrl Pts',(-50.7428205977302,-15.0933182852754,
173.226451476554));
#15282=CARTESIAN_POINT('Ctrl Pts',(-52.6035006910652,-15.2135426682566,
173.650512878487));
#15283=CARTESIAN_POINT('Ctrl Pts',(-53.382025542189,-15.2486168447941,174.397702687793));
#15284=CARTESIAN_POINT('Ctrl Pts',(-53.905727267535,-15.1159903036539,176.219573585739));
#15285=CARTESIAN_POINT('Ctrl Pts',(-53.6343010604909,-14.9449274325696,
177.258764585683));
#15286=CARTESIAN_POINT('Ctrl Pts',(-52.3195045847479,-14.4589334435455,
178.541768722646));
#15287=CARTESIAN_POINT('Ctrl Pts',(-51.3015568868895,-14.1438839803641,
178.764698457169));
#15288=CARTESIAN_POINT('Ctrl Pts',(-49.5920248617255,-13.5797433288121,
178.136857041975));
#15289=CARTESIAN_POINT('Ctrl Pts',(-48.9380275082558,-13.3381062047143,
177.30578604004));
#15290=CARTESIAN_POINT('Ctrl Pts',(-48.7105476579708,-13.0557925005452,
175.429441731563));
#15291=CARTESIAN_POINT('Ctrl Pts',(-49.1406103931943,-13.0235604552581,
174.438788862592));
#15292=CARTESIAN_POINT('Ctrl Pts',(-50.6761207099769,-13.0860799668151,
173.321489243126));
#15293=CARTESIAN_POINT('Ctrl Pts',(-51.7550963134731,-13.1754760058423,
173.222308149713));
#15294=CARTESIAN_POINT('Ctrl Pts',(-53.4658619993328,-13.2728668841322,
174.044907498799));
#15295=CARTESIAN_POINT('Ctrl Pts',(-54.0695830139971,-13.2704822339251,
174.951304580462));
#15296=CARTESIAN_POINT('Ctrl Pts',(-54.1756431350045,-13.0566118191168,
176.841599266944));
#15297=CARTESIAN_POINT('Ctrl Pts',(-53.682402379201,-12.8459201272062,177.784941606983));
#15298=CARTESIAN_POINT('Ctrl Pts',(-52.1086906323698,-12.3039548020853,
178.724742549594));
#15299=CARTESIAN_POINT('Ctrl Pts',(-51.0761365726385,-11.9897880340734,
178.697123202695));
#15300=CARTESIAN_POINT('Ctrl Pts',(-49.5543778605173,-11.4626036611189,
177.68675201361));
#15301=CARTESIAN_POINT('Ctrl Pts',(-49.102117382649,-11.2567014833508,176.719561205716));
#15302=CARTESIAN_POINT('Ctrl Pts',(-49.292107286816,-11.0609269687249,174.839303437302));
#15303=CARTESIAN_POINT('Ctrl Pts',(-49.9319808722111,-11.065488255827,173.957841233623));
#15304=CARTESIAN_POINT('Ctrl Pts',(-51.6826661337304,-11.1687038756892,
173.21175444078));
#15305=CARTESIAN_POINT('Ctrl Pts',(-52.7531972098707,-11.2596980870477,
173.357216390535));
#15306=CARTESIAN_POINT('Ctrl Pts',(-54.2460458385202,-11.3089418781751,
174.551734842451));
#15307=CARTESIAN_POINT('Ctrl Pts',(-54.6245671161656,-11.2668768405657,
175.56211463078));
#15308=CARTESIAN_POINT('Ctrl Pts',(-54.3123472668563,-10.9730441873765,
177.413426209709));
#15309=CARTESIAN_POINT('Ctrl Pts',(-53.6216949876352,-10.7211032153202,
178.215314744748));
#15310=CARTESIAN_POINT('Ctrl Pts',(-51.8913746121094,-10.1550133368813,
178.758899998487));
#15311=CARTESIAN_POINT('Ctrl Pts',(-50.8831280746124,-9.84182247697009,
178.493145848044));
#15312=CARTESIAN_POINT('Ctrl Pts',(-49.6236112332636,-9.36447275925141,
177.143870489208));
#15313=CARTESIAN_POINT('Ctrl Pts',(-49.3975849797945,-9.20540142615231,
176.095279478262));
#15314=CARTESIAN_POINT('Ctrl Pts',(-50.0079456983536,-9.08466255147406,
174.288405253537));
#15315=CARTESIAN_POINT('Ctrl Pts',(-50.8244602905949,-9.12692713822202,
173.581609594638));
#15316=CARTESIAN_POINT('Ctrl Pts',(-52.6906598209441,-9.25318698046637,
173.246687842459));
#15317=CARTESIAN_POINT('Ctrl Pts',(-53.7047460872083,-9.33006604421617,
173.631253257821));
#15318=CARTESIAN_POINT('Ctrl Pts',(-54.8900559939021,-9.32613298909108,
175.117109460381));
#15319=CARTESIAN_POINT('Ctrl Pts',(-55.0428852800419,-9.23680213120813,
176.191613835385));
#15320=CARTESIAN_POINT('Ctrl Pts',(-54.3260630027991,-8.86426623816917,
177.917066297754));
#15321=CARTESIAN_POINT('Ctrl Pts',(-53.4783261791472,-8.5852751826903,178.533414961083));
#15322=CARTESIAN_POINT('Ctrl Pts',(-51.6632029807945,-7.99669600625119,
178.652882987613));
#15323=CARTESIAN_POINT('Ctrl Pts',(-50.7499980781025,-7.70554604519678,
178.155739114359));
#15324=CARTESIAN_POINT('Ctrl Pts',(-49.8242259537338,-7.29327695933862,
176.547077701437));
#15325=CARTESIAN_POINT('Ctrl Pts',(-49.838033268214,-7.17726487827271,175.466032067978));
#15326=CARTESIAN_POINT('Ctrl Pts',(-50.8256764893838,-7.13523953214819,
173.842841571287));
#15327=CARTESIAN_POINT('Ctrl Pts',(-51.7828991970818,-7.20106754009712,
173.328393136411));
#15328=CARTESIAN_POINT('Ctrl Pts',(-53.682121466631,-7.33289296119618,173.423267613666));
#15329=CARTESIAN_POINT('Ctrl Pts',(-54.5824458512144,-7.39109185214275,
174.023927494841));
#15330=CARTESIAN_POINT('Ctrl Pts',(-55.4117106483233,-7.31244449093335,
175.744908515432));
#15331=CARTESIAN_POINT('Ctrl Pts',(-55.3174225063257,-7.17911919393448,
176.81298142285));
#15332=CARTESIAN_POINT('Ctrl Pts',(-54.241836216539,-6.73809069114013,178.316074643566));
#15333=CARTESIAN_POINT('Ctrl Pts',(-53.2777666803375,-6.43346338348791,
178.716995563853));
#15334=CARTESIAN_POINT('Ctrl Pts',(-51.492709987459,-5.85671796076922,178.410389321177));
#15335=CARTESIAN_POINT('Ctrl Pts',(-50.7047045568934,-5.58599179870949,
177.709705935534));
#15336=CARTESIAN_POINT('Ctrl Pts',(-50.1611589540997,-5.24690475917716,
175.91572047402));
#15337=CARTESIAN_POINT('Ctrl Pts',(-50.412988668319,-5.17989675417243,174.862537959116));
#15338=CARTESIAN_POINT('Ctrl Pts',(-51.7459369624996,-5.19848686371817,
173.493142781303));
#15339=CARTESIAN_POINT('Ctrl Pts',(-52.7859565461007,-5.28395186106844,
173.214419006065));
#15340=CARTESIAN_POINT('Ctrl Pts',(-54.6124153348595,-5.40237052054082,
173.730440016312));
#15341=CARTESIAN_POINT('Ctrl Pts',(-55.3590089692939,-5.42765093815174,
174.520747942326));
#15342=CARTESIAN_POINT('Ctrl Pts',(-55.7857743262001,-5.27753030569205,
176.366096056906));
#15343=CARTESIAN_POINT('Ctrl Pts',(-55.461398252989,-5.09617167994865,177.38970404608));
#15344=CARTESIAN_POINT('Ctrl Pts',(-54.0763289367501,-4.5947076574371,178.59887213214));
#15345=CARTESIAN_POINT('Ctrl Pts',(-53.0518069694618,-4.2817330879142,178.762764238352));
#15346=CARTESIAN_POINT('Ctrl Pts',(-51.3741810061549,-3.71961935803744,
178.037173193724));
#15347=CARTESIAN_POINT('Ctrl Pts',(-50.7709128345885,-3.48817293681553,
177.171361011829));
#15348=CARTESIAN_POINT('Ctrl Pts',(-50.6389382081356,-3.22905679794207,
175.293151941354));
#15349=CARTESIAN_POINT('Ctrl Pts',(-51.12053621277,-3.20321300476925,174.318272388974));
#15350=CARTESIAN_POINT('Ctrl Pts',(-52.7133196362096,-3.27785561089881,
173.283689189228));
#15351=CARTESIAN_POINT('Ctrl Pts',(-53.7973395798457,-3.36818712000785,
173.24106430149));
#15352=CARTESIAN_POINT('Ctrl Pts',(-55.4653436163453,-3.45546685002776,
174.15674387015));
#15353=CARTESIAN_POINT('Ctrl Pts',(-56.0173052873986,-3.44570666511222,
175.091057375796));
#15354=CARTESIAN_POINT('Ctrl Pts',(-56.0215539606611,-3.28449111210032,
176.384962205932));
#15355=CARTESIAN_POINT('Ctrl Pts',(-55.9545655524391,-3.23079314429921,
176.725242297786));
#15356=CARTESIAN_POINT('Ctrl Pts',(-55.7610730366685,-3.12770940060629,
177.200137919422));
#15357=CARTESIAN_POINT('Ctrl Pts',(-55.6813772878146,-3.09105284269064,
177.349953976371));
#15358=CARTESIAN_POINT('Ctrl Pts',(-55.542047034587,-3.0325075684579,177.559861392858));
#15359=CARTESIAN_POINT('Ctrl Pts',(-55.4922962422521,-3.01237854056411,
177.627368088468));
#15360=CARTESIAN_POINT('Ctrl Pts',(-55.3864710916189,-2.97076694703694,
177.757099244203));
#15361=CARTESIAN_POINT('Ctrl Pts',(-55.3343400650611,-2.9517036220202,177.814670571915));
#15362=CARTESIAN_POINT('Ctrl Pts',(-55.2712257966423,-2.92704897744562,
177.878689530232));
#15363=CARTESIAN_POINT('Ctrl Pts',(-50.193114320713,-27.8005016688432,177.448440461337));
#15364=CARTESIAN_POINT('Ctrl Pts',(-50.1356777281885,-27.7780416249781,
177.514251363723));
#15365=CARTESIAN_POINT('Ctrl Pts',(-50.0768656935625,-27.751543311514,177.569181845458));
#15366=CARTESIAN_POINT('Ctrl Pts',(-49.9502510673185,-27.7006718917524,
177.678131488152));
#15367=CARTESIAN_POINT('Ctrl Pts',(-49.8836384545372,-27.6746069642733,
177.728584647058));
#15368=CARTESIAN_POINT('Ctrl Pts',(-49.6751767137455,-27.5945945456976,
177.866776279515));
#15369=CARTESIAN_POINT('Ctrl Pts',(-49.5241175159801,-27.5384622401806,
177.941191651987));
#15370=CARTESIAN_POINT('Ctrl Pts',(-49.052722448706,-27.3677108924734,178.102046365205));
#15371=CARTESIAN_POINT('Ctrl Pts',(-48.713006227557,-27.2491092781452,178.126053652285));
#15372=CARTESIAN_POINT('Ctrl Pts',(-47.7382795874562,-26.9019657740439,
177.942209528285));
#15373=CARTESIAN_POINT('Ctrl Pts',(-47.1597470877608,-26.6842880122364,
177.461567693823));
#15374=CARTESIAN_POINT('Ctrl Pts',(-46.658904710499,-26.3725604903201,176.179580952166));
#15375=CARTESIAN_POINT('Ctrl Pts',(-46.744016732095,-26.2835354545934,175.410971277798));
#15376=CARTESIAN_POINT('Ctrl Pts',(-47.5354179070377,-26.2224078706935,
174.242909311213));
#15377=CARTESIAN_POINT('Ctrl Pts',(-48.2245449656354,-26.2493771368743,
173.87343933243));
#15378=CARTESIAN_POINT('Ctrl Pts',(-49.6317089464608,-26.3060463238627,
173.871895146128));
#15379=CARTESIAN_POINT('Ctrl Pts',(-50.3230600395606,-26.332977077053,174.238655026377));
#15380=CARTESIAN_POINT('Ctrl Pts',(-51.1153496063116,-26.2743348509258,
175.387691644257));
#15381=CARTESIAN_POINT('Ctrl Pts',(-51.2096393582444,-26.1855070701005,
176.164686974611));
#15382=CARTESIAN_POINT('Ctrl Pts',(-50.7213268039385,-25.8775623946772,
177.442968877094));
#15383=CARTESIAN_POINT('Ctrl Pts',(-50.1473617008829,-25.6602454668112,
177.932812658479));
#15384=CARTESIAN_POINT('Ctrl Pts',(-48.8451246534299,-25.1962898596545,
178.190564242377));
#15385=CARTESIAN_POINT('Ctrl Pts',(-48.1356293396501,-24.9529458243571,
177.955714348281));
#15386=CARTESIAN_POINT('Ctrl Pts',(-47.2268076672755,-24.5631416907191,
176.954286183848));
#15387=CARTESIAN_POINT('Ctrl Pts',(-47.0395646158613,-24.4209960169422,
176.20954077848));
#15388=CARTESIAN_POINT('Ctrl Pts',(-47.370313215787,-24.2726666068476,174.855768290097));
#15389=CARTESIAN_POINT('Ctrl Pts',(-47.8845545017147,-24.265674947158,174.26583855031));
#15390=CARTESIAN_POINT('Ctrl Pts',(-49.1994460468846,-24.3046603227726,
173.764180115318));
#15391=CARTESIAN_POINT('Ctrl Pts',(-49.9762257647407,-24.3480555327739,
173.861039734223));
#15392=CARTESIAN_POINT('Ctrl Pts',(-51.1285193941288,-24.3574791486806,
174.66646218052));
#15393=CARTESIAN_POINT('Ctrl Pts',(-51.4882290443068,-24.3203491702665,
175.364132112564));
#15394=CARTESIAN_POINT('Ctrl Pts',(-51.4777341832408,-24.1036300286494,
176.755680066459));
#15395=CARTESIAN_POINT('Ctrl Pts',(-51.1141102527119,-23.9275319100486,
177.423612084264));
#15396=CARTESIAN_POINT('Ctrl Pts',(-49.9940329966114,-23.4994535030053,
178.148719290634));
#15397=CARTESIAN_POINT('Ctrl Pts',(-49.2531996565364,-23.2503850964097,
178.195074921104));
#15398=CARTESIAN_POINT('Ctrl Pts',(-48.0540724826088,-22.804580182732,177.607487959387));
#15399=CARTESIAN_POINT('Ctrl Pts',(-47.6174629086983,-22.6140260251447,
176.985139741962));
#15400=CARTESIAN_POINT('Ctrl Pts',(-47.4549919432363,-22.3698803060775,
175.609945370482));
#15401=CARTESIAN_POINT('Ctrl Pts',(-47.7329522193418,-22.3169255939418,
174.876470615888));
#15402=CARTESIAN_POINT('Ctrl Pts',(-48.8440385240951,-22.3059754149369,
173.902867041218));
#15403=CARTESIAN_POINT('Ctrl Pts',(-49.7035599970344,-22.3554674780819,
173.739637329099));
#15404=CARTESIAN_POINT('Ctrl Pts',(-51.1531706356154,-22.4011313967338,
174.265066374312));
#15405=CARTESIAN_POINT('Ctrl Pts',(-51.7115054154064,-22.3910761212842,
174.945624054023));
#15406=CARTESIAN_POINT('Ctrl Pts',(-51.9563259347572,-22.2045289991918,
176.459132103654));
#15407=CARTESIAN_POINT('Ctrl Pts',(-51.63765119649,-22.0251559400258,177.262331468575));
#15408=CARTESIAN_POINT('Ctrl Pts',(-50.4571461815608,-21.5627984935069,
178.149907937338));
#15409=CARTESIAN_POINT('Ctrl Pts',(-49.6222512854117,-21.2849471395443,
178.217719280236));
#15410=CARTESIAN_POINT('Ctrl Pts',(-48.3256452005116,-20.7988977065915,
177.525255091295));
#15411=CARTESIAN_POINT('Ctrl Pts',(-47.8935170509031,-20.5993012814682,
176.78942555283));
#15412=CARTESIAN_POINT('Ctrl Pts',(-47.9069259765589,-20.3679964193449,
175.264267840625));
#15413=CARTESIAN_POINT('Ctrl Pts',(-48.3565963500671,-20.33698501403,174.508050023486));
#15414=CARTESIAN_POINT('Ctrl Pts',(-49.7115395236169,-20.3645147337819,
173.767258025586));
#15415=CARTESIAN_POINT('Ctrl Pts',(-50.5919963646361,-20.4163759449694,
173.798730113887));
#15416=CARTESIAN_POINT('Ctrl Pts',(-51.8921615926268,-20.4324111199544,
174.637786957993));
#15417=CARTESIAN_POINT('Ctrl Pts',(-52.2870845316673,-20.391715494119,175.425932171935));
#15418=CARTESIAN_POINT('Ctrl Pts',(-52.1845249551972,-20.1359343420921,
176.949348485014));
#15419=CARTESIAN_POINT('Ctrl Pts',(-51.6978717551623,-19.9258306519252,
177.647217385389));
#15420=CARTESIAN_POINT('Ctrl Pts',(-50.3567743114224,-19.4332812849397,
178.229888643815));
#15421=CARTESIAN_POINT('Ctrl Pts',(-49.531482093434,-19.1564117811874,178.098575810452));
#15422=CARTESIAN_POINT('Ctrl Pts',(-48.4209526978951,-18.7085233315365,
177.123331466978));
#15423=CARTESIAN_POINT('Ctrl Pts',(-48.1597795720535,-18.5402167412103,
176.29718764283));
#15424=CARTESIAN_POINT('Ctrl Pts',(-48.5145782694716,-18.3739619700934,
174.800216258582));
#15425=CARTESIAN_POINT('Ctrl Pts',(-49.1216168980297,-18.3741927637648,
174.159897255644));
#15426=CARTESIAN_POINT('Ctrl Pts',(-50.6124880467131,-18.4256628314289,
173.74530968569));
#15427=CARTESIAN_POINT('Ctrl Pts',(-51.4570089590119,-18.472296203581,173.973986288395));
#15428=CARTESIAN_POINT('Ctrl Pts',(-52.5367755134872,-18.4465314340497,
175.076321400051));
#15429=CARTESIAN_POINT('Ctrl Pts',(-52.7461464663159,-18.3691716102472,
175.928004990245));
#15430=CARTESIAN_POINT('Ctrl Pts',(-52.3166330239091,-18.0526500335514,
177.376965544067));
#15431=CARTESIAN_POINT('Ctrl Pts',(-51.6857211698905,-17.8130496454,177.945754508989));
#15432=CARTESIAN_POINT('Ctrl Pts',(-50.2465394893753,-17.3007990625156,
178.194297846636));
#15433=CARTESIAN_POINT('Ctrl Pts',(-49.4703000985441,-17.0343670318334,
177.871754882023));
#15434=CARTESIAN_POINT('Ctrl Pts',(-48.6088763818932,-16.6321365971318,
176.648991214725));
#15435=CARTESIAN_POINT('Ctrl Pts',(-48.5409020769561,-16.5028432711256,
175.78526591443));
#15436=CARTESIAN_POINT('Ctrl Pts',(-49.2164515058916,-16.3991203888251,
174.401518908745));
#15437=CARTESIAN_POINT('Ctrl Pts',(-49.9496118192587,-16.4227354715302,
173.914202886417));
#15438=CARTESIAN_POINT('Ctrl Pts',(-51.4902606534728,-16.4861638259448,
173.836744887307));
#15439=CARTESIAN_POINT('Ctrl Pts',(-52.2697075969923,-16.5185243960147,
174.249627738192));
#15440=CARTESIAN_POINT('Ctrl Pts',(-53.0792623986938,-16.4399376212412,
175.566241461313));
#15441=CARTESIAN_POINT('Ctrl Pts',(-53.0958608617722,-16.3264383488088,
176.440260240546));
#15442=CARTESIAN_POINT('Ctrl Pts',(-52.3498924896565,-15.9464100326616,
177.743856795072));
#15443=CARTESIAN_POINT('Ctrl Pts',(-51.6136771994172,-15.6882407493956,
178.142477224647));
#15444=CARTESIAN_POINT('Ctrl Pts',(-50.1619939854693,-15.1743526813971,
178.045393567771));
#15445=CARTESIAN_POINT('Ctrl Pts',(-49.479535393056,-14.9249532161513,177.547481856475));
#15446=CARTESIAN_POINT('Ctrl Pts',(-48.9083003859244,-14.5811172796918,
176.154888290848));
#15447=CARTESIAN_POINT('Ctrl Pts',(-49.032687325759,-14.4872017268269,175.286386043965));
#15448=CARTESIAN_POINT('Ctrl Pts',(-50.002899927607,-14.4395306566209,174.08106638639));
#15449=CARTESIAN_POINT('Ctrl Pts',(-50.8258619899905,-14.4815667576624,
173.768688449528));
#15450=CARTESIAN_POINT('Ctrl Pts',(-52.3490472247602,-14.5391579602322,
174.044477097964));
#15451=CARTESIAN_POINT('Ctrl Pts',(-53.0108480437211,-14.5505369630929,
174.618897762295));
#15452=CARTESIAN_POINT('Ctrl Pts',(-53.508606726061,-14.41258118913,176.072854784516));
#15453=CARTESIAN_POINT('Ctrl Pts',(-53.3308496256547,-14.2605010523332,
176.92211652172));
#15454=CARTESIAN_POINT('Ctrl Pts',(-52.3234046589676,-13.8325238003689,
178.011250192421));
#15455=CARTESIAN_POINT('Ctrl Pts',(-51.5138129382755,-13.5585438056648,
178.229366209696));
#15456=CARTESIAN_POINT('Ctrl Pts',(-50.1182607249297,-13.0546721198729,
177.788098654291));
#15457=CARTESIAN_POINT('Ctrl Pts',(-49.5630188185408,-12.8308644828691,
177.140857971114));
#15458=CARTESIAN_POINT('Ctrl Pts',(-49.3219040202974,-12.5483689245281,
175.637957478437));
#15459=CARTESIAN_POINT('Ctrl Pts',(-49.6365594730894,-12.4926951709364,
174.821179942866));
#15460=CARTESIAN_POINT('Ctrl Pts',(-50.8450351424658,-12.4918253386163,
173.862170041067));
#15461=CARTESIAN_POINT('Ctrl Pts',(-51.7160671936879,-12.5420406725331,
173.742988789581));
#15462=CARTESIAN_POINT('Ctrl Pts',(-53.1380531234061,-12.5824907099911,
174.344563971126));
#15463=CARTESIAN_POINT('Ctrl Pts',(-53.661497991413,-12.565516429584,175.054752397452));
#15464=CARTESIAN_POINT('Ctrl Pts',(-53.8242077932451,-12.3622912981454,
176.579637740953));
#15465=CARTESIAN_POINT('Ctrl Pts',(-53.4635573374974,-12.1759538811977,
177.362604506387));
#15466=CARTESIAN_POINT('Ctrl Pts',(-52.2358756182636,-11.7031645393402,
178.179207046235));
#15467=CARTESIAN_POINT('Ctrl Pts',(-51.404471480006,-11.4266005921062,178.198059647233));
#15468=CARTESIAN_POINT('Ctrl Pts',(-50.1465877134854,-10.9499764840513,
177.440684540534));
#15469=CARTESIAN_POINT('Ctrl Pts',(-49.7512566691313,-10.7559713173261,
176.677961727673));
#15470=CARTESIAN_POINT('Ctrl Pts',(-49.8442980389787,-10.5402489724976,
175.152069846099));
#15471=CARTESIAN_POINT('Ctrl Pts',(-50.3336227209985,-10.5166703329192,
174.417963751365));
#15472=CARTESIAN_POINT('Ctrl Pts',(-51.729412313951,-10.5511670115394,173.750914008412));
#15473=CARTESIAN_POINT('Ctrl Pts',(-52.6055357660183,-10.6034581645062,
173.829125569603));
#15474=CARTESIAN_POINT('Ctrl Pts',(-53.8591972775733,-10.6090268187652,
174.739479897504));
#15475=CARTESIAN_POINT('Ctrl Pts',(-54.2075655427863,-10.559958422732,175.542285446703));
#15476=CARTESIAN_POINT('Ctrl Pts',(-54.0309723767407,-10.2919570312328,
177.05153449857));
#15477=CARTESIAN_POINT('Ctrl Pts',(-53.5065211660476,-10.0729835636969,
177.724885949439));
#15478=CARTESIAN_POINT('Ctrl Pts',(-52.1359327706082,-9.57501150980407,
178.231990439602));
#15479=CARTESIAN_POINT('Ctrl Pts',(-51.3168725161042,-9.29919601638729,
178.055337178134));
#15480=CARTESIAN_POINT('Ctrl Pts',(-50.258716477129,-8.86039345968628,177.014257444883));
#15481=CARTESIAN_POINT('Ctrl Pts',(-50.0419858596938,-8.70190296068798,
176.174822144773));
#15482=CARTESIAN_POINT('Ctrl Pts',(-50.4788136762356,-8.55014763089762,
174.697436550109));
#15483=CARTESIAN_POINT('Ctrl Pts',(-51.1165600370436,-8.55674976323144,
174.095019459488));
#15484=CARTESIAN_POINT('Ctrl Pts',(-52.6206590619166,-8.6128620697194,173.755704628284));
#15485=CARTESIAN_POINT('Ctrl Pts',(-53.456626592603,-8.65630954771657,174.029197443714));
#15486=CARTESIAN_POINT('Ctrl Pts',(-54.4781193003427,-8.6195332279715,175.187078119489));
#15487=CARTESIAN_POINT('Ctrl Pts',(-54.643602443466,-8.53353572012608,176.04949882023));
#15488=CARTESIAN_POINT('Ctrl Pts',(-54.1354947853707,-8.20096498746117,
177.472181687833));
#15489=CARTESIAN_POINT('Ctrl Pts',(-53.4760203027823,-7.95706608118669,
178.003825172765));
#15490=CARTESIAN_POINT('Ctrl Pts',(-52.0249165538012,-7.441132564782,178.167825277993));
#15491=CARTESIAN_POINT('Ctrl Pts',(-51.2723007652614,-7.17976116760829,
177.802466009854));
#15492=CARTESIAN_POINT('Ctrl Pts',(-50.4742318046734,-6.79179686888332,
176.539214575509));
#15493=CARTESIAN_POINT('Ctrl Pts',(-50.4508393849021,-6.66952799804251,
175.667365550039));
#15494=CARTESIAN_POINT('Ctrl Pts',(-51.1982775200671,-6.57992894303025,
174.318931761547));
#15495=CARTESIAN_POINT('Ctrl Pts',(-51.9567203354133,-6.60831910752051,
173.869388776842));
#15496=CARTESIAN_POINT('Ctrl Pts',(-53.5030461170827,-6.67180659392302,
173.876188814802));
#15497=CARTESIAN_POINT('Ctrl Pts',(-54.2579318048227,-6.70074853854407,
174.329266762268));
#15498=CARTESIAN_POINT('Ctrl Pts',(-54.9950541895712,-6.6067812144727,175.688231083653));
#15499=CARTESIAN_POINT('Ctrl Pts',(-54.9633937640365,-6.48434226598442,
176.556150922255));
#15500=CARTESIAN_POINT('Ctrl Pts',(-54.1573516980127,-6.0949735677162,177.812809342709));
#15501=CARTESIAN_POINT('Ctrl Pts',(-53.3979887985791,-5.83073710308303,
178.172806822259));
#15502=CARTESIAN_POINT('Ctrl Pts',(-51.9519097716579,-5.31810666795101,
177.994568269632));
#15503=CARTESIAN_POINT('Ctrl Pts',(-51.2952074816856,-5.0735953089356,177.458800517348));
#15504=CARTESIAN_POINT('Ctrl Pts',(-50.7993635736617,-4.74342220821161,
176.031468409862));
#15505=CARTESIAN_POINT('Ctrl Pts',(-50.9692613848378,-4.65940397939939,
175.170313217647));
#15506=CARTESIAN_POINT('Ctrl Pts',(-52.0040245669764,-4.62293999106357,
174.01934301833));
#15507=CARTESIAN_POINT('Ctrl Pts',(-52.8385688131003,-4.66759138415716,
173.754231358386));
#15508=CARTESIAN_POINT('Ctrl Pts',(-54.3414847379305,-4.72329909029368,
174.103969484305));
#15509=CARTESIAN_POINT('Ctrl Pts',(-54.9761466933045,-4.72791014175074,
174.714716972292));
#15510=CARTESIAN_POINT('Ctrl Pts',(-55.3975165431988,-4.57549651155636,
176.192173272167));
#15511=CARTESIAN_POINT('Ctrl Pts',(-55.1760506072609,-4.4148786220368,177.03103539143));
#15512=CARTESIAN_POINT('Ctrl Pts',(-54.1093043232961,-3.97451188101218,
178.061753391873));
#15513=CARTESIAN_POINT('Ctrl Pts',(-53.2902925544343,-3.69995792969149,
178.233822626392));
#15514=CARTESIAN_POINT('Ctrl Pts',(-51.9203920380846,-3.19963469730891,
177.711493690972));
#15515=CARTESIAN_POINT('Ctrl Pts',(-51.4044324721558,-2.98383265912278,
177.036002564632));
#15516=CARTESIAN_POINT('Ctrl Pts',(-51.237949425703,-2.71774512370317,175.525044339462));
#15517=CARTESIAN_POINT('Ctrl Pts',(-51.5957499271559,-2.66894330374766,
174.721509320474));
#15518=CARTESIAN_POINT('Ctrl Pts',(-52.8541051305037,-2.67783999801612,
173.825937213487));
#15519=CARTESIAN_POINT('Ctrl Pts',(-53.7315999697276,-2.7292086653859,173.7525048498));
#15520=CARTESIAN_POINT('Ctrl Pts',(-55.1208667949195,-2.76252327401043,
174.431246184642));
#15521=CARTESIAN_POINT('Ctrl Pts',(-55.6054709668258,-2.73893798071373,
175.167402226862));
#15522=CARTESIAN_POINT('Ctrl Pts',(-55.6603171863937,-2.58869274068622,
176.211840888345));
#15523=CARTESIAN_POINT('Ctrl Pts',(-55.6210463302226,-2.5392081864434,176.490448482462));
#15524=CARTESIAN_POINT('Ctrl Pts',(-55.4836397365907,-2.4479441182576,176.880586390838));
#15525=CARTESIAN_POINT('Ctrl Pts',(-55.4253285390117,-2.41535251334816,
177.005027857449));
#15526=CARTESIAN_POINT('Ctrl Pts',(-55.321414213033,-2.36345060131236,177.180440236558));
#15527=CARTESIAN_POINT('Ctrl Pts',(-55.2840225057543,-2.34563722905757,
177.23703696138));
#15528=CARTESIAN_POINT('Ctrl Pts',(-55.2039936793606,-2.30896761153951,
177.345998347345));
#15529=CARTESIAN_POINT('Ctrl Pts',(-55.1587206712145,-2.28906361698866,
177.401367187303));
#15530=CARTESIAN_POINT('Ctrl Pts',(-55.1161897096451,-2.27071607222657,
177.448351373365));
#15531=CARTESIAN_POINT('Origin',(-49.8994188116831,-27.9943596339097,177.258277275215));
#15532=CARTESIAN_POINT('Ctrl Pts',(-47.8886718415116,-31.6995536639001,
175.585485069079));
#15533=CARTESIAN_POINT('Ctrl Pts',(-47.9424090991571,-31.4208895534118,
175.585485069079));
#15534=CARTESIAN_POINT('Ctrl Pts',(-48.0165136638412,-31.142217631488,175.587595470504));
#15535=CARTESIAN_POINT('Ctrl Pts',(-48.206190379979,-30.6092681473582,175.5992945923));
#15536=CARTESIAN_POINT('Ctrl Pts',(-48.3219855416571,-30.3543443720961,
175.608895409754));
#15537=CARTESIAN_POINT('Ctrl Pts',(-48.7193595355016,-29.6463117438825,
175.654781597023));
#15538=CARTESIAN_POINT('Ctrl Pts',(-49.0545911241397,-29.252967076522,175.707428551708));
#15539=CARTESIAN_POINT('Ctrl Pts',(-49.5445318563166,-28.7861739714513,
175.852028081795));
#15540=CARTESIAN_POINT('Ctrl Pts',(-49.6987397911889,-28.6436248452838,
175.911397856293));
#15541=CARTESIAN_POINT('Ctrl Pts',(-49.9262155871255,-28.4691236019893,
176.025260422827));
#15542=CARTESIAN_POINT('Ctrl Pts',(-50.0186861454797,-28.4371266816906,
176.06691518842));
#15543=CARTESIAN_POINT('Ctrl Pts',(-50.1842299781189,-28.3689363752761,
176.173317219728));
#15544=CARTESIAN_POINT('Ctrl Pts',(-50.2569026354171,-28.3307458842207,
176.235836425973));
#15545=CARTESIAN_POINT('Ctrl Pts',(-50.4390882192945,-28.20291241382,176.455121758264));
#15546=CARTESIAN_POINT('Ctrl Pts',(-50.5079392950738,-28.0960057551614,
176.657103040121));
#15547=CARTESIAN_POINT('Ctrl Pts',(-50.4672993044493,-27.9634501974094,
176.968869644582));
#15548=CARTESIAN_POINT('Ctrl Pts',(-50.4326818607288,-27.9245995634275,
177.070967051899));
#15549=CARTESIAN_POINT('Ctrl Pts',(-50.3339110252539,-27.8569369682875,
177.264936028611));
#15550=CARTESIAN_POINT('Ctrl Pts',(-50.2683927599471,-27.8299386004748,
177.362186354007));
#15551=CARTESIAN_POINT('Ctrl Pts',(-50.193114320713,-27.8005016688432,177.448440461337));
#15552=CARTESIAN_POINT('Ctrl Pts',(-47.1031441589869,-31.5480734342088,
175.585485069079));
#15553=CARTESIAN_POINT('Ctrl Pts',(-47.1603662041614,-31.2513383379729,
175.585485069079));
#15554=CARTESIAN_POINT('Ctrl Pts',(-47.2482359974308,-30.9149655772776,
175.587875715227));
#15555=CARTESIAN_POINT('Ctrl Pts',(-47.4670950242505,-30.3000308864083,
175.601419934118));
#15556=CARTESIAN_POINT('Ctrl Pts',(-47.6018961077871,-30.0028542362142,
175.612574303893));
#15557=CARTESIAN_POINT('Ctrl Pts',(-48.06625584225,-29.1754899206181,175.666311941427));
#15558=CARTESIAN_POINT('Ctrl Pts',(-48.4618683742085,-28.7136853353929,
175.729732505271));
#15559=CARTESIAN_POINT('Ctrl Pts',(-49.0063756293611,-28.1949480459011,
175.890763292055));
#15560=CARTESIAN_POINT('Ctrl Pts',(-49.1677731230246,-28.0480163131157,
175.972468320302));
#15561=CARTESIAN_POINT('Ctrl Pts',(-49.3965343491423,-27.8703147335455,
176.056354650694));
#15562=CARTESIAN_POINT('Ctrl Pts',(-49.5042735598544,-27.8224509492496,
176.029622920355));
#15563=CARTESIAN_POINT('Ctrl Pts',(-49.714154138436,-27.7365778903946,176.021696276872));
#15564=CARTESIAN_POINT('Ctrl Pts',(-49.8092250008766,-27.6958009021663,
176.040400247712));
#15565=CARTESIAN_POINT('Ctrl Pts',(-50.0526599599857,-27.5670382667944,
176.149507116298));
#15566=CARTESIAN_POINT('Ctrl Pts',(-50.1573360552302,-27.4697774585579,
176.29868387691));
#15567=CARTESIAN_POINT('Ctrl Pts',(-50.1883082447542,-27.3362137867349,
176.557013250615));
#15568=CARTESIAN_POINT('Ctrl Pts',(-50.1794299894878,-27.2944646349798,
176.647304730812));
#15569=CARTESIAN_POINT('Ctrl Pts',(-50.1311335533471,-27.2163290407286,
176.829965813571));
#15570=CARTESIAN_POINT('Ctrl Pts',(-50.0905156624001,-27.1753600677279,
176.937389673553));
#15571=CARTESIAN_POINT('Ctrl Pts',(-50.0383214665825,-27.1440081492037,
177.018259765604));
#15572=CARTESIAN_POINT('Ctrl Pts',(-47.1031441589869,-31.5480734342088,
176.385485069079));
#15573=CARTESIAN_POINT('Ctrl Pts',(-47.1599854936771,-31.2533125799253,
176.385485069079));
#15574=CARTESIAN_POINT('Ctrl Pts',(-47.2462550636215,-30.9240508319461,
176.387855155919));
#15575=CARTESIAN_POINT('Ctrl Pts',(-47.460249087206,-30.3229192382893,176.401096636113));
#15576=CARTESIAN_POINT('Ctrl Pts',(-47.5913742255291,-30.0344018731676,
176.411980487031));
#15577=CARTESIAN_POINT('Ctrl Pts',(-48.0375122982338,-29.2397387684011,
176.463601555155));
#15578=CARTESIAN_POINT('Ctrl Pts',(-48.4124469809922,-28.8074108937189,
176.525602813253));
#15579=CARTESIAN_POINT('Ctrl Pts',(-48.8848496853331,-28.3577893519108,
176.665278154737));
#15580=CARTESIAN_POINT('Ctrl Pts',(-49.026848150992,-28.2513597906944,176.736022770841));
#15581=CARTESIAN_POINT('Ctrl Pts',(-49.1705854582322,-28.1079648662814,
176.786782875481));
#15582=CARTESIAN_POINT('Ctrl Pts',(-49.2060240792629,-28.0278386987345,
176.747088553392));
#15583=CARTESIAN_POINT('Ctrl Pts',(-49.2810889004422,-27.9003322593211,
176.67860791329));
#15584=CARTESIAN_POINT('Ctrl Pts',(-49.3144205003265,-27.8541778608178,
176.654181717029));
#15585=CARTESIAN_POINT('Ctrl Pts',(-49.3895778283813,-27.7529515714288,
176.588058724708));
#15586=CARTESIAN_POINT('Ctrl Pts',(-49.4143850760995,-27.7397337398683,
176.533088088996));
#15587=CARTESIAN_POINT('Ctrl Pts',(-49.4653959512805,-27.6892053509014,
176.504625861351));
#15588=CARTESIAN_POINT('Ctrl Pts',(-49.480846052191,-27.6666966453102,176.508814220202));
#15589=CARTESIAN_POINT('Ctrl Pts',(-49.4871117159947,-27.6078471194517,
176.551208753368));
#15590=CARTESIAN_POINT('Ctrl Pts',(-49.4794905861727,-27.5632681966532,
176.593760604048));
#15591=CARTESIAN_POINT('Ctrl Pts',(-49.4509304485228,-27.5317240793367,
176.63793339336));
#15592=CARTESIAN_POINT('Ctrl Pts',(-47.8886718415116,-31.6995536639001,
176.385485069079));
#15593=CARTESIAN_POINT('Ctrl Pts',(-47.9420283886728,-31.4228637953642,
176.385485069079));
#15594=CARTESIAN_POINT('Ctrl Pts',(-48.014532730032,-31.1513028861565,176.387574911196));
#15595=CARTESIAN_POINT('Ctrl Pts',(-48.1993444429345,-30.6321564992392,
176.398971294295));
#15596=CARTESIAN_POINT('Ctrl Pts',(-48.3114636593991,-30.3858920090494,
176.408301592892));
#15597=CARTESIAN_POINT('Ctrl Pts',(-48.6906159914853,-29.7105605916654,
176.452071210751));
#15598=CARTESIAN_POINT('Ctrl Pts',(-49.0051697309234,-29.3466926348484,
176.50329885969));
#15599=CARTESIAN_POINT('Ctrl Pts',(-49.4230059122887,-28.9490152774608,
176.626542944478));
#15600=CARTESIAN_POINT('Ctrl Pts',(-49.5578148191563,-28.8469683228627,
176.674952306832));
#15601=CARTESIAN_POINT('Ctrl Pts',(-49.7002666962155,-28.7067737347251,
176.755688647613));
#15602=CARTESIAN_POINT('Ctrl Pts',(-49.7204366648883,-28.6425144311754,
176.784380821457));
#15603=CARTESIAN_POINT('Ctrl Pts',(-49.7511647401251,-28.5326907442027,
176.830228856146));
#15604=CARTESIAN_POINT('Ctrl Pts',(-49.7620981348669,-28.4891228428723,
176.849617895289));
#15605=CARTESIAN_POINT('Ctrl Pts',(-49.7760060876902,-28.3888257184543,
176.893673366674));
#15606=CARTESIAN_POINT('Ctrl Pts',(-49.764988315943,-28.3659620364717,176.891507252207));
#15607=CARTESIAN_POINT('Ctrl Pts',(-49.7443870109756,-28.3164417615759,
176.916482255318));
#15608=CARTESIAN_POINT('Ctrl Pts',(-49.7340979234319,-28.2968315737579,
176.932476541289));
#15609=CARTESIAN_POINT('Ctrl Pts',(-49.6898891879014,-28.2484550470107,
176.986178968408));
#15610=CARTESIAN_POINT('Ctrl Pts',(-49.6573676837196,-28.2178467294001,
177.018557284502));
#15611=CARTESIAN_POINT('Ctrl Pts',(-49.6057233026532,-28.1882175989763,
177.068114089093));
#15612=CARTESIAN_POINT('Ctrl Pts',(-48.6741995240363,-31.8510338935913,
176.385485069079));
#15613=CARTESIAN_POINT('Ctrl Pts',(-48.7240712836685,-31.5924150108031,
176.385485069079));
#15614=CARTESIAN_POINT('Ctrl Pts',(-48.7828103964424,-31.3785549403669,
176.387294666473));
#15615=CARTESIAN_POINT('Ctrl Pts',(-48.9384397986629,-30.941393760189,176.396845952478));
#15616=CARTESIAN_POINT('Ctrl Pts',(-49.0315530932691,-30.7373821449313,
176.404622698753));
#15617=CARTESIAN_POINT('Ctrl Pts',(-49.3437196847369,-30.1813824149298,
176.440540866346));
#15618=CARTESIAN_POINT('Ctrl Pts',(-49.5978924808545,-29.8859743759779,
176.480994906127));
#15619=CARTESIAN_POINT('Ctrl Pts',(-49.9611621392443,-29.5402412030108,
176.587807734218));
#15620=CARTESIAN_POINT('Ctrl Pts',(-50.0887814873205,-29.442576855031,176.613881842823));
#15621=CARTESIAN_POINT('Ctrl Pts',(-50.2299479341988,-29.3055826031689,
176.724594419746));
#15622=CARTESIAN_POINT('Ctrl Pts',(-50.2348492505137,-29.2571901636164,
176.821673089522));
#15623=CARTESIAN_POINT('Ctrl Pts',(-50.221240579808,-29.1650492290843,176.981849799003));
#15624=CARTESIAN_POINT('Ctrl Pts',(-50.2097757694073,-29.1240678249268,
177.04505407355));
#15625=CARTESIAN_POINT('Ctrl Pts',(-50.162434346999,-29.0246998654798,177.199288008639));
#15626=CARTESIAN_POINT('Ctrl Pts',(-50.1155915557866,-28.9921903330752,
177.249926415417));
#15627=CARTESIAN_POINT('Ctrl Pts',(-50.0233780706706,-28.9436781722504,
177.328338649285));
#15628=CARTESIAN_POINT('Ctrl Pts',(-49.9873497946729,-28.9269665022055,
177.356138862376));
#15629=CARTESIAN_POINT('Ctrl Pts',(-49.8926666598081,-28.8890629745697,
177.421149183448));
#15630=CARTESIAN_POINT('Ctrl Pts',(-49.8352447812666,-28.872425262147,177.443353964955));
#15631=CARTESIAN_POINT('Ctrl Pts',(-49.7605161567837,-28.8447111186158,
177.498294784826));
#15632=CARTESIAN_POINT('Ctrl Pts',(-48.6741995240363,-31.8510338935913,
175.585485069079));
#15633=CARTESIAN_POINT('Ctrl Pts',(-48.7244519941528,-31.5904407688506,
175.585485069079));
#15634=CARTESIAN_POINT('Ctrl Pts',(-48.7847913302516,-31.3694696856984,
175.587315225781));
#15635=CARTESIAN_POINT('Ctrl Pts',(-48.9452857357075,-30.918505408308,175.597169250483));
#15636=CARTESIAN_POINT('Ctrl Pts',(-49.042074975527,-30.7058345079779,175.605216515615));
#15637=CARTESIAN_POINT('Ctrl Pts',(-49.3724632287533,-30.1171335671469,
175.643251252618));
#15638=CARTESIAN_POINT('Ctrl Pts',(-49.6473138740709,-29.7922488176511,
175.685124598145));
#15639=CARTESIAN_POINT('Ctrl Pts',(-50.0826880832722,-29.3773998970014,
175.813292871536));
#15640=CARTESIAN_POINT('Ctrl Pts',(-50.2297064593532,-29.239233377452,175.850327392284));
#15641=CARTESIAN_POINT('Ctrl Pts',(-50.4558968251088,-29.0679324704331,
175.99416619496));
#15642=CARTESIAN_POINT('Ctrl Pts',(-50.5330987311051,-29.0518024141316,
176.104207456485));
#15643=CARTESIAN_POINT('Ctrl Pts',(-50.6543058178018,-29.0012948601576,
176.324938162585));
#15644=CARTESIAN_POINT('Ctrl Pts',(-50.7045802699575,-28.9656908662752,
176.431272604233));
#15645=CARTESIAN_POINT('Ctrl Pts',(-50.8255164786033,-28.8387865608456,
176.760736400229));
#15646=CARTESIAN_POINT('Ctrl Pts',(-50.8585425349173,-28.722234051765,177.015522203332));
#15647=CARTESIAN_POINT('Ctrl Pts',(-50.7462903641443,-28.5906866080838,
177.38072603855));
#15648=CARTESIAN_POINT('Ctrl Pts',(-50.6859337319697,-28.5547344918753,
177.494629372986));
#15649=CARTESIAN_POINT('Ctrl Pts',(-50.5366884971606,-28.4975448958465,
177.699906243651));
#15650=CARTESIAN_POINT('Ctrl Pts',(-50.446269857494,-28.4845171332217,177.786983034461));
#15651=CARTESIAN_POINT('Ctrl Pts',(-50.3479071748434,-28.4569951884828,
177.87862115707));
#15652=CARTESIAN_POINT('Ctrl Pts',(-47.8886718415116,-31.6995536639001,
175.585485069079));
#15653=CARTESIAN_POINT('Ctrl Pts',(-47.9424090991571,-31.4208895534118,
175.585485069079));
#15654=CARTESIAN_POINT('Ctrl Pts',(-48.0165136638412,-31.142217631488,175.587595470504));
#15655=CARTESIAN_POINT('Ctrl Pts',(-48.206190379979,-30.6092681473582,175.5992945923));
#15656=CARTESIAN_POINT('Ctrl Pts',(-48.3219855416571,-30.3543443720961,
175.608895409754));
#15657=CARTESIAN_POINT('Ctrl Pts',(-48.7193595355016,-29.6463117438825,
175.654781597023));
#15658=CARTESIAN_POINT('Ctrl Pts',(-49.0545911241397,-29.252967076522,175.707428551708));
#15659=CARTESIAN_POINT('Ctrl Pts',(-49.5445318563166,-28.7861739714513,
175.852028081795));
#15660=CARTESIAN_POINT('Ctrl Pts',(-49.6987397911889,-28.6436248452838,
175.911397856293));
#15661=CARTESIAN_POINT('Ctrl Pts',(-49.9262155871255,-28.4691236019893,
176.025260422827));
#15662=CARTESIAN_POINT('Ctrl Pts',(-50.0186861454797,-28.4371266816906,
176.06691518842));
#15663=CARTESIAN_POINT('Ctrl Pts',(-50.1842299781189,-28.3689363752761,
176.173317219728));
#15664=CARTESIAN_POINT('Ctrl Pts',(-50.2569026354171,-28.3307458842207,
176.235836425973));
#15665=CARTESIAN_POINT('Ctrl Pts',(-50.4390882192945,-28.20291241382,176.455121758264));
#15666=CARTESIAN_POINT('Ctrl Pts',(-50.5079392950738,-28.0960057551614,
176.657103040121));
#15667=CARTESIAN_POINT('Ctrl Pts',(-50.4672993044493,-27.9634501974094,
176.968869644582));
#15668=CARTESIAN_POINT('Ctrl Pts',(-50.4326818607288,-27.9245995634275,
177.070967051899));
#15669=CARTESIAN_POINT('Ctrl Pts',(-50.3339110252539,-27.8569369682875,
177.264936028611));
#15670=CARTESIAN_POINT('Ctrl Pts',(-50.2683927599471,-27.8299386004748,
177.362186354007));
#15671=CARTESIAN_POINT('Ctrl Pts',(-50.193114320713,-27.8005016688432,177.448440461337));
#15672=CARTESIAN_POINT('Origin',(-54.5589537515075,2.89037996126418,174.712692862944));
#15673=CARTESIAN_POINT('Origin',(-47.4705283379689,-33.8679111978839,177.258277275215));
#15674=CARTESIAN_POINT('',(0.,0.,0.));
#15675=CARTESIAN_POINT('Origin',(-38.9776940652676,8.40516957928876,178.735485069079));
#15676=CARTESIAN_POINT('',(-42.2848832040984,8.40516957928876,180.985485069079));
#15677=CARTESIAN_POINT('Origin',(-38.9776940652676,8.40516957928876,180.985485069079));
#15678=CARTESIAN_POINT('Origin',(-38.9776940652676,8.40516957928876,175.985485069079));
#15679=CARTESIAN_POINT('',(-38.9776940652676,10.4051695792888,180.985485069079));
#15680=CARTESIAN_POINT('Origin',(-38.9776940652676,8.40516957928876,180.985485069079));
#15681=CARTESIAN_POINT('',(-38.9776940652676,10.4051695792888,170.985485069079));
#15682=CARTESIAN_POINT('',(-38.9776940652676,10.4051695792888,175.985485069079));
#15683=CARTESIAN_POINT('Origin',(-38.9776940652676,8.40516957928876,170.985485069079));
#15684=CARTESIAN_POINT('Origin',(-38.9776940652676,8.40516957928876,173.235485069079));
#15685=CARTESIAN_POINT('',(-42.2848832040984,8.40516957928876,170.985485069079));
#15686=CARTESIAN_POINT('Origin',(-38.9776940652676,8.40516957928876,170.985485069079));
#15687=CARTESIAN_POINT('Origin',(-36.9776940652676,8.40516957928876,170.985485069079));
#15688=CARTESIAN_POINT('Origin',(-36.9776940652676,8.40516957928876,180.985485069079));
#15689=CARTESIAN_POINT('',(0.,0.,0.));
#15690=CARTESIAN_POINT('Origin',(-36.6843857876575,24.5637629925993,178.485485069079));
#15691=CARTESIAN_POINT('',(-41.6447424765058,23.9353829170101,177.985485069079));
#15692=CARTESIAN_POINT('',(-41.5929060189763,25.5158287144556,177.985485069079));
#15693=CARTESIAN_POINT('Origin',(-36.6843857876575,24.5637629925993,177.985485069079));
#15694=CARTESIAN_POINT('',(-41.5929060189763,25.5158287144556,173.985485069079));
#15695=CARTESIAN_POINT('',(-41.5929060189763,25.5158287144556,178.485485069079));
#15696=CARTESIAN_POINT('',(-41.6447424765058,23.9353829170101,173.985485069079));
#15697=CARTESIAN_POINT('Origin',(-36.6843857876575,24.5637629925993,173.985485069079));
#15698=CARTESIAN_POINT('',(-41.6447424765058,23.9353829170101,173.485485069079));
#15699=CARTESIAN_POINT('',(-41.6447424765058,23.9353829170101,173.985485069079));
#15700=CARTESIAN_POINT('',(-36.0590295603455,19.6030241777692,173.485485069079));
#15701=CARTESIAN_POINT('Origin',(-36.6843857876575,24.5637629925993,173.485485069079));
#15702=CARTESIAN_POINT('',(-36.0590295603455,19.6030241777692,178.485485069079));
#15703=CARTESIAN_POINT('',(-36.0590295603455,19.6030241777692,178.485485069079));
#15704=CARTESIAN_POINT('',(-41.5571272820614,23.4428748051719,178.485485069079));
#15705=CARTESIAN_POINT('Origin',(-36.6843857876575,24.5637629925993,178.485485069079));
#15706=CARTESIAN_POINT('',(-41.6447424765058,23.9353829170101,178.985485069079));
#15707=CARTESIAN_POINT('Ctrl Pts',(-41.6447424765058,23.9353829170101,178.985485069079));
#15708=CARTESIAN_POINT('Ctrl Pts',(-41.6447424765058,23.9353829170101,178.947628514448));
#15709=CARTESIAN_POINT('Ctrl Pts',(-41.6442074037926,23.931116111951,178.909894818394));
#15710=CARTESIAN_POINT('Ctrl Pts',(-41.6420233045055,23.9142225446529,178.836122709058));
#15711=CARTESIAN_POINT('Ctrl Pts',(-41.6403803832545,23.9016504746563,178.800323230855));
#15712=CARTESIAN_POINT('Ctrl Pts',(-41.6342624737586,23.8569870933521,178.707899216115));
#15713=CARTESIAN_POINT('Ctrl Pts',(-41.628662774516,23.817789652519,178.655609780093));
#15714=CARTESIAN_POINT('Ctrl Pts',(-41.61328097085,23.722137104376,178.569197903206));
#15715=CARTESIAN_POINT('Ctrl Pts',(-41.6036260582216,23.6666496809067,178.535876943855));
#15716=CARTESIAN_POINT('Ctrl Pts',(-41.5816188124318,23.5538091064277,178.495162061707));
#15717=CARTESIAN_POINT('Ctrl Pts',(-41.5699032941903,23.4984148716403,178.485485069079));
#15718=CARTESIAN_POINT('Ctrl Pts',(-41.5571272820614,23.4428748051719,178.485485069079));
#15719=CARTESIAN_POINT('',(-41.6447424765058,23.9353829170101,178.485485069079));
#15720=CARTESIAN_POINT('Origin',(-60.1632027754914,33.6789365837495,173.985485069079));
#15721=CARTESIAN_POINT('',(-28.0689593736356,55.8365434144167,173.485485069079));
#15722=CARTESIAN_POINT('',(-21.8418923193128,26.4348241521828,173.485485069079));
#15723=CARTESIAN_POINT('Origin',(-60.1632027754914,33.6789365837495,173.485485069079));
#15724=CARTESIAN_POINT('',(-27.6574947146374,56.1206152968612,173.985485069079));
#15725=CARTESIAN_POINT('Origin',(-28.0689593736356,55.8365434144167,173.985485069079));
#15726=CARTESIAN_POINT('',(-21.3209582807514,26.5004936738394,173.985485069079));
#15727=CARTESIAN_POINT('Origin',(-60.1632027754914,33.6789365837495,173.985485069079));
#15728=CARTESIAN_POINT('Ctrl Pts',(-21.8418923193129,26.4348241521828,173.485485069079));
#15729=CARTESIAN_POINT('Ctrl Pts',(-21.7765607092714,26.443059927277,173.485485069079));
#15730=CARTESIAN_POINT('Ctrl Pts',(-21.6995647127339,26.4527661278471,173.500361703275));
#15731=CARTESIAN_POINT('Ctrl Pts',(-21.5798826947022,26.4678533755469,173.548919514567));
#15732=CARTESIAN_POINT('Ctrl Pts',(-21.5156359974204,26.4759523853374,173.590627108911));
#15733=CARTESIAN_POINT('Ctrl Pts',(-21.4256203189965,26.487299861421,173.678725059264));
#15734=CARTESIAN_POINT('Ctrl Pts',(-21.3833926501498,26.4926231281084,173.740151465957));
#15735=CARTESIAN_POINT('Ctrl Pts',(-21.3355571377766,26.4986533257596,173.853335868708));
#15736=CARTESIAN_POINT('Ctrl Pts',(-21.3209582807514,26.5004936738394,173.924735228568));
#15737=CARTESIAN_POINT('Ctrl Pts',(-21.3209582807514,26.5004936738394,173.985485069079));
#15738=CARTESIAN_POINT('Origin',(-60.1632027754914,33.6789365837495,177.985485069079));
#15739=CARTESIAN_POINT('',(-27.6574947146374,56.1206152968612,177.985485069079));
#15740=CARTESIAN_POINT('',(-21.3209582807514,26.5004936738394,177.985485069079));
#15741=CARTESIAN_POINT('Origin',(-60.1632027754914,33.6789365837495,177.985485069079));
#15742=CARTESIAN_POINT('',(-28.0689593736356,55.8365434144167,178.485485069079));
#15743=CARTESIAN_POINT('Origin',(-28.0689593736356,55.8365434144167,177.985485069079));
#15744=CARTESIAN_POINT('',(-21.8418923193128,26.4348241521828,178.485485069079));
#15745=CARTESIAN_POINT('Origin',(-60.1632027754914,33.6789365837495,178.485485069079));
#15746=CARTESIAN_POINT('Ctrl Pts',(-21.3209582807514,26.5004936738394,177.985485069079));
#15747=CARTESIAN_POINT('Ctrl Pts',(-21.3209582807514,26.5004936738394,178.046234909591));
#15748=CARTESIAN_POINT('Ctrl Pts',(-21.3355571377766,26.4986533257596,178.117634269451));
#15749=CARTESIAN_POINT('Ctrl Pts',(-21.3833926501498,26.4926231281084,178.230818672202));
#15750=CARTESIAN_POINT('Ctrl Pts',(-21.4256203189965,26.487299861421,178.292245078894));
#15751=CARTESIAN_POINT('Ctrl Pts',(-21.5156359974204,26.4759523853374,178.380343029248));
#15752=CARTESIAN_POINT('Ctrl Pts',(-21.5798826947022,26.4678533755469,178.422050623592));
#15753=CARTESIAN_POINT('Ctrl Pts',(-21.6995647127339,26.4527661278471,178.470608434884));
#15754=CARTESIAN_POINT('Ctrl Pts',(-21.7765607092714,26.443059927277,178.485485069079));
#15755=CARTESIAN_POINT('Ctrl Pts',(-21.8418923193129,26.4348241521828,178.485485069079));
#15756=CARTESIAN_POINT('Origin',(-32.4121430547972,41.0900517459514,178.985485069079));
#15757=CARTESIAN_POINT('',(-33.3358320373305,35.4434146616551,178.735485069079));
#15758=CARTESIAN_POINT('',(-26.7516402862307,41.9245696338691,178.735485069079));
#15759=CARTESIAN_POINT('Origin',(-32.4121430547972,41.0900517459514,178.735485069079));
#15760=CARTESIAN_POINT('',(-33.7154041461839,35.0749167312736,178.485485069079));
#15761=CARTESIAN_POINT('Ctrl Pts',(-33.3358320373305,35.4434146616551,178.735485069079));
#15762=CARTESIAN_POINT('Ctrl Pts',(-33.3446356128532,35.4344346820991,178.717673683699));
#15763=CARTESIAN_POINT('Ctrl Pts',(-33.3542668467474,35.4246420637755,178.700821574011));
#15764=CARTESIAN_POINT('Ctrl Pts',(-33.3645777815926,35.4142026008384,178.684920753159));
#15765=CARTESIAN_POINT('Ctrl Pts',(-33.3756414866745,35.4030009842163,178.667859061362));
#15766=CARTESIAN_POINT('Ctrl Pts',(-33.3874878790304,35.3910544439032,178.65189219269));
#15767=CARTESIAN_POINT('Ctrl Pts',(-33.3999755348309,35.3785236283123,178.637015071129));
#15768=CARTESIAN_POINT('Ctrl Pts',(-33.4130084572907,35.3654456615133,178.621488348193));
#15769=CARTESIAN_POINT('Ctrl Pts',(-33.4267402497532,35.351730797418,178.607148080583));
#15770=CARTESIAN_POINT('Ctrl Pts',(-33.4410493968144,35.3375207872263,178.594001236326));
#15771=CARTESIAN_POINT('Ctrl Pts',(-33.4561591001456,35.3225157671918,178.58011886335));
#15772=CARTESIAN_POINT('Ctrl Pts',(-33.4719129905256,35.3069580905995,178.567566428292));
#15773=CARTESIAN_POINT('Ctrl Pts',(-33.4882045709165,35.2909781638283,178.55637629334));
#15774=CARTESIAN_POINT('Ctrl Pts',(-33.4908937363219,35.2883404414452,178.554529196676));
#15775=CARTESIAN_POINT('Ctrl Pts',(-33.4935976198782,35.2856911491175,178.552719283668));
#15776=CARTESIAN_POINT('Ctrl Pts',(-33.496315818567,35.2830308017146,178.550946781807));
#15777=CARTESIAN_POINT('Ctrl Pts',(-33.4979816419081,35.2814004320077,178.549860520165));
#15778=CARTESIAN_POINT('Ctrl Pts',(-33.4996535237804,35.2797653173119,178.548787729124));
#15779=CARTESIAN_POINT('Ctrl Pts',(-33.5013313549608,35.2781255722169,178.547728373383));
#15780=CARTESIAN_POINT('Ctrl Pts',(-33.5188939634074,35.2609616278402,178.536639623625));
#15781=CARTESIAN_POINT('Ctrl Pts',(-33.5370160952805,35.2433826910993,178.527077684688));
#15782=CARTESIAN_POINT('Ctrl Pts',(-33.555555321407,35.2255349949421,178.51898718902));
#15783=CARTESIAN_POINT('Ctrl Pts',(-33.5747845425526,35.2070230412065,178.510595580367));
#15784=CARTESIAN_POINT('Ctrl Pts',(-33.5944632801671,35.1882210900316,178.503786595037));
#15785=CARTESIAN_POINT('Ctrl Pts',(-33.6144624549482,35.1692666992868,178.498541410487));
#15786=CARTESIAN_POINT('Ctrl Pts',(-33.6347878405447,35.1500031394223,178.49321067061));
#15787=CARTESIAN_POINT('Ctrl Pts',(-33.6554451836208,35.1305810847787,178.48949483668));
#15788=CARTESIAN_POINT('Ctrl Pts',(-33.6763154303043,35.111133705737,178.487422973537));
#15789=CARTESIAN_POINT('Ctrl Pts',(-33.6892719921304,35.0990604814608,178.486136729856));
#15790=CARTESIAN_POINT('Ctrl Pts',(-33.7023108775159,35.0869773346724,178.485485069079));
#15791=CARTESIAN_POINT('Ctrl Pts',(-33.7154041461839,35.0749167312735,178.485485069079));
#15792=CARTESIAN_POINT('',(-26.3219838963068,41.9787334640029,178.485485070198));
#15793=CARTESIAN_POINT('Origin',(-32.4121430547972,41.0900517459514,178.485485069079));
#15794=CARTESIAN_POINT('Origin',(-26.3219553285719,41.9787349031418,178.985611152631));
#15795=CARTESIAN_POINT('Origin',(-32.4121430547972,41.0900517459514,172.985485069079));
#15796=CARTESIAN_POINT('',(-33.7154041461839,35.0749167312736,173.485485069079));
#15797=CARTESIAN_POINT('',(-26.3219838963069,41.978733464003,173.485485067961));
#15798=CARTESIAN_POINT('Origin',(-32.4121430547972,41.0900517459514,173.485485069079));
#15799=CARTESIAN_POINT('',(-33.3358320373305,35.4434146616551,173.235485069079));
#15800=CARTESIAN_POINT('Ctrl Pts',(-33.7154041461839,35.0749167312736,173.485485069079));
#15801=CARTESIAN_POINT('Ctrl Pts',(-33.6954888490377,35.0932613104929,173.485485069079));
#15802=CARTESIAN_POINT('Ctrl Pts',(-33.6757087151231,35.1116502887521,173.483968922187));
#15803=CARTESIAN_POINT('Ctrl Pts',(-33.6561598265164,35.1299705828502,173.481006046776));
#15804=CARTESIAN_POINT('Ctrl Pts',(-33.636566911742,35.1483321361909,173.478036498656));
#15805=CARTESIAN_POINT('Ctrl Pts',(-33.6172052208955,35.1666258031105,173.473613456166));
#15806=CARTESIAN_POINT('Ctrl Pts',(-33.5981739866564,35.1847410363725,173.467754726979));
#15807=CARTESIAN_POINT('Ctrl Pts',(-33.580095426628,35.2019494490188,173.462189276732));
#15808=CARTESIAN_POINT('Ctrl Pts',(-33.5623142955273,35.2189976863789,173.455327760286));
#15809=CARTESIAN_POINT('Ctrl Pts',(-33.5449309637082,35.2357800196407,173.447144659799));
#15810=CARTESIAN_POINT('Ctrl Pts',(-33.530114973709,35.2500837724746,173.440170120267));
#15811=CARTESIAN_POINT('Ctrl Pts',(-33.5155878973462,35.2641945027656,173.43223485025));
#15812=CARTESIAN_POINT('Ctrl Pts',(-33.5014276378414,35.2780331864915,173.423301327231));
#15813=CARTESIAN_POINT('Ctrl Pts',(-33.4997577343866,35.2796651668769,173.422247806923));
#15814=CARTESIAN_POINT('Ctrl Pts',(-33.4980939376313,35.2812923576261,173.421181015993));
#15815=CARTESIAN_POINT('Ctrl Pts',(-33.4964363677189,35.2829146343261,173.420100920878));
#15816=CARTESIAN_POINT('Ctrl Pts',(-33.4803968946902,35.2986125926318,173.409649381951));
#15817=CARTESIAN_POINT('Ctrl Pts',(-33.4648415796479,35.3139396402464,173.397884146828));
#15818=CARTESIAN_POINT('Ctrl Pts',(-33.4498680795511,35.3287758944578,173.384843020246));
#15819=CARTESIAN_POINT('Ctrl Pts',(-33.4355338630463,35.3429787246988,173.372358675859));
#15820=CARTESIAN_POINT('Ctrl Pts',(-33.4217324124934,35.3567323181604,173.358704431557));
#15821=CARTESIAN_POINT('Ctrl Pts',(-33.4085774472733,35.3699038956445,173.343892300498));
#15822=CARTESIAN_POINT('Ctrl Pts',(-33.3960026091048,35.3824946134848,173.329733376633));
#15823=CARTESIAN_POINT('Ctrl Pts',(-33.3840181614552,35.3945539366785,173.314515951653));
#15824=CARTESIAN_POINT('Ctrl Pts',(-33.3727549753283,35.4059333420876,173.298238618397));
#15825=CARTESIAN_POINT('Ctrl Pts',(-33.3621571222363,35.4166405492172,173.282922811249));
#15826=CARTESIAN_POINT('Ctrl Pts',(-33.352197670638,35.4267460178717,173.266668241163));
#15827=CARTESIAN_POINT('Ctrl Pts',(-33.3430175110135,35.4360922327446,173.249468987379));
#15828=CARTESIAN_POINT('Ctrl Pts',(-33.3405655228213,35.4385885737068,173.244875127476));
#15829=CARTESIAN_POINT('Ctrl Pts',(-33.3381693226984,35.4410305423009,173.240213862542));
#15830=CARTESIAN_POINT('Ctrl Pts',(-33.3358320373305,35.4434146616551,173.235485069079));
#15831=CARTESIAN_POINT('',(-26.7516402862308,41.9245696338692,173.235485069079));
#15832=CARTESIAN_POINT('Origin',(-32.4121430547972,41.0900517459514,173.235485069079));
#15833=CARTESIAN_POINT('Origin',(-26.3219553285719,41.9787349031418,172.985358985528));
#15834=CARTESIAN_POINT('Origin',(-32.4121430547972,41.0900517459514,171.985485069079));
#15835=CARTESIAN_POINT('',(-27.4666827350209,41.8265449404332,171.985485069079));
#15836=CARTESIAN_POINT('',(-32.9897423165504,36.1235254330303,171.985485177731));
#15837=CARTESIAN_POINT('Origin',(-32.4121430547972,41.0900517459514,171.985485069079));
#15838=CARTESIAN_POINT('Ctrl Pts',(-26.7516402862308,41.9245696338692,173.235485069079));
#15839=CARTESIAN_POINT('Ctrl Pts',(-26.9899986267538,41.8919790534973,172.818818009845));
#15840=CARTESIAN_POINT('Ctrl Pts',(-27.2283468751689,41.8593100351519,172.402151301397));
#15841=CARTESIAN_POINT('Ctrl Pts',(-27.4666827350209,41.8265449404332,171.985485069079));
#15842=CARTESIAN_POINT('Ctrl Pts',(-33.3358320373305,35.4434146616551,173.235485069079));
#15843=CARTESIAN_POINT('Ctrl Pts',(-33.2135131757875,35.6670237814666,172.81906058758));
#15844=CARTESIAN_POINT('Ctrl Pts',(-33.0981931871628,35.893798298462,172.402420570166));
#15845=CARTESIAN_POINT('Ctrl Pts',(-32.9897418511957,36.1235256358927,171.985485410552));
#15846=CARTESIAN_POINT('Origin',(-32.4121430547972,41.0900517459514,179.985485069079));
#15847=CARTESIAN_POINT('',(-27.4666827350209,41.8265449404332,179.985485069079));
#15848=CARTESIAN_POINT('',(-32.9897423165518,36.1235254330304,179.985484960428));
#15849=CARTESIAN_POINT('Origin',(-32.4121430547972,41.0900517459514,179.985485069079));
#15850=CARTESIAN_POINT('Ctrl Pts',(-32.9897418511957,36.1235256358926,179.985484727606));
#15851=CARTESIAN_POINT('Ctrl Pts',(-33.0981931871628,35.893798298462,179.568549567993));
#15852=CARTESIAN_POINT('Ctrl Pts',(-33.2135131757875,35.6670237814665,179.151909550578));
#15853=CARTESIAN_POINT('Ctrl Pts',(-33.3358320373305,35.4434146616551,178.735485069079));
#15854=CARTESIAN_POINT('Ctrl Pts',(-27.4666827350209,41.8265449404332,179.985485069079));
#15855=CARTESIAN_POINT('Ctrl Pts',(-27.2283468751687,41.8593100351504,179.568818836762));
#15856=CARTESIAN_POINT('Ctrl Pts',(-26.9899986267537,41.8919790534971,179.152152128314));
#15857=CARTESIAN_POINT('Ctrl Pts',(-26.7516402862307,41.9245696338691,178.735485069079));
#15858=CARTESIAN_POINT('Origin',(-38.9776940652676,8.40516957928876,165.645237852233));
#15859=CARTESIAN_POINT('',(-40.9664250445818,8.61718158818506,178.485485069079));
#15860=CARTESIAN_POINT('Origin',(-38.9776940652676,8.40516957928876,178.485485069079));
#15861=CARTESIAN_POINT('',(-40.9664250445818,8.61718158818506,180.985485069079));
#15862=CARTESIAN_POINT('',(-40.9664250445818,8.61718158818506,165.645237852233));
#15863=CARTESIAN_POINT('Origin',(-38.9776940652676,8.40516957928876,180.985485069079));
#15864=CARTESIAN_POINT('Origin',(-38.9776940652676,8.40516957928876,165.645237852233));
#15865=CARTESIAN_POINT('',(-40.9664250445818,8.61718158818506,170.985485069079));
#15866=CARTESIAN_POINT('Origin',(-38.9776940652676,8.40516957928876,170.985485069079));
#15867=CARTESIAN_POINT('',(-40.9664250445818,8.61718158818506,173.485485069079));
#15868=CARTESIAN_POINT('',(-40.9664250445818,8.61718158818506,165.645237852233));
#15869=CARTESIAN_POINT('Origin',(-38.9776940652676,8.40516957928876,173.485485069079));
#15870=CARTESIAN_POINT('Origin',(-39.4690592605811,9.0940082318961,180.985485069079));
#15871=CARTESIAN_POINT('',(-54.4340581561246,8.06989492938437,173.485485069079));
#15872=CARTESIAN_POINT('Origin',(-39.4690592605811,9.0940082318961,173.485485069079));
#15873=CARTESIAN_POINT('',(-41.3451279425171,23.9762246763865,173.526200018228));
#15874=CARTESIAN_POINT('Ctrl Pts',(-41.6447424765058,23.9353829170101,173.985485069079));
#15875=CARTESIAN_POINT('Ctrl Pts',(-41.6447424765058,23.9353829170101,173.920389070876));
#15876=CARTESIAN_POINT('Ctrl Pts',(-41.6321641038074,23.9372419809971,173.855916759188));
#15877=CARTESIAN_POINT('Ctrl Pts',(-41.5832406087156,23.944289310737,173.735462005052));
#15878=CARTESIAN_POINT('Ctrl Pts',(-41.547358159805,23.9494033791653,173.680632537013));
#15879=CARTESIAN_POINT('Ctrl Pts',(-41.4571701130823,23.9617406441373,173.588390147553));
#15880=CARTESIAN_POINT('Ctrl Pts',(-41.4038900740746,23.9688170570234,173.551685312956));
#15881=CARTESIAN_POINT('Ctrl Pts',(-41.3451279425169,23.9762246763865,173.526200018228));
#15882=CARTESIAN_POINT('',(-41.3451279425171,23.9762246763865,171.485485069079));
#15883=CARTESIAN_POINT('',(-41.3451279425171,23.9762246763865,180.985485069079));
#15884=CARTESIAN_POINT('',(-54.4340581561246,8.06989492938437,171.485485069079));
#15885=CARTESIAN_POINT('Origin',(-39.4690592605811,9.0940082318961,171.485485069079));
#15886=CARTESIAN_POINT('',(-54.4340581561246,8.06989492938437,180.985485069079));
#15887=CARTESIAN_POINT('Origin',(-39.4690592605811,9.0940082318961,180.985485069079));
#15888=CARTESIAN_POINT('',(-54.4340581561246,8.06989492938437,180.485485069079));
#15889=CARTESIAN_POINT('',(-41.3451279425171,23.9762246763865,180.485485069079));
#15890=CARTESIAN_POINT('Origin',(-39.4690592605811,9.0940082318961,180.485485069079));
#15891=CARTESIAN_POINT('',(-41.3451279425171,23.9762246763865,178.444770119931));
#15892=CARTESIAN_POINT('',(-41.3451279425171,23.9762246763865,180.985485069079));
#15893=CARTESIAN_POINT('Ctrl Pts',(-41.3451279425169,23.9762246763865,178.444770119931));
#15894=CARTESIAN_POINT('Ctrl Pts',(-41.3955883597458,23.969863580323,178.422885301067));
#15895=CARTESIAN_POINT('Ctrl Pts',(-41.4421229365782,23.9637326784515,178.392675835198));
#15896=CARTESIAN_POINT('Ctrl Pts',(-41.5305271634123,23.9517560192715,178.311515809307));
#15897=CARTESIAN_POINT('Ctrl Pts',(-41.5692848349094,23.9462751370746,178.258717426295));
#15898=CARTESIAN_POINT('Ctrl Pts',(-41.6126217111684,23.9400646596951,178.166504459593));
#15899=CARTESIAN_POINT('Ctrl Pts',(-41.6245994664793,23.9383240624959,178.131449443898));
#15900=CARTESIAN_POINT('Ctrl Pts',(-41.6406845749615,23.9359794470033,178.059314374365));
#15901=CARTESIAN_POINT('Ctrl Pts',(-41.6447424765058,23.9353829170101,178.022456793883));
#15902=CARTESIAN_POINT('Ctrl Pts',(-41.6447424765058,23.9353829170101,177.985485069079));
#15903=CARTESIAN_POINT('',(-54.4340581561246,8.06989492938437,178.985485069079));
#15904=CARTESIAN_POINT('Origin',(-39.4690592605811,9.0940082318961,178.985485069079));
#15905=CARTESIAN_POINT('',(-54.4340581561246,8.06989492938437,180.985485069079));
#15906=CARTESIAN_POINT('Origin',(-51.4899841053611,-42.5281564925371,175.985485069079));
#15907=CARTESIAN_POINT('',(-60.5935545601082,-98.4662830593508,178.485485069079));
#15908=CARTESIAN_POINT('',(-54.633706038692,-98.6988977036234,178.813912075476));
#15909=CARTESIAN_POINT('Ctrl Pts',(-60.5935545601082,-98.4662830593508,
178.485485069079));
#15910=CARTESIAN_POINT('Ctrl Pts',(-60.3880207695053,-98.4688260755358,
178.741086946021));
#15911=CARTESIAN_POINT('Ctrl Pts',(-60.152209790567,-98.4757252435905,178.970557766682));
#15912=CARTESIAN_POINT('Ctrl Pts',(-59.6240017814705,-98.4925949995657,
179.371542094559));
#15913=CARTESIAN_POINT('Ctrl Pts',(-59.3326632292186,-98.503134685847,179.539996656388));
#15914=CARTESIAN_POINT('Ctrl Pts',(-58.5298830462485,-98.5351183946245,
179.878612357701));
#15915=CARTESIAN_POINT('Ctrl Pts',(-57.9994202067562,-98.5589973863814,
179.98575755042));
#15916=CARTESIAN_POINT('Ctrl Pts',(-56.948798132757,-98.6112255589572,179.985221824441));
#15917=CARTESIAN_POINT('Ctrl Pts',(-56.4382579068318,-98.6342747561005,
179.885486106302));
#15918=CARTESIAN_POINT('Ctrl Pts',(-55.4642502766152,-98.673456639198,179.49070605567));
#15919=CARTESIAN_POINT('Ctrl Pts',(-55.0130604929058,-98.6888974774772,
179.192189168768));
#15920=CARTESIAN_POINT('Ctrl Pts',(-54.6337060386916,-98.6988977036235,
178.813912075475));
#15921=CARTESIAN_POINT('',(-54.580703036468,-98.2017149587949,178.813912075476));
#15922=CARTESIAN_POINT('',(-48.6774936648204,-42.82798676345,178.813912075476));
#15923=CARTESIAN_POINT('',(-60.5405515578841,-97.9691003145223,178.485485069079));
#15924=CARTESIAN_POINT('Ctrl Pts',(-54.580703036468,-98.2017149587947,178.813912075476));
#15925=CARTESIAN_POINT('Ctrl Pts',(-54.9600551075263,-98.1917147954715,
179.19218679238));
#15926=CARTESIAN_POINT('Ctrl Pts',(-55.4112503915159,-98.1762737685919,
179.490707319102));
#15927=CARTESIAN_POINT('Ctrl Pts',(-56.3852549043046,-98.1370920116987,
179.88548610616));
#15928=CARTESIAN_POINT('Ctrl Pts',(-56.8957951303142,-98.1140428141397,
179.985221824425));
#15929=CARTESIAN_POINT('Ctrl Pts',(-57.946417204408,-98.0618146415591,179.985757550436));
#15930=CARTESIAN_POINT('Ctrl Pts',(-58.4768800438985,-98.0379356498009,
179.878612357734));
#15931=CARTESIAN_POINT('Ctrl Pts',(-59.279658681122,-98.005952002607,179.539997308455));
#15932=CARTESIAN_POINT('Ctrl Pts',(-59.5709958684452,-97.9954123600177,
179.371543778558));
#15933=CARTESIAN_POINT('Ctrl Pts',(-60.099201714192,-97.9785426487718,178.970562132848));
#15934=CARTESIAN_POINT('Ctrl Pts',(-60.335018812839,-97.9716433177709,178.741085645765));
#15935=CARTESIAN_POINT('Ctrl Pts',(-60.5405515578841,-97.9691003145223,
178.485485069079));
#15936=CARTESIAN_POINT('',(-54.5948893516535,-42.1971528497386,178.485485069079));
#15937=CARTESIAN_POINT('',(-54.5948893516535,-42.1971528497386,178.485485069079));
#15938=CARTESIAN_POINT('',(-48.3850788590687,-42.8591601353355,178.485485069079));
#15939=CARTESIAN_POINT('Origin',(-51.4899841053611,-42.5281564925371,175.985485069079));
#15940=CARTESIAN_POINT('',(-50.7024802268255,-64.597022606232,178.485485069079));
#15941=CARTESIAN_POINT('',(-48.3850788590687,-42.8591601353355,178.485485069079));
#15942=CARTESIAN_POINT('',(-51.1888180761633,-76.238457947575,176.985485069122));
#15943=CARTESIAN_POINT('Ctrl Pts',(-51.1888180761633,-76.238457947575,176.985485069122));
#15944=CARTESIAN_POINT('Ctrl Pts',(-51.2021305879066,-76.3214937428782,
177.002667010649));
#15945=CARTESIAN_POINT('Ctrl Pts',(-51.2156898705536,-76.4043562432359,
177.020272310541));
#15946=CARTESIAN_POINT('Ctrl Pts',(-51.2295466744237,-76.4869415706103,
177.038591562764));
#15947=CARTESIAN_POINT('Ctrl Pts',(-51.2428693654739,-76.5663436327459,
177.056204696349));
#15948=CARTESIAN_POINT('Ctrl Pts',(-51.2564667204762,-76.6454895294908,
177.074478125875));
#15949=CARTESIAN_POINT('Ctrl Pts',(-51.2704287680282,-76.7242798841604,
177.093677810158));
#15950=CARTESIAN_POINT('Ctrl Pts',(-51.2834506181271,-76.7977645348837,
177.111584597091));
#15951=CARTESIAN_POINT('Ctrl Pts',(-51.2967895433251,-76.8709399358143,
177.130297444209));
#15952=CARTESIAN_POINT('Ctrl Pts',(-51.3105617329162,-76.9437187503107,
177.15003421173));
#15953=CARTESIAN_POINT('Ctrl Pts',(-51.3223585263326,-77.0060586298211,
177.166940061566));
#15954=CARTESIAN_POINT('Ctrl Pts',(-51.3344736028237,-77.0681074686509,
177.184597395297));
#15955=CARTESIAN_POINT('Ctrl Pts',(-51.3470101229251,-77.1298057199427,
177.20314103713));
#15956=CARTESIAN_POINT('Ctrl Pts',(-51.3557988119162,-77.1730590898982,
177.216141000399));
#15957=CARTESIAN_POINT('Ctrl Pts',(-51.364781415635,-77.2161774090964,177.229465123715));
#15958=CARTESIAN_POINT('Ctrl Pts',(-51.3740444012484,-77.2590260001929,
177.243492025122));
#15959=CARTESIAN_POINT('Ctrl Pts',(-51.3828789589595,-77.2998927754084,
177.256870159901));
#15960=CARTESIAN_POINT('Ctrl Pts',(-51.3919681872068,-77.3405142529802,
177.270887849947));
#15961=CARTESIAN_POINT('Ctrl Pts',(-51.401432215628,-77.3807665395897,177.285874813254));
#15962=CARTESIAN_POINT('Ctrl Pts',(-51.4101714388937,-77.4179360940314,
177.299713995956));
#15963=CARTESIAN_POINT('Ctrl Pts',(-51.4192300650648,-77.4547908693569,
177.314379973633));
#15964=CARTESIAN_POINT('Ctrl Pts',(-51.4287456836206,-77.4912266116723,
177.330129441093));
#15965=CARTESIAN_POINT('Ctrl Pts',(-51.4345017021272,-77.5132666720046,
177.339656328456));
#15966=CARTESIAN_POINT('Ctrl Pts',(-51.4404257743927,-77.5351532749502,
177.349579610017));
#15967=CARTESIAN_POINT('Ctrl Pts',(-51.4465575779221,-77.5568619102505,
177.359954660612));
#15968=CARTESIAN_POINT('Ctrl Pts',(-51.4526736736208,-77.5785149345768,
177.370303133458));
#15969=CARTESIAN_POINT('Ctrl Pts',(-51.4590189397432,-77.6002653389843,
177.38103395459));
#15970=CARTESIAN_POINT('Ctrl Pts',(-51.4656713009053,-77.6215697467313,
177.392576424021));
#15971=CARTESIAN_POINT('Ctrl Pts',(-51.4719423749727,-77.6416530698833,
177.403457324646));
#15972=CARTESIAN_POINT('Ctrl Pts',(-51.4784859081488,-77.6613401262172,
177.415059786582));
#15973=CARTESIAN_POINT('Ctrl Pts',(-51.485411326381,-77.6801687747737,177.427738660107));
#15974=CARTESIAN_POINT('Ctrl Pts',(-51.491747978897,-77.6973967022792,177.439339636846));
#15975=CARTESIAN_POINT('Ctrl Pts',(-51.4984041162443,-77.7139060095734,
177.4518420813));
#15976=CARTESIAN_POINT('Ctrl Pts',(-51.5055059785157,-77.7293360108029,
177.465509726159));
#15977=CARTESIAN_POINT('Ctrl Pts',(-51.5084960109055,-77.7358323636871,
177.471264090192));
#15978=CARTESIAN_POINT('Ctrl Pts',(-51.5115656173302,-77.7421373112703,
177.47722486705));
#15979=CARTESIAN_POINT('Ctrl Pts',(-51.5147269509126,-77.7482235053492,
177.483411011986));
#15980=CARTESIAN_POINT('Ctrl Pts',(-51.5232794127367,-77.7646886904234,
177.500146597468));
#15981=CARTESIAN_POINT('Ctrl Pts',(-51.5327381680121,-77.7794241002675,
177.519242344142));
#15982=CARTESIAN_POINT('Ctrl Pts',(-51.5425320619611,-77.7882308246434,
177.540116101265));
#15983=CARTESIAN_POINT('Ctrl Pts',(-51.5485309012701,-77.7936250145994,
177.552901446441));
#15984=CARTESIAN_POINT('Ctrl Pts',(-51.5546552639884,-77.7967949768587,
177.566353184388));
#15985=CARTESIAN_POINT('Ctrl Pts',(-51.5607652634837,-77.7967769698663,
177.580332016632));
#15986=CARTESIAN_POINT('Ctrl Pts',(-51.5673406412735,-77.7967575913413,
177.595375569931));
#15987=CARTESIAN_POINT('Ctrl Pts',(-51.5734029435428,-77.7927425070794,
177.609994002081));
#15988=CARTESIAN_POINT('Ctrl Pts',(-51.5789129584608,-77.786000814162,177.623796257218));
#15989=CARTESIAN_POINT('Ctrl Pts',(-51.5850074273648,-77.7785440216746,
177.639062534351));
#15990=CARTESIAN_POINT('Ctrl Pts',(-51.5904257027035,-77.7677515886449,
177.653329863453));
#15991=CARTESIAN_POINT('Ctrl Pts',(-51.5950548021663,-77.7553505852216,
177.666095526557));
#15992=CARTESIAN_POINT('Ctrl Pts',(-51.5964787378413,-77.7515359704523,
177.670022312588));
#15993=CARTESIAN_POINT('Ctrl Pts',(-51.5978276539958,-77.7475692084199,
177.673807202938));
#15994=CARTESIAN_POINT('Ctrl Pts',(-51.5990975017122,-77.7435006940469,
177.677436042246));
#15995=CARTESIAN_POINT('Ctrl Pts',(-51.6038775271175,-77.7281857851694,
177.691095903863));
#15996=CARTESIAN_POINT('Ctrl Pts',(-51.6079935240033,-77.7117519853323,
177.703326388188));
#15997=CARTESIAN_POINT('Ctrl Pts',(-51.6115435129349,-77.6945144134463,
177.714453362138));
#15998=CARTESIAN_POINT('Ctrl Pts',(-51.6153029287069,-77.6762599341032,
177.726236757007));
#15999=CARTESIAN_POINT('Ctrl Pts',(-51.618428308146,-77.6571039402551,177.736782793592));
#16000=CARTESIAN_POINT('Ctrl Pts',(-51.6210961780892,-77.6374112528145,
177.746464371838));
#16001=CARTESIAN_POINT('Ctrl Pts',(-51.6240034009094,-77.6159517995671,
177.757014550748));
#16002=CARTESIAN_POINT('Ctrl Pts',(-51.6263678480769,-77.5938549565873,
177.766538360512));
#16003=CARTESIAN_POINT('Ctrl Pts',(-51.6284773090603,-77.5715834420731,
177.775499096543));
#16004=CARTESIAN_POINT('Ctrl Pts',(-51.62958722901,-77.5598649990846,177.780213902724));
#16005=CARTESIAN_POINT('Ctrl Pts',(-51.6306274481688,-77.5480980575388,
177.784772501055));
#16006=CARTESIAN_POINT('Ctrl Pts',(-51.6316450558895,-77.5363491979955,
177.789240317579));
#16007=CARTESIAN_POINT('Ctrl Pts',(-51.6345785013937,-77.5024809022792,
177.802119638392));
#16008=CARTESIAN_POINT('Ctrl Pts',(-51.6369806567888,-77.4682654516565,
177.8138359583));
#16009=CARTESIAN_POINT('Ctrl Pts',(-51.6389709535977,-77.4337999799066,
177.824711738984));
#16010=CARTESIAN_POINT('Ctrl Pts',(-51.6411016541027,-77.3969031724893,
177.836354741822));
#16011=CARTESIAN_POINT('Ctrl Pts',(-51.642760815162,-77.3597197547319,177.847034606129));
#16012=CARTESIAN_POINT('Ctrl Pts',(-51.6441487479128,-77.3223603097426,
177.857125713464));
#16013=CARTESIAN_POINT('Ctrl Pts',(-51.6442939346125,-77.318452271319,177.858181308247));
#16014=CARTESIAN_POINT('Ctrl Pts',(-51.6444361951343,-77.314542299998,177.859230441347));
#16015=CARTESIAN_POINT('Ctrl Pts',(-51.6445757869095,-77.3106305178212,
177.860273527955));
#16016=CARTESIAN_POINT('Ctrl Pts',(-51.646532188841,-77.2558062404107,177.874892560132));
#16017=CARTESIAN_POINT('Ctrl Pts',(-51.6479312585446,-77.2005791231423,
177.888296102344));
#16018=CARTESIAN_POINT('Ctrl Pts',(-51.6488633782082,-77.1450897561686,
177.900765991515));
#16019=CARTESIAN_POINT('Ctrl Pts',(-51.6498609622602,-77.085703274256,177.914111662732));
#16020=CARTESIAN_POINT('Ctrl Pts',(-51.6503241286654,-77.0260163532741,
177.926388205594));
#16021=CARTESIAN_POINT('Ctrl Pts',(-51.6504193884841,-76.966192392791,177.937917077868));
#16022=CARTESIAN_POINT('Ctrl Pts',(-51.6504826689159,-76.9264517539148,
177.945575627153));
#16023=CARTESIAN_POINT('Ctrl Pts',(-51.6503847250362,-76.8866504601454,
177.95290372211));
#16024=CARTESIAN_POINT('Ctrl Pts',(-51.6501852172071,-76.8468346421424,
177.959989646563));
#16025=CARTESIAN_POINT('Ctrl Pts',(-51.6497395509928,-76.7578929451445,
177.975818384418));
#16026=CARTESIAN_POINT('Ctrl Pts',(-51.6487423505584,-76.6688263647255,
177.990398012595));
#16027=CARTESIAN_POINT('Ctrl Pts',(-51.6472480837277,-76.5796659014834,
178.0039885827));
#16028=CARTESIAN_POINT('Ctrl Pts',(-51.6456937152051,-76.4869192683657,
178.018125786271));
#16029=CARTESIAN_POINT('Ctrl Pts',(-51.6436020909363,-76.3940709627132,
178.03119298766));
#16030=CARTESIAN_POINT('Ctrl Pts',(-51.6410857399421,-76.3011475515338,
178.043456674307));
#16031=CARTESIAN_POINT('Ctrl Pts',(-51.6384292049469,-76.2030474477577,
178.056403561614));
#16032=CARTESIAN_POINT('Ctrl Pts',(-51.6352997717696,-76.1048635740488,
178.068455130834));
#16033=CARTESIAN_POINT('Ctrl Pts',(-51.6318773801508,-76.0066192617694,
178.079892775063));
#16034=CARTESIAN_POINT('Ctrl Pts',(-51.6307428227353,-75.9740502791856,
178.083684469738));
#16035=CARTESIAN_POINT('Ctrl Pts',(-51.6295764095476,-75.9414745967699,
178.087408430568));
#16036=CARTESIAN_POINT('Ctrl Pts',(-51.6283856383612,-75.9088929032812,
178.091074131322));
#16037=CARTESIAN_POINT('Ctrl Pts',(-51.6230479302402,-75.762843375106,178.107505869769));
#16038=CARTESIAN_POINT('Ctrl Pts',(-51.617133671971,-75.6166509425742,178.122695645834));
#16039=CARTESIAN_POINT('Ctrl Pts',(-51.6106720679446,-75.4703596661805,
178.13686703474));
#16040=CARTESIAN_POINT('Ctrl Pts',(-51.603825778809,-75.3153590854994,178.151882103059));
#16041=CARTESIAN_POINT('Ctrl Pts',(-51.5963654529363,-75.1602474897245,
178.165754310024));
#16042=CARTESIAN_POINT('Ctrl Pts',(-51.5883753887386,-75.005069113572,178.178719571855));
#16043=CARTESIAN_POINT('Ctrl Pts',(-51.5799333134435,-74.8411120409846,
178.192418299912));
#16044=CARTESIAN_POINT('Ctrl Pts',(-51.5709003709617,-74.6770803555337,
178.205104877183));
#16045=CARTESIAN_POINT('Ctrl Pts',(-51.5614222526274,-74.5130183020776,
178.217019375693));
#16046=CARTESIAN_POINT('Ctrl Pts',(-51.5519949464334,-74.3498357843876,
178.228870000643));
#16047=CARTESIAN_POINT('Ctrl Pts',(-51.5421279869841,-74.1866231105131,
178.239956676937));
#16048=CARTESIAN_POINT('Ctrl Pts',(-51.5319988666506,-74.0234176542754,
178.250478142846));
#16049=CARTESIAN_POINT('Ctrl Pts',(-51.5178618990269,-73.7956357566507,
178.265162697675));
#16050=CARTESIAN_POINT('Ctrl Pts',(-51.5030623270387,-73.5678777386058,
178.278645978382));
#16051=CARTESIAN_POINT('Ctrl Pts',(-51.487657634943,-73.3401462751523,178.291141952504));
#16052=CARTESIAN_POINT('Ctrl Pts',(-51.4714916117283,-73.1011598610119,
178.304255503004));
#16053=CARTESIAN_POINT('Ctrl Pts',(-51.4546597605595,-72.8622026182683,
178.316282066724));
#16054=CARTESIAN_POINT('Ctrl Pts',(-51.4372695238474,-72.6232703614539,
178.327427903459));
#16055=CARTESIAN_POINT('Ctrl Pts',(-51.4254590327489,-72.461000730569,178.334997541971));
#16056=CARTESIAN_POINT('Ctrl Pts',(-51.4133918338923,-72.2987424737129,
178.342160074865));
#16057=CARTESIAN_POINT('Ctrl Pts',(-51.4011095455939,-72.1364927659349,
178.348969236345));
#16058=CARTESIAN_POINT('Ctrl Pts',(-51.3768673720191,-71.8162523121323,
178.362408822721));
#16059=CARTESIAN_POINT('Ctrl Pts',(-51.3517889968695,-71.4960451991844,
178.374473831145));
#16060=CARTESIAN_POINT('Ctrl Pts',(-51.325910214073,-71.175876660519,178.385374291189));
#16061=CARTESIAN_POINT('Ctrl Pts',(-51.299237757716,-70.8458889079437,178.396609056251));
#16062=CARTESIAN_POINT('Ctrl Pts',(-51.2717158347394,-70.5159420263348,
178.406606963097));
#16063=CARTESIAN_POINT('Ctrl Pts',(-51.2434204705399,-70.1860349960978,
178.415554089733));
#16064=CARTESIAN_POINT('Ctrl Pts',(-51.2138284065372,-69.8410092213846,
178.424911238918));
#16065=CARTESIAN_POINT('Ctrl Pts',(-51.1833911427243,-69.4960269329799,
178.433119311743));
#16066=CARTESIAN_POINT('Ctrl Pts',(-51.1522232776757,-69.1510812999414,
178.440340314044));
#16067=CARTESIAN_POINT('Ctrl Pts',(-51.1285558932623,-68.8891461020658,
178.445823597453));
#16068=CARTESIAN_POINT('Ctrl Pts',(-51.1044678762701,-68.6272319106942,
178.45073662802));
#16069=CARTESIAN_POINT('Ctrl Pts',(-51.0800153847959,-68.3653342504166,
178.455131374877));
#16070=CARTESIAN_POINT('Ctrl Pts',(-51.0392670697878,-67.9289006717707,
178.462454903829));
#16071=CARTESIAN_POINT('Ctrl Pts',(-50.9974328843074,-67.4925218290922,
178.468324733422));
#16072=CARTESIAN_POINT('Ctrl Pts',(-50.9545694977588,-67.0561972253282,
178.472891592671));
#16073=CARTESIAN_POINT('Ctrl Pts',(-50.909938769321,-66.601882098378,178.477646752527));
#16074=CARTESIAN_POINT('Ctrl Pts',(-50.8641932062194,-66.1476256195205,
178.480989278531));
#16075=CARTESIAN_POINT('Ctrl Pts',(-50.8174078822645,-65.6934241972506,
178.483034538648));
#16076=CARTESIAN_POINT('Ctrl Pts',(-50.8061241485162,-65.5838794194492,
178.483527816639));
#16077=CARTESIAN_POINT('Ctrl Pts',(-50.7947799440958,-65.4743378370309,
178.483945395322));
#16078=CARTESIAN_POINT('Ctrl Pts',(-50.7833763168631,-65.36479939044,178.484288448851));
#16079=CARTESIAN_POINT('Ctrl Pts',(-50.7567311311835,-65.1088569443284,
178.485090011792));
#16080=CARTESIAN_POINT('Ctrl Pts',(-50.7297618268952,-64.852931521511,178.485485016653));
#16081=CARTESIAN_POINT('Ctrl Pts',(-50.7024802268255,-64.597022606232,178.485485069074));
#16082=CARTESIAN_POINT('',(-51.1887931847522,-76.2384284136363,174.985485069079));
#16083=CARTESIAN_POINT('Ctrl Pts',(-51.1887978133155,-76.2384598819686,
176.985483211559));
#16084=CARTESIAN_POINT('Ctrl Pts',(-51.168723086379,-76.1132573740385,176.959575232915));
#16085=CARTESIAN_POINT('Ctrl Pts',(-51.1477303137464,-75.982626364191,176.931299532441));
#16086=CARTESIAN_POINT('Ctrl Pts',(-51.1263778064616,-75.8500958709827,
176.900742946067));
#16087=CARTESIAN_POINT('Ctrl Pts',(-51.1052284580587,-75.7188263419536,
176.870477090979));
#16088=CARTESIAN_POINT('Ctrl Pts',(-51.0837261817287,-75.5856934803233,
176.837973546585));
#16089=CARTESIAN_POINT('Ctrl Pts',(-51.0624157913829,-75.4540754929927,
176.803316693716));
#16090=CARTESIAN_POINT('Ctrl Pts',(-51.0406184711992,-75.3194501123587,
176.76786795222));
#16091=CARTESIAN_POINT('Ctrl Pts',(-51.0190219083614,-75.1864096200007,
176.730166374361));
#16092=CARTESIAN_POINT('Ctrl Pts',(-50.9982115787268,-75.0585136716332,
176.690302258296));
#16093=CARTESIAN_POINT('Ctrl Pts',(-50.9897004353455,-75.0062059584184,
176.673998373949));
#16094=CARTESIAN_POINT('Ctrl Pts',(-50.9813208328539,-74.9547581431755,
176.657332761972));
#16095=CARTESIAN_POINT('Ctrl Pts',(-50.9731129323308,-74.9044112818398,
176.640311599764));
#16096=CARTESIAN_POINT('Ctrl Pts',(-50.9581672362543,-74.8127351113248,
176.609317910633));
#16097=CARTESIAN_POINT('Ctrl Pts',(-50.9428274715336,-74.7188051428769,
176.575173825758));
#16098=CARTESIAN_POINT('Ctrl Pts',(-50.927879342889,-74.6274317515189,176.538057900926));
#16099=CARTESIAN_POINT('Ctrl Pts',(-50.9119396002641,-74.5299969236798,
176.498479817063));
#16100=CARTESIAN_POINT('Ctrl Pts',(-50.8964451777353,-74.4354691361771,
176.45552252949));
#16101=CARTESIAN_POINT('Ctrl Pts',(-50.8823514823103,-74.3496185699138,
176.409402537941));
#16102=CARTESIAN_POINT('Ctrl Pts',(-50.8756807371488,-74.3089842839974,
176.387573294354));
#16103=CARTESIAN_POINT('Ctrl Pts',(-50.869323829929,-74.2702930463482,176.365035522011));
#16104=CARTESIAN_POINT('Ctrl Pts',(-50.8633822358648,-74.2341528138115,
176.341812177418));
#16105=CARTESIAN_POINT('Ctrl Pts',(-50.8548047188014,-74.1819793637386,
176.308286050866));
#16106=CARTESIAN_POINT('Ctrl Pts',(-50.8459342959469,-74.1280817181684,
176.268790272864));
#16107=CARTESIAN_POINT('Ctrl Pts',(-50.8383519847354,-74.0820498566621,
176.224327986109));
#16108=CARTESIAN_POINT('Ctrl Pts',(-50.8362284960464,-74.069158254812,176.211875956592));
#16109=CARTESIAN_POINT('Ctrl Pts',(-50.8342060519672,-74.05688325133,176.199034390808));
#16110=CARTESIAN_POINT('Ctrl Pts',(-50.8323194103639,-74.0454348151833,
176.185825323489));
#16111=CARTESIAN_POINT('Ctrl Pts',(-50.827864840102,-74.018403786549,176.154637249209));
#16112=CARTESIAN_POINT('Ctrl Pts',(-50.8239090771887,-73.9944144112031,
176.119612333733));
#16113=CARTESIAN_POINT('Ctrl Pts',(-50.821298479485,-73.9785862257575,176.081298694509));
#16114=CARTESIAN_POINT('Ctrl Pts',(-50.8193532731165,-73.9667923415113,
176.052750467827));
#16115=CARTESIAN_POINT('Ctrl Pts',(-50.8181944769487,-73.9597687273717,
176.022964685054));
#16116=CARTESIAN_POINT('Ctrl Pts',(-50.8180506457443,-73.9588968877778,
175.992027399553));
#16117=CARTESIAN_POINT('Ctrl Pts',(-50.817908130518,-73.9580330250466,175.961373173548));
#16118=CARTESIAN_POINT('Ctrl Pts',(-50.818771419997,-73.9632653488002,175.931596917882));
#16119=CARTESIAN_POINT('Ctrl Pts',(-50.8204678882598,-73.9735504690026,
175.902755935248));
#16120=CARTESIAN_POINT('Ctrl Pts',(-50.8226211501266,-73.9866049761884,
175.866149186116));
#16121=CARTESIAN_POINT('Ctrl Pts',(-50.8260344374881,-74.0073021325509,
175.832457982263));
#16122=CARTESIAN_POINT('Ctrl Pts',(-50.8299972977936,-74.0313451228971,
175.80212682161));
#16123=CARTESIAN_POINT('Ctrl Pts',(-50.8362737302612,-74.0694247405445,
175.754087913644));
#16124=CARTESIAN_POINT('Ctrl Pts',(-50.8443796156014,-74.1186360495895,
175.711069473412));
#16125=CARTESIAN_POINT('Ctrl Pts',(-50.8526027993114,-74.1686130255098,
175.674187743685));
#16126=CARTESIAN_POINT('Ctrl Pts',(-50.8539198545757,-74.1766175212803,
175.668280630576));
#16127=CARTESIAN_POINT('Ctrl Pts',(-50.8552399236702,-74.1846415471193,
175.662530938822));
#16128=CARTESIAN_POINT('Ctrl Pts',(-50.8565559779939,-74.1926423775393,
175.6569432546));
#16129=CARTESIAN_POINT('Ctrl Pts',(-50.868899714928,-74.2676849834404,175.604534396648));
#16130=CARTESIAN_POINT('Ctrl Pts',(-50.8833664041038,-74.3557461756237,
175.555830160403));
#16131=CARTESIAN_POINT('Ctrl Pts',(-50.898709234606,-74.449322863261,175.511142903759));
#16132=CARTESIAN_POINT('Ctrl Pts',(-50.9122347199158,-74.5318154720261,
175.471748814567));
#16133=CARTESIAN_POINT('Ctrl Pts',(-50.9264410802539,-74.6185943708312,
175.435476448387));
#16134=CARTESIAN_POINT('Ctrl Pts',(-50.9404762908346,-74.7044702872778,
175.40253979577));
#16135=CARTESIAN_POINT('Ctrl Pts',(-50.9423621250129,-74.7160089626255,
175.398114278613));
#16136=CARTESIAN_POINT('Ctrl Pts',(-50.9442448726816,-74.727531258289,175.393748983833));
#16137=CARTESIAN_POINT('Ctrl Pts',(-50.9461224701891,-74.7390245137205,
175.389444430525));
#16138=CARTESIAN_POINT('Ctrl Pts',(-50.9649625531635,-74.8543494889124,
175.346251924598));
#16139=CARTESIAN_POINT('Ctrl Pts',(-50.9850447742112,-74.977532800152,175.305189767046));
#16140=CARTESIAN_POINT('Ctrl Pts',(-51.0057593748162,-75.1049143140581,
175.266364772338));
#16141=CARTESIAN_POINT('Ctrl Pts',(-51.0260059583032,-75.2294178227266,
175.228416973502));
#16142=CARTESIAN_POINT('Ctrl Pts',(-51.0468566504168,-75.3579323481973,
175.192606388452));
#16143=CARTESIAN_POINT('Ctrl Pts',(-51.0677442194091,-75.4869918763851,
175.159032754036));
#16144=CARTESIAN_POINT('Ctrl Pts',(-51.0888832841532,-75.6176053395035,
175.125054877919));
#16145=CARTESIAN_POINT('Ctrl Pts',(-51.1100601094042,-75.7487771848276,
175.093368144521));
#16146=CARTESIAN_POINT('Ctrl Pts',(-51.1306891566218,-75.876859965402,175.064075936874));
#16147=CARTESIAN_POINT('Ctrl Pts',(-51.1507544538042,-76.0014425032698,
175.035584225871));
#16148=CARTESIAN_POINT('Ctrl Pts',(-51.1703015295575,-76.1231018808035,
175.009357953825));
#16149=CARTESIAN_POINT('Ctrl Pts',(-51.1887936826668,-76.2384341198503,
174.985492257536));
#16150=CARTESIAN_POINT('',(-50.7024802268295,-64.5970226062537,173.485485069079));
#16151=CARTESIAN_POINT('Ctrl Pts',(-50.7024802268248,-64.5970226062542,
173.485485069085));
#16152=CARTESIAN_POINT('Ctrl Pts',(-50.9643032922535,-67.0529990415413,
173.485485603988));
#16153=CARTESIAN_POINT('Ctrl Pts',(-51.218469484852,-69.7245979498243,173.520841304362));
#16154=CARTESIAN_POINT('Ctrl Pts',(-51.4912169004962,-73.3272878136435,
173.671974926571));
#16155=CARTESIAN_POINT('Ctrl Pts',(-51.7170878156646,-76.636174896363,173.822575916535));
#16156=CARTESIAN_POINT('Ctrl Pts',(-51.6237538197336,-77.6203204977443,
174.215041830701));
#16157=CARTESIAN_POINT('Ctrl Pts',(-51.6154076427636,-77.6830014132838,
174.245424370326));
#16158=CARTESIAN_POINT('Ctrl Pts',(-51.5981975764625,-77.7480985755699,
174.296408211552));
#16159=CARTESIAN_POINT('Ctrl Pts',(-51.5917351323593,-77.7667510220376,
174.314500312631));
#16160=CARTESIAN_POINT('Ctrl Pts',(-51.5786277845437,-77.7877830295759,
174.348195468307));
#16161=CARTESIAN_POINT('Ctrl Pts',(-51.5729256033243,-77.7935256381876,
174.362246416503));
#16162=CARTESIAN_POINT('Ctrl Pts',(-51.5609350615783,-77.7976939764001,
174.390403091874));
#16163=CARTESIAN_POINT('Ctrl Pts',(-51.5551546562069,-77.796735277411,174.403455794326));
#16164=CARTESIAN_POINT('Ctrl Pts',(-51.5420841811777,-77.7889989352672,
174.432006923496));
#16165=CARTESIAN_POINT('Ctrl Pts',(-51.5350614462774,-77.7811412466012,
174.446707746341));
#16166=CARTESIAN_POINT('Ctrl Pts',(-51.5167709889332,-77.7544514481327,
174.4839390495));
#16167=CARTESIAN_POINT('Ctrl Pts',(-51.5056242119341,-77.7306696787344,
174.505354751846));
#16168=CARTESIAN_POINT('Ctrl Pts',(-51.4723854079891,-77.6487073114297,
174.567396292195));
#16169=CARTESIAN_POINT('Ctrl Pts',(-51.449199025989,-77.5696294940345,174.607070508007));
#16170=CARTESIAN_POINT('Ctrl Pts',(-51.3451043426313,-77.1694577561508,
174.778180690935));
#16171=CARTESIAN_POINT('Ctrl Pts',(-51.255403237339,-76.6537518959946,174.899487153725));
#16172=CARTESIAN_POINT('Ctrl Pts',(-51.1888118575074,-76.2384181515047,
174.985415709881));
#16173=CARTESIAN_POINT('',(-48.3850788590687,-42.8591601353355,173.485485069079));
#16174=CARTESIAN_POINT('',(-48.3850788590687,-42.8591601353355,173.485485069079));
#16175=CARTESIAN_POINT('',(-54.5948893516535,-42.1971528497386,173.485485069079));
#16176=CARTESIAN_POINT('Origin',(-51.4899841053611,-42.5281564925371,175.985485069079));
#16177=CARTESIAN_POINT('',(-60.5749026458094,-98.2913229710871,173.485485069079));
#16178=CARTESIAN_POINT('',(-54.5948893516535,-42.1971528497386,173.485485069079));
#16179=CARTESIAN_POINT('',(-60.6995605645563,-99.4606485490079,178.485485069079));
#16180=CARTESIAN_POINT('Ctrl Pts',(-60.5749026458094,-98.2913229710871,
173.485485069079));
#16181=CARTESIAN_POINT('Ctrl Pts',(-60.3843342578436,-98.3299608318209,
173.243690644989));
#16182=CARTESIAN_POINT('Ctrl Pts',(-60.1664113055595,-98.3704554623929,
173.025230159753));
#16183=CARTESIAN_POINT('Ctrl Pts',(-59.6797951404782,-98.4594953210885,
172.639492409097));
#16184=CARTESIAN_POINT('Ctrl Pts',(-59.4118189594528,-98.507396166173,172.474839570992));
#16185=CARTESIAN_POINT('Ctrl Pts',(-58.6475696307461,-98.6412135625171,
172.12302034014));
#16186=CARTESIAN_POINT('Ctrl Pts',(-58.1285326590571,-98.7293077079875,
172.001630150343));
#16187=CARTESIAN_POINT('Ctrl Pts',(-57.0934944411569,-98.8999216213785,
171.972905197423));
#16188=CARTESIAN_POINT('Ctrl Pts',(-56.5880866935318,-98.9843175007548,
172.057860325957));
#16189=CARTESIAN_POINT('Ctrl Pts',(-55.6187428548676,-99.1521396670418,
172.423693545831));
#16190=CARTESIAN_POINT('Ctrl Pts',(-55.1668789617469,-99.2330770981518,
172.708357719645));
#16191=CARTESIAN_POINT('Ctrl Pts',(-54.4152301073058,-99.3735193085268,
173.42678745864));
#16192=CARTESIAN_POINT('Ctrl Pts',(-54.117636559382,-99.4356985494873,173.847812184324));
#16193=CARTESIAN_POINT('Ctrl Pts',(-53.6961108373074,-99.5440869286819,
174.784491901195));
#16194=CARTESIAN_POINT('Ctrl Pts',(-53.5772634151522,-99.5885264630858,
175.29189396112));
#16195=CARTESIAN_POINT('Ctrl Pts',(-53.5376636121844,-99.6533071133646,
176.336975547334));
#16196=CARTESIAN_POINT('Ctrl Pts',(-53.6220957342369,-99.6753461866961,
176.86477871382));
#16197=CARTESIAN_POINT('Ctrl Pts',(-53.9867706921353,-99.7008570794232,
177.847215661255));
#16198=CARTESIAN_POINT('Ctrl Pts',(-54.2591330424856,-99.7036171849942,
178.293920024946));
#16199=CARTESIAN_POINT('Ctrl Pts',(-54.9652132353756,-99.688957954165,179.067651982994));
#16200=CARTESIAN_POINT('Ctrl Pts',(-55.3955739876124,-99.6740155440745,
179.384324188019));
#16201=CARTESIAN_POINT('Ctrl Pts',(-56.3444317593121,-99.6372231709392,
179.82771784559));
#16202=CARTESIAN_POINT('Ctrl Pts',(-56.8518377636485,-99.6149533982737,
179.954069319539));
#16203=CARTESIAN_POINT('Ctrl Pts',(-57.8965798954297,-99.5642480107107,
180.007121753964));
#16204=CARTESIAN_POINT('Ctrl Pts',(-58.4243189790396,-99.5388174118719,
179.929254775814));
#16205=CARTESIAN_POINT('Ctrl Pts',(-59.2732803979538,-99.5037201258886,
179.625522348307));
#16206=CARTESIAN_POINT('Ctrl Pts',(-59.6053345182171,-99.4912868821982,
179.451477802644));
#16207=CARTESIAN_POINT('Ctrl Pts',(-60.2050026582842,-99.4715409050409,
179.021596162725));
#16208=CARTESIAN_POINT('Ctrl Pts',(-60.4709693041988,-99.4634768492749,
178.769761221572));
#16209=CARTESIAN_POINT('Ctrl Pts',(-60.6995605645563,-99.4606485490079,
178.485485069079));
#16210=CARTESIAN_POINT('',(-54.5948893516535,-42.1971528497386,178.485485069079));
#16211=CARTESIAN_POINT('Origin',(-51.4899841053611,-42.5281564925371,175.985485069079));
#16212=CARTESIAN_POINT('',(-60.7525635667804,-99.9578312938364,178.485485069079));
#16213=CARTESIAN_POINT('',(-60.6279056480334,-98.7885057159157,173.485485069079));
#16214=CARTESIAN_POINT('Ctrl Pts',(-60.7525635667804,-99.9578312938363,
178.485485069079));
#16215=CARTESIAN_POINT('Ctrl Pts',(-60.5471423783721,-99.9603729168234,
178.740946913902));
#16216=CARTESIAN_POINT('Ctrl Pts',(-60.3114768367406,-99.9672665268891,
178.970306818076));
#16217=CARTESIAN_POINT('Ctrl Pts',(-59.7836134097214,-99.984122670903,179.371140823409));
#16218=CARTESIAN_POINT('Ctrl Pts',(-59.4924716081514,-99.9946533930933,
179.539560425843));
#16219=CARTESIAN_POINT('Ctrl Pts',(-58.689917777404,-100.026622058121,179.878337837155));
#16220=CARTESIAN_POINT('Ctrl Pts',(-58.1594421477247,-100.050492208668,
179.985627564123));
#16221=CARTESIAN_POINT('Ctrl Pts',(-57.1087945616306,-100.102727643745,
179.98534767287));
#16222=CARTESIAN_POINT('Ctrl Pts',(-56.598242490745,-100.125780453932,179.885741010665));
#16223=CARTESIAN_POINT('Ctrl Pts',(-55.6234756153487,-100.164999588288,
179.490939604252));
#16224=CARTESIAN_POINT('Ctrl Pts',(-55.1718628664936,-100.180456631909,
179.192079540234));
#16225=CARTESIAN_POINT('Ctrl Pts',(-54.4271820616128,-100.200076542985,
178.449324335202));
#16226=CARTESIAN_POINT('Ctrl Pts',(-54.1351780528778,-100.199832004087,
178.01823003711));
#16227=CARTESIAN_POINT('Ctrl Pts',(-53.7214511213677,-100.179252959187,
177.050986426422));
#16228=CARTESIAN_POINT('Ctrl Pts',(-53.6110793820867,-100.158325421843,
176.520980040015));
#16229=CARTESIAN_POINT('Ctrl Pts',(-53.6046567482091,-100.098079340991,
175.450211066692));
#16230=CARTESIAN_POINT('Ctrl Pts',(-53.7080530455439,-100.05436333493,174.920181160456));
#16231=CARTESIAN_POINT('Ctrl Pts',(-54.1082249007172,-99.9470040374134,
173.952740103037));
#16232=CARTESIAN_POINT('Ctrl Pts',(-54.3936147011503,-99.8852054601572,
173.521645801326));
#16233=CARTESIAN_POINT('Ctrl Pts',(-55.1256953569007,-99.7473927319089,
172.778890603587));
#16234=CARTESIAN_POINT('Ctrl Pts',(-55.5704169165303,-99.6672945533789,
172.480030545584));
#16235=CARTESIAN_POINT('Ctrl Pts',(-56.5315444145501,-99.5001344145226,
172.085229134352));
#16236=CARTESIAN_POINT('Ctrl Pts',(-57.035481997341,-99.4150358490739,171.985622467862));
#16237=CARTESIAN_POINT('Ctrl Pts',(-58.0735288862887,-99.2446024971114,
171.985342571377));
#16238=CARTESIAN_POINT('Ctrl Pts',(-58.5971145479235,-99.156102675648,172.092632290086));
#16239=CARTESIAN_POINT('Ctrl Pts',(-59.3883708997698,-99.0181605272865,
172.431409687741));
#16240=CARTESIAN_POINT('Ctrl Pts',(-59.6751894929103,-98.9670768091508,
172.599829292627));
#16241=CARTESIAN_POINT('Ctrl Pts',(-60.1947430170222,-98.8722713063087,
173.000663306832));
#16242=CARTESIAN_POINT('Ctrl Pts',(-60.4265653832759,-98.8293275814563,
173.230023216865));
#16243=CARTESIAN_POINT('Ctrl Pts',(-60.6279056480337,-98.7885057159156,
173.48548506908));
#16244=CARTESIAN_POINT('',(-60.7339116524816,-99.7828712055727,173.485485069079));
#16245=CARTESIAN_POINT('',(-54.5948893516535,-42.1971528497386,173.485485069079));
#16246=CARTESIAN_POINT('',(-60.8585695712285,-100.952196783494,178.485485069079));
#16247=CARTESIAN_POINT('Ctrl Pts',(-60.7339116524819,-99.7828712055727,
173.48548506908));
#16248=CARTESIAN_POINT('Ctrl Pts',(-60.5433422383796,-99.8215092743563,
173.243689343021));
#16249=CARTESIAN_POINT('Ctrl Pts',(-60.3254252550916,-99.8620027807692,
173.025234570342));
#16250=CARTESIAN_POINT('Ctrl Pts',(-59.8388069738715,-99.9510430502776,
172.639494146729));
#16251=CARTESIAN_POINT('Ctrl Pts',(-59.5708294688831,-99.9989441375308,
172.474840262781));
#16252=CARTESIAN_POINT('Ctrl Pts',(-58.8065786374188,-100.132761797002,
172.123020340141));
#16253=CARTESIAN_POINT('Ctrl Pts',(-58.2875416657299,-100.220855942473,
172.001630150343));
#16254=CARTESIAN_POINT('Ctrl Pts',(-57.2525034478298,-100.391469855864,
171.972905197423));
#16255=CARTESIAN_POINT('Ctrl Pts',(-56.7470957002047,-100.47586573524,172.057860325957));
#16256=CARTESIAN_POINT('Ctrl Pts',(-55.7777518615402,-100.643687901527,
172.423693545831));
#16257=CARTESIAN_POINT('Ctrl Pts',(-55.3258879684196,-100.724625332637,
172.708357719645));
#16258=CARTESIAN_POINT('Ctrl Pts',(-54.5742391139785,-100.865067543012,
173.42678745864));
#16259=CARTESIAN_POINT('Ctrl Pts',(-54.2766455660546,-100.927246783973,
173.847812184324));
#16260=CARTESIAN_POINT('Ctrl Pts',(-53.8551198439798,-101.035635163167,
174.784491901194));
#16261=CARTESIAN_POINT('Ctrl Pts',(-53.7362724218245,-101.080074697571,
175.291893961119));
#16262=CARTESIAN_POINT('Ctrl Pts',(-53.6966726188566,-101.14485534785,176.336975547333));
#16263=CARTESIAN_POINT('Ctrl Pts',(-53.781104740909,-101.166894421182,176.864778713819));
#16264=CARTESIAN_POINT('Ctrl Pts',(-54.1457796988072,-101.192405313909,
177.847215661254));
#16265=CARTESIAN_POINT('Ctrl Pts',(-54.4181420491574,-101.195165419479,
178.293920024946));
#16266=CARTESIAN_POINT('Ctrl Pts',(-55.124222242047,-101.18050618865,179.067651982994));
#16267=CARTESIAN_POINT('Ctrl Pts',(-55.5545829942836,-101.16556377856,179.384324188018));
#16268=CARTESIAN_POINT('Ctrl Pts',(-56.5034407659834,-101.128771405425,
179.827717845589));
#16269=CARTESIAN_POINT('Ctrl Pts',(-57.0108467703198,-101.106501632759,
179.954069319539));
#16270=CARTESIAN_POINT('Ctrl Pts',(-58.0555889021011,-101.055796245196,
180.007121753964));
#16271=CARTESIAN_POINT('Ctrl Pts',(-58.583327985711,-101.030365646357,179.929254775814));
#16272=CARTESIAN_POINT('Ctrl Pts',(-59.4322909909086,-100.995268294794,
179.625521780784));
#16273=CARTESIAN_POINT('Ctrl Pts',(-59.7643465168892,-100.982835004683,
179.451476233125));
#16274=CARTESIAN_POINT('Ctrl Pts',(-60.3640168394565,-100.963088982314,
179.021591890977));
#16275=CARTESIAN_POINT('Ctrl Pts',(-60.629977267773,-100.955025096667,178.769762518769));
#16276=CARTESIAN_POINT('Ctrl Pts',(-60.8585695712285,-100.952196783494,
178.485485069079));
#16277=CARTESIAN_POINT('',(-54.5948893516535,-42.1971528497386,178.485485069079));
#16278=CARTESIAN_POINT('Origin',(-51.4899841053611,-42.5281564925371,175.985485069079));
#16279=CARTESIAN_POINT('',(-60.9115725734526,-101.449379528322,178.485485069079));
#16280=CARTESIAN_POINT('',(-60.7869146547057,-100.280053950401,173.485485069079));
#16281=CARTESIAN_POINT('Ctrl Pts',(-60.9115725734526,-101.449379528322,
178.485485069079));
#16282=CARTESIAN_POINT('Ctrl Pts',(-60.7061513850443,-101.451921151309,
178.740946913902));
#16283=CARTESIAN_POINT('Ctrl Pts',(-60.4704858434129,-101.458814761375,
178.970306818076));
#16284=CARTESIAN_POINT('Ctrl Pts',(-59.9426224163936,-101.475670905389,
179.371140823409));
#16285=CARTESIAN_POINT('Ctrl Pts',(-59.6514806148234,-101.48620162758,179.539560425843));
#16286=CARTESIAN_POINT('Ctrl Pts',(-58.8489267840763,-101.518170292608,
179.878337837155));
#16287=CARTESIAN_POINT('Ctrl Pts',(-58.318451154397,-101.542040443154,179.985627564123));
#16288=CARTESIAN_POINT('Ctrl Pts',(-57.2678035683027,-101.594275878231,
179.98534767287));
#16289=CARTESIAN_POINT('Ctrl Pts',(-56.757251497417,-101.617328688418,179.885741010665));
#16290=CARTESIAN_POINT('Ctrl Pts',(-55.782484622021,-101.656547822774,179.490939604252));
#16291=CARTESIAN_POINT('Ctrl Pts',(-55.3308718731657,-101.672004866394,
179.192079540234));
#16292=CARTESIAN_POINT('Ctrl Pts',(-54.5861910682848,-101.69162477747,178.449324335202));
#16293=CARTESIAN_POINT('Ctrl Pts',(-54.2941870595498,-101.691380238572,
178.01823003711));
#16294=CARTESIAN_POINT('Ctrl Pts',(-53.8804601280398,-101.670801193672,
177.050986426422));
#16295=CARTESIAN_POINT('Ctrl Pts',(-53.7700883887589,-101.649873656328,
176.520980040015));
#16296=CARTESIAN_POINT('Ctrl Pts',(-53.7636657548814,-101.589627575476,
175.450211066692));
#16297=CARTESIAN_POINT('Ctrl Pts',(-53.8670620522162,-101.545911569416,
174.920181160456));
#16298=CARTESIAN_POINT('Ctrl Pts',(-54.2672339073893,-101.438552271899,
173.952740103038));
#16299=CARTESIAN_POINT('Ctrl Pts',(-54.5526237078223,-101.376753694642,
173.521645801326));
#16300=CARTESIAN_POINT('Ctrl Pts',(-55.2847043635729,-101.238940966394,
172.778890603587));
#16301=CARTESIAN_POINT('Ctrl Pts',(-55.7294259232024,-101.158842787864,
172.480030545584));
#16302=CARTESIAN_POINT('Ctrl Pts',(-56.6905534212225,-100.991682649007,
172.085229134352));
#16303=CARTESIAN_POINT('Ctrl Pts',(-57.1944910040133,-100.906584083559,
171.985622467862));
#16304=CARTESIAN_POINT('Ctrl Pts',(-58.2325378929607,-100.736150731597,
171.985342571377));
#16305=CARTESIAN_POINT('Ctrl Pts',(-58.7561235545955,-100.647650910134,
172.092632290086));
#16306=CARTESIAN_POINT('Ctrl Pts',(-59.547378382634,-100.509709027422,172.431409035321));
#16307=CARTESIAN_POINT('Ctrl Pts',(-59.8341956324852,-100.458625554302,
172.599827608127));
#16308=CARTESIAN_POINT('Ctrl Pts',(-60.353747032482,-100.363820463799,173.000658940243));
#16309=CARTESIAN_POINT('Ctrl Pts',(-60.5855754147608,-100.320875608161,
173.230024517154));
#16310=CARTESIAN_POINT('Ctrl Pts',(-60.7869146547057,-100.280053950401,
173.485485069079));
#16311=CARTESIAN_POINT('',(-60.8929206591539,-101.274419440058,173.485485069079));
#16312=CARTESIAN_POINT('',(-54.5948893516535,-42.1971528497386,173.485485069079));
#16313=CARTESIAN_POINT('',(-53.8728824136219,-102.614109889754,175.985485078249));
#16314=CARTESIAN_POINT('Ctrl Pts',(-60.8929206591538,-101.274419440058,
173.485485069079));
#16315=CARTESIAN_POINT('Ctrl Pts',(-60.7102269210105,-101.311460710579,
173.253682052479));
#16316=CARTESIAN_POINT('Ctrl Pts',(-60.502365296309,-101.350178825903,173.043294821439));
#16317=CARTESIAN_POINT('Ctrl Pts',(-60.0395467045387,-101.435037463867,
172.669117273279));
#16318=CARTESIAN_POINT('Ctrl Pts',(-59.7851929521217,-101.480626055513,
172.507657607619));
#16319=CARTESIAN_POINT('Ctrl Pts',(-59.0406892261035,-101.611411060069,
172.147006028652));
#16320=CARTESIAN_POINT('Ctrl Pts',(-58.5252323432285,-101.699158257146,
172.015459906787));
#16321=CARTESIAN_POINT('Ctrl Pts',(-57.4926845327902,-101.869865342548,
171.965563441252));
#16322=CARTESIAN_POINT('Ctrl Pts',(-56.9862231691556,-101.953834724284,
172.039921277568));
#16323=CARTESIAN_POINT('Ctrl Pts',(-56.0247569440159,-102.11975084989,172.379917992812));
#16324=CARTESIAN_POINT('Ctrl Pts',(-55.5793041661649,-102.199151236466,
172.644151600608));
#16325=CARTESIAN_POINT('Ctrl Pts',(-54.8070206720663,-102.342342925632,
173.335663171704));
#16326=CARTESIAN_POINT('Ctrl Pts',(-54.4900108722134,-102.406626608065,
173.758726921452));
#16327=CARTESIAN_POINT('Ctrl Pts',(-54.1325977439973,-102.495899358773,
174.506835663783));
#16328=CARTESIAN_POINT('Ctrl Pts',(-54.033087296471,-102.525372948297,174.796081818852));
#16329=CARTESIAN_POINT('Ctrl Pts',(-53.9027346997917,-102.576055283617,
175.386624643971));
#16330=CARTESIAN_POINT('Ctrl Pts',(-53.8710837883173,-102.597238295983,
175.685621934182));
#16331=CARTESIAN_POINT('Ctrl Pts',(-53.8728824136219,-102.614109889754,
175.985485078249));
#16332=CARTESIAN_POINT('',(-60.9552496185426,-101.859082229163,178.485485069079));
#16333=CARTESIAN_POINT('Origin',(-57.8503443722502,-102.190085871961,175.985485069079));
#16334=CARTESIAN_POINT('',(-54.5948893516535,-42.1971528497386,178.485485069079));
#16335=CARTESIAN_POINT('Origin',(-57.8503443722502,-102.190085871961,175.985485069079));
#16336=CARTESIAN_POINT('',(-59.5310685485181,-102.312170685956,173.485485069079));
#16337=CARTESIAN_POINT('',(-56.2564866337797,-102.944965370977,173.489866571436));
#16338=CARTESIAN_POINT('Ctrl Pts',(-56.2564866337792,-102.944965370977,
173.489866571436));
#16339=CARTESIAN_POINT('Ctrl Pts',(-56.4989794446454,-102.895253602946,
173.325488559424));
#16340=CARTESIAN_POINT('Ctrl Pts',(-56.7642531084334,-102.842545984514,
173.198515194001));
#16341=CARTESIAN_POINT('Ctrl Pts',(-57.3189939774646,-102.735361409915,
173.028869909839));
#16342=CARTESIAN_POINT('Ctrl Pts',(-57.6051560932325,-102.681480718025,
172.985872610607));
#16343=CARTESIAN_POINT('Ctrl Pts',(-58.1808148055288,-102.575807458543,
172.985103094898));
#16344=CARTESIAN_POINT('Ctrl Pts',(-58.4670480699436,-102.521964579041,
173.02725873048));
#16345=CARTESIAN_POINT('Ctrl Pts',(-59.0224385185242,-102.414706992302,
173.195445680148));
#16346=CARTESIAN_POINT('Ctrl Pts',(-59.2880999534127,-102.361950173258,
173.32172571804));
#16347=CARTESIAN_POINT('Ctrl Pts',(-59.5310685485181,-102.312170685956,
173.485485069079));
#16348=CARTESIAN_POINT('',(-59.5702274233335,-102.679491706429,173.485485069079));
#16349=CARTESIAN_POINT('',(-59.4993129890855,-102.014294800821,173.485485069079));
#16350=CARTESIAN_POINT('',(-56.2951298069876,-103.312392114382,173.490216228516));
#16351=CARTESIAN_POINT('Ctrl Pts',(-59.570227423334,-102.679491706429,173.48548506908));
#16352=CARTESIAN_POINT('Ctrl Pts',(-59.3272139607109,-102.729280386204,
173.321695477607));
#16353=CARTESIAN_POINT('Ctrl Pts',(-59.0614995139417,-102.782047448757,
173.195399203235));
#16354=CARTESIAN_POINT('Ctrl Pts',(-58.5060004700764,-102.889324948104,
173.027212807591));
#16355=CARTESIAN_POINT('Ctrl Pts',(-58.2197132838581,-102.943175309962,
172.985072830814));
#16356=CARTESIAN_POINT('Ctrl Pts',(-57.6439497370216,-103.048869755498,
172.98590377254));
#16357=CARTESIAN_POINT('Ctrl Pts',(-57.3577384239598,-103.102760957316,
173.028947814549));
#16358=CARTESIAN_POINT('Ctrl Pts',(-56.8029251208583,-103.209962647076,
173.198713721519));
#16359=CARTESIAN_POINT('Ctrl Pts',(-56.5376294470979,-103.262676571874,
173.325758640231));
#16360=CARTESIAN_POINT('Ctrl Pts',(-56.2951298069871,-103.312392114382,
173.490216228516));
#16361=CARTESIAN_POINT('',(-56.2564866337797,-102.944965370977,173.489866571436));
#16362=CARTESIAN_POINT('Origin',(-57.8503443722502,-102.190085871961,175.985485069079));
#16363=CARTESIAN_POINT('',(-59.6900775551904,-103.803718920442,173.485485069079));
#16364=CARTESIAN_POINT('',(-56.4134173387405,-104.436939704691,173.491276679515));
#16365=CARTESIAN_POINT('Ctrl Pts',(-56.41341733874,-104.436939704691,173.491276679516));
#16366=CARTESIAN_POINT('Ctrl Pts',(-56.6559375281166,-104.387212747836,
173.326577849171));
#16367=CARTESIAN_POINT('Ctrl Pts',(-56.9212997932767,-104.334479728502,
173.199315985643));
#16368=CARTESIAN_POINT('Ctrl Pts',(-57.4763324841321,-104.227226186699,
173.029184302443));
#16369=CARTESIAN_POINT('Ctrl Pts',(-57.7626928792531,-104.173303132952,
172.985998496287));
#16370=CARTESIAN_POINT('Ctrl Pts',(-58.3387741518067,-104.067544473328,
172.984981238005));
#16371=CARTESIAN_POINT('Ctrl Pts',(-58.6252247782338,-104.013671424672,
173.02707370444));
#16372=CARTESIAN_POINT('Ctrl Pts',(-59.1810529817342,-103.906333570922,
173.195258356014));
#16373=CARTESIAN_POINT('Ctrl Pts',(-59.4469281068036,-103.853535461025,
173.321603824031));
#16374=CARTESIAN_POINT('Ctrl Pts',(-59.6900775551904,-103.803718920442,
173.485485069079));
#16375=CARTESIAN_POINT('',(-59.7292364300057,-104.171039940915,173.485485069079));
#16376=CARTESIAN_POINT('',(-59.4993129890855,-102.014294800821,173.485485069079));
#16377=CARTESIAN_POINT('',(-56.4520785736129,-104.80436276488,173.491614708043));
#16378=CARTESIAN_POINT('Ctrl Pts',(-59.7292364300062,-104.171039940915,
173.48548506908));
#16379=CARTESIAN_POINT('Ctrl Pts',(-59.4860436647418,-104.220865356275,
173.32157462872));
#16380=CARTESIAN_POINT('Ctrl Pts',(-59.2201173545953,-104.273673356308,
173.195213495731));
#16381=CARTESIAN_POINT('Ctrl Pts',(-58.6641842924699,-104.381030436189,
173.027029420215));
#16382=CARTESIAN_POINT('Ctrl Pts',(-58.3776815999021,-104.434910714353,
172.984952103883));
#16383=CARTESIAN_POINT('Ctrl Pts',(-57.8014991187094,-104.540689830233,
172.986028757149));
#16384=CARTESIAN_POINT('Ctrl Pts',(-57.5150912399971,-104.594623030155,
173.029259751801));
#16385=CARTESIAN_POINT('Ctrl Pts',(-56.9599887060397,-104.70189308346,173.199508012997));
#16386=CARTESIAN_POINT('Ctrl Pts',(-56.6946052633784,-104.754632179713,
173.326839009941));
#16387=CARTESIAN_POINT('Ctrl Pts',(-56.452078573613,-104.80436276488,173.491614708043));
#16388=CARTESIAN_POINT('',(-56.4134173387405,-104.436939704691,173.491276679515));
#16389=CARTESIAN_POINT('Origin',(-57.8503443722502,-102.190085871961,175.985485069079));
#16390=CARTESIAN_POINT('',(-59.8490865618626,-105.295267154927,173.485485069079));
#16391=CARTESIAN_POINT('',(-56.5704762085008,-105.92888783639,173.492602186485));
#16392=CARTESIAN_POINT('Ctrl Pts',(-56.5704762085003,-105.92888783639,173.492602186486));
#16393=CARTESIAN_POINT('Ctrl Pts',(-56.8130217456382,-105.879146680719,
173.327602022451));
#16394=CARTESIAN_POINT('Ctrl Pts',(-57.07846691305,-105.826389859661,173.200069123079));
#16395=CARTESIAN_POINT('Ctrl Pts',(-57.633773223064,-105.719071619894,173.029480349745));
#16396=CARTESIAN_POINT('Ctrl Pts',(-57.9203197057099,-105.6651088001,172.986117345367));
#16397=CARTESIAN_POINT('Ctrl Pts',(-58.4967976547893,-105.559269960174,
172.984867162949));
#16398=CARTESIAN_POINT('Ctrl Pts',(-58.7834523644571,-105.505368567675,
173.026900204104));
#16399=CARTESIAN_POINT('Ctrl Pts',(-59.339691582227,-105.397955355066,173.195082541135));
#16400=CARTESIAN_POINT('Ctrl Pts',(-59.6057673336779,-105.345118480053,
173.321489393483));
#16401=CARTESIAN_POINT('Ctrl Pts',(-59.8490865618626,-105.295267154927,
173.485485069079));
#16402=CARTESIAN_POINT('',(-59.8882454366779,-105.662588175401,173.485485069079));
#16403=CARTESIAN_POINT('',(-59.4993129890855,-102.014294800821,173.485485069079));
#16404=CARTESIAN_POINT('',(-56.6091901843099,-106.296300098484,173.492904904243));
#16405=CARTESIAN_POINT('Ctrl Pts',(-59.8882454366779,-105.662588175401,
173.485485069079));
#16406=CARTESIAN_POINT('Ctrl Pts',(-59.6448874651583,-105.712447438273,
173.321463280712));
#16407=CARTESIAN_POINT('Ctrl Pts',(-59.3787659285087,-105.765293159726,
173.195042425979));
#16408=CARTESIAN_POINT('Ctrl Pts',(-58.8224329097879,-105.872723569926,
173.026860638454));
#16409=CARTESIAN_POINT('Ctrl Pts',(-58.5357316247444,-105.926631433394,
172.984841174824));
#16410=CARTESIAN_POINT('Ctrl Pts',(-57.959163155205,-106.03248857175,172.986144557556));
#16411=CARTESIAN_POINT('Ctrl Pts',(-57.6725742135264,-106.086460466031,
173.029548030212));
#16412=CARTESIAN_POINT('Ctrl Pts',(-57.1172055074798,-106.19379346387,173.200241176083));
#16413=CARTESIAN_POINT('Ctrl Pts',(-56.8517414582687,-106.246555710665,
173.327835953701));
#16414=CARTESIAN_POINT('Ctrl Pts',(-56.60919018431,-106.296300098484,173.492904904243));
#16415=CARTESIAN_POINT('',(-56.5704762085008,-105.92888783639,173.492602186485));
#16416=CARTESIAN_POINT('Origin',(-57.8503443722502,-102.190085871961,175.985485069079));
#16417=CARTESIAN_POINT('',(-60.0080955685348,-106.786815389413,173.485485069079));
#16418=CARTESIAN_POINT('',(-56.7277951555015,-107.420782694947,173.49375276819));
#16419=CARTESIAN_POINT('Ctrl Pts',(-56.727795155501,-107.420782694947,173.49375276819));
#16420=CARTESIAN_POINT('Ctrl Pts',(-56.9703623912548,-107.371029275934,
173.328491222585));
#16421=CARTESIAN_POINT('Ctrl Pts',(-57.2358792201269,-107.318251853156,
173.200723175827));
#16422=CARTESIAN_POINT('Ctrl Pts',(-57.7914224962462,-107.210877556492,
173.02973773311));
#16423=CARTESIAN_POINT('Ctrl Pts',(-58.0781302770999,-107.156880260998,
172.986220914227));
#16424=CARTESIAN_POINT('Ctrl Pts',(-58.6549521376339,-107.050971897315,
172.984768510842));
#16425=CARTESIAN_POINT('Ctrl Pts',(-58.9417838117716,-106.997045913428,
173.026749932901));
#16426=CARTESIAN_POINT('Ctrl Pts',(-59.4983794295013,-106.889567359307,
173.194930140002));
#16427=CARTESIAN_POINT('Ctrl Pts',(-59.7646291406404,-106.836696872864,
173.321390181777));
#16428=CARTESIAN_POINT('Ctrl Pts',(-60.0080955685353,-106.786815389413,
173.48548506908));
#16429=CARTESIAN_POINT('',(-60.0472544433502,-107.154136409886,173.485485069079));
#16430=CARTESIAN_POINT('',(-59.4993129890855,-102.014294800821,173.485485069079));
#16431=CARTESIAN_POINT('',(-56.766590524313,-107.788178276076,173.494000465338));
#16432=CARTESIAN_POINT('Ctrl Pts',(-60.0472544433507,-107.154136409886,
173.48548506908));
#16433=CARTESIAN_POINT('Ctrl Pts',(-59.803756348025,-107.204024381371,173.321368838121));
#16434=CARTESIAN_POINT('Ctrl Pts',(-59.5374692105895,-107.256902098957,
173.194897357342));
#16435=CARTESIAN_POINT('Ctrl Pts',(-58.9807969137183,-107.364394710774,
173.026717623417));
#16436=CARTESIAN_POINT('Ctrl Pts',(-58.6939271659299,-107.41832598715,172.984747318098));
#16437=CARTESIAN_POINT('Ctrl Pts',(-58.1170313186328,-107.524249308753,
172.98624325915));
#16438=CARTESIAN_POINT('Ctrl Pts',(-57.83028884093,-107.578254021139,173.029793191131));
#16439=CARTESIAN_POINT('Ctrl Pts',(-57.2746946153895,-107.685640373486,
173.200864016778));
#16440=CARTESIAN_POINT('Ctrl Pts',(-57.0091623950157,-107.73842222438,173.328682671664));
#16441=CARTESIAN_POINT('Ctrl Pts',(-56.766590524313,-107.788178276076,173.494000465338));
#16442=CARTESIAN_POINT('',(-56.7277951555015,-107.420782694947,173.49375276819));
#16443=CARTESIAN_POINT('Origin',(-57.8503443722502,-102.190085871961,175.985485069079));
#16444=CARTESIAN_POINT('',(-60.167104575207,-108.278363623899,173.485485069079));
#16445=CARTESIAN_POINT('',(-56.8854801878217,-108.912602509009,173.494655322398));
#16446=CARTESIAN_POINT('Ctrl Pts',(-56.8854801878217,-108.912602509009,
173.494655322398));
#16447=CARTESIAN_POINT('Ctrl Pts',(-57.1280642474478,-108.86283951024,173.329188860889));
#16448=CARTESIAN_POINT('Ctrl Pts',(-57.3936370951202,-108.810045965017,
173.20123643479));
#16449=CARTESIAN_POINT('Ctrl Pts',(-57.9493659024473,-108.702627762264,
173.029939895836));
#16450=CARTESIAN_POINT('Ctrl Pts',(-58.2362000607429,-108.648603450439,
172.986302419157));
#16451=CARTESIAN_POINT('Ctrl Pts',(-58.8132914268818,-108.542640598827,
172.984691363898));
#16452=CARTESIAN_POINT('Ctrl Pts',(-59.1002617970616,-108.488695332397,
173.026632270813));
#16453=CARTESIAN_POINT('Ctrl Pts',(-59.657136744632,-108.381165569144,173.194810728768));
#16454=CARTESIAN_POINT('Ctrl Pts',(-59.9235227921166,-108.328268741361,
173.321312433078));
#16455=CARTESIAN_POINT('Ctrl Pts',(-60.1671045752075,-108.278363623899,
173.48548506908));
#16456=CARTESIAN_POINT('',(-60.2062634500224,-108.645684644372,173.485485069079));
#16457=CARTESIAN_POINT('',(-59.4993129890855,-102.014294800821,173.485485069079));
#16458=CARTESIAN_POINT('',(-56.9243786881305,-109.279976942609,173.494832944144));
#16459=CARTESIAN_POINT('Ctrl Pts',(-60.2062634500224,-108.645684644372,
173.485485069079));
#16460=CARTESIAN_POINT('Ctrl Pts',(-59.9626589773804,-108.695594410477,
173.321297140459));
#16461=CARTESIAN_POINT('Ctrl Pts',(-59.6962461124362,-108.748496419544,
173.194787243505));
#16462=CARTESIAN_POINT('Ctrl Pts',(-59.1393162193742,-108.856036255613,
173.026609137869));
#16463=CARTESIAN_POINT('Ctrl Pts',(-58.8523185670886,-108.909985315935,
172.984676206522));
#16464=CARTESIAN_POINT('Ctrl Pts',(-58.2751741904042,-109.01595888565,172.986318485945));
#16465=CARTESIAN_POINT('Ctrl Pts',(-57.988315176016,-109.069988511531,173.029979707834));
#16466=CARTESIAN_POINT('Ctrl Pts',(-57.4325498914681,-109.1774153483,173.201337463568));
#16467=CARTESIAN_POINT('Ctrl Pts',(-57.1669660388386,-109.230212062577,
173.32932616747));
#16468=CARTESIAN_POINT('Ctrl Pts',(-56.92437868813,-109.279976942609,173.494832944145));
#16469=CARTESIAN_POINT('',(-56.8854801878217,-108.912602509009,173.494655322398));
#16470=CARTESIAN_POINT('Origin',(-57.8503443722502,-102.190085871961,175.985485069079));
#16471=CARTESIAN_POINT('',(-60.3261135818793,-109.769911858384,173.485485069079));
#16472=CARTESIAN_POINT('',(-57.043608201862,-110.404331475209,173.49525648095));
#16473=CARTESIAN_POINT('Ctrl Pts',(-57.043608201862,-110.404331475209,173.49525648095));
#16474=CARTESIAN_POINT('Ctrl Pts',(-57.2862033712323,-110.354562115194,
173.329653591047));
#16475=CARTESIAN_POINT('Ctrl Pts',(-57.5518134361477,-110.301757850008,
173.201578394561));
#16476=CARTESIAN_POINT('Ctrl Pts',(-58.1076656473085,-110.194310435517,
173.030074676988));
#16477=CARTESIAN_POINT('Ctrl Pts',(-58.3945839079253,-110.140268142502,
172.986356834207));
#16478=CARTESIAN_POINT('Ctrl Pts',(-58.9718546506282,-110.034269022205,
172.984640095432));
#16479=CARTESIAN_POINT('Ctrl Pts',(-59.258917342467,-109.980310916145,173.026554005271));
#16480=CARTESIAN_POINT('Ctrl Pts',(-59.8159782237473,-109.872747067167,
173.194731260047));
#16481=CARTESIAN_POINT('Ctrl Pts',(-60.0824550199058,-109.81983270633,173.321260684579));
#16482=CARTESIAN_POINT('Ctrl Pts',(-60.3261135818792,-109.769911858384,
173.485485069079));
#16483=CARTESIAN_POINT('',(-60.3652724566946,-110.137232878857,173.485485069079));
#16484=CARTESIAN_POINT('',(-59.4993129890855,-102.014294800821,173.485485069079));
#16485=CARTESIAN_POINT('',(-57.0826240442751,-110.771681839542,173.495354125416));
#16486=CARTESIAN_POINT('Ctrl Pts',(-60.3652724566951,-110.137232878857,
173.48548506908));
#16487=CARTESIAN_POINT('Ctrl Pts',(-60.1216014284393,-110.187156280899,
173.321252282381));
#16488=CARTESIAN_POINT('Ctrl Pts',(-59.8551098973998,-110.240073488555,
173.194718357766));
#16489=CARTESIAN_POINT('Ctrl Pts',(-59.2980188256342,-110.347642872018,
173.026541301285));
#16490=CARTESIAN_POINT('Ctrl Pts',(-59.0109411433348,-110.401603063207,
172.984631777171));
#16491=CARTESIAN_POINT('Ctrl Pts',(-58.4336412749047,-110.507608072709,
172.986365681921));
#16492=CARTESIAN_POINT('Ctrl Pts',(-58.1467093586421,-110.561653285463,
173.030096578176));
#16493=CARTESIAN_POINT('Ctrl Pts',(-57.5908371149738,-110.669105442524,
173.201633944823));
#16494=CARTESIAN_POINT('Ctrl Pts',(-57.3252210114735,-110.721911447645,
173.32972907989));
#16495=CARTESIAN_POINT('Ctrl Pts',(-57.0826240442746,-110.771681839542,
173.495354125417));
#16496=CARTESIAN_POINT('',(-57.043608201862,-110.404331475209,173.49525648095));
#16497=CARTESIAN_POINT('Origin',(-57.8503443722502,-102.190085871961,175.985485069079));
#16498=CARTESIAN_POINT('',(-60.4851225885515,-111.26146009287,173.485485069079));
#16499=CARTESIAN_POINT('',(-57.2022249863543,-111.895960177099,173.495524270213));
#16500=CARTESIAN_POINT('Ctrl Pts',(-57.2022168441609,-111.895961847564,
173.49552983027));
#16501=CARTESIAN_POINT('Ctrl Pts',(-57.4448169377341,-111.846189658907,
173.329866182698));
#16502=CARTESIAN_POINT('Ctrl Pts',(-57.7104516990721,-111.793378952777,
173.201730747205));
#16503=CARTESIAN_POINT('Ctrl Pts',(-58.2663588369567,-111.685918534124,
173.030134748854));
#16504=CARTESIAN_POINT('Ctrl Pts',(-58.5533145426031,-111.631868234738,
172.986381106475));
#16505=CARTESIAN_POINT('Ctrl Pts',(-59.1306651557994,-111.525852964465,
172.984617287507));
#16506=CARTESIAN_POINT('Ctrl Pts',(-59.417768957726,-111.471889139892,173.026519168419));
#16507=CARTESIAN_POINT('Ctrl Pts',(-59.9749126339239,-111.364310113107,
173.194695877431));
#16508=CARTESIAN_POINT('Ctrl Pts',(-60.2414298391488,-111.311387945147,
173.321237642461));
#16509=CARTESIAN_POINT('Ctrl Pts',(-60.4851225885515,-111.26146009287,173.485485069079));
#16510=CARTESIAN_POINT('',(-60.5242814633668,-111.628781113343,173.485485069079));
#16511=CARTESIAN_POINT('',(-59.4993129890855,-102.014294800821,173.485485069079));
#16512=CARTESIAN_POINT('',(-57.2413645753253,-112.263285154287,173.495537439996));
#16513=CARTESIAN_POINT('Ctrl Pts',(-60.5242814633673,-111.628781113343,
173.48548506908));
#16514=CARTESIAN_POINT('Ctrl Pts',(-60.2805870334125,-111.678709309933,
173.321236509779));
#16515=CARTESIAN_POINT('Ctrl Pts',(-60.014067841777,-111.73163186167,173.194694138168));
#16516=CARTESIAN_POINT('Ctrl Pts',(-59.4569200955657,-111.839211634557,
173.026517456143));
#16517=CARTESIAN_POINT('Ctrl Pts',(-59.1698142727596,-111.893175740257,
172.984616166662));
#16518=CARTESIAN_POINT('Ctrl Pts',(-58.5924597320949,-111.999191804659,
172.986382300312));
#16519=CARTESIAN_POINT('Ctrl Pts',(-58.3055021845535,-112.053242497856,
173.030137703114));
#16520=CARTESIAN_POINT('Ctrl Pts',(-57.7495923447614,-112.160703556161,
173.201738239673));
#16521=CARTESIAN_POINT('Ctrl Pts',(-57.4839649112239,-112.213512826487,
173.329870804249));
#16522=CARTESIAN_POINT('Ctrl Pts',(-57.2413645753249,-112.263285154288,
173.495537439996));
#16523=CARTESIAN_POINT('',(-57.2022249863543,-111.895960177099,173.495524270213));
#16524=CARTESIAN_POINT('Ctrl Pts',(-55.8010581637105,-111.27473179072,176.985485069079));
#16525=CARTESIAN_POINT('Ctrl Pts',(-55.8010581637105,-111.27473179072,174.585485069079));
#16526=CARTESIAN_POINT('Ctrl Pts',(-55.7783810390096,-111.064602968901,
176.985485069079));
#16527=CARTESIAN_POINT('Ctrl Pts',(-55.7783810390096,-111.064602968901,
174.585485069079));
#16528=CARTESIAN_POINT('Ctrl Pts',(-55.7556780473044,-110.854924957015,
176.985485069079));
#16529=CARTESIAN_POINT('Ctrl Pts',(-55.7556780473044,-110.854924957015,
174.585485069079));
#16530=CARTESIAN_POINT('Ctrl Pts',(-55.7329493398378,-110.645696396341,
176.985485069079));
#16531=CARTESIAN_POINT('Ctrl Pts',(-55.7329493398378,-110.645696396341,
174.585485069079));
#16532=CARTESIAN_POINT('',(-55.8006548129149,-111.270994369097,176.985485069079));
#16533=CARTESIAN_POINT('',(-55.7842612734031,-111.119216054728,174.985485069079));
#16534=CARTESIAN_POINT('Ctrl Pts',(-55.8006548129149,-111.270994369097,
176.985485069079));
#16535=CARTESIAN_POINT('Ctrl Pts',(-55.7959899850579,-111.227771226778,
176.734066274092));
#16536=CARTESIAN_POINT('Ctrl Pts',(-55.7920778567201,-111.19155181727,176.481361799263));
#16537=CARTESIAN_POINT('Ctrl Pts',(-55.7892777370619,-111.165635089573,
176.226833564659));
#16538=CARTESIAN_POINT('Ctrl Pts',(-55.7887660302618,-111.160898947044,
176.180319899403));
#16539=CARTESIAN_POINT('Ctrl Pts',(-55.788291815303,-111.156510162777,176.133790055636));
#16540=CARTESIAN_POINT('Ctrl Pts',(-55.7878564822688,-111.152481456388,
176.087208558517));
#16541=CARTESIAN_POINT('Ctrl Pts',(-55.787624519141,-111.150334797942,176.062388044287));
#16542=CARTESIAN_POINT('Ctrl Pts',(-55.7874036801174,-111.148291157356,
176.037561954759));
#16543=CARTESIAN_POINT('Ctrl Pts',(-55.7871941426494,-111.146352156858,
176.012724127882));
#16544=CARTESIAN_POINT('Ctrl Pts',(-55.7871517350105,-111.145959728556,
176.00769727706));
#16545=CARTESIAN_POINT('Ctrl Pts',(-55.7871097917316,-111.145571599719,
176.002670116688));
#16546=CARTESIAN_POINT('Ctrl Pts',(-55.7870683141655,-111.145187782708,
175.997642593218));
#16547=CARTESIAN_POINT('Ctrl Pts',(-55.787045553112,-111.144977160911,175.994883710735));
#16548=CARTESIAN_POINT('Ctrl Pts',(-55.7870229324165,-111.144767838626,
175.99212473304));
#16549=CARTESIAN_POINT('Ctrl Pts',(-55.7870004522962,-111.144559817836,
175.989365651051));
#16550=CARTESIAN_POINT('Ctrl Pts',(-55.7869897994373,-111.144461241134,
175.988058179796));
#16551=CARTESIAN_POINT('Ctrl Pts',(-55.7869792403406,-111.144363532218,
175.986758281555));
#16552=CARTESIAN_POINT('Ctrl Pts',(-55.7869689268157,-111.144268095849,
175.985484943511));
#16553=CARTESIAN_POINT('Ctrl Pts',(-55.7869624231925,-111.144207914466,
175.98468198711));
#16554=CARTESIAN_POINT('Ctrl Pts',(-55.7869560149882,-111.144148616101,
175.983889593831));
#16555=CARTESIAN_POINT('Ctrl Pts',(-55.7869497397808,-111.144090548475,
175.983112525094));
#16556=CARTESIAN_POINT('Ctrl Pts',(-55.7869283414167,-111.143892538734,
175.980462732245));
#16557=CARTESIAN_POINT('Ctrl Pts',(-55.7869070495478,-111.143695515059,
175.977812867795));
#16558=CARTESIAN_POINT('Ctrl Pts',(-55.7868858643761,-111.143499479302,
175.975162926479));
#16559=CARTESIAN_POINT('Ctrl Pts',(-55.7868496261866,-111.143164151318,
175.970630082616));
#16560=CARTESIAN_POINT('Ctrl Pts',(-55.7868137003751,-111.142831715664,
175.966097037108));
#16561=CARTESIAN_POINT('Ctrl Pts',(-55.7867780879403,-111.142502181493,
175.961563763315));
#16562=CARTESIAN_POINT('Ctrl Pts',(-55.7866367441066,-111.141194278134,
175.94357144406));
#16563=CARTESIAN_POINT('Ctrl Pts',(-55.786500346155,-111.13993216747,175.925576725693));
#16564=CARTESIAN_POINT('Ctrl Pts',(-55.7863689538889,-111.138716397416,
175.90757786131));
#16565=CARTESIAN_POINT('Ctrl Pts',(-55.7859262399947,-111.134619974459,
175.84693237906));
#16566=CARTESIAN_POINT('Ctrl Pts',(-55.785540741415,-111.131053222404,175.786292696376));
#16567=CARTESIAN_POINT('Ctrl Pts',(-55.7852143761284,-111.128033707311,
175.725582395189));
#16568=CARTESIAN_POINT('Ctrl Pts',(-55.7838829914684,-111.115715803902,
175.477918911893));
#16569=CARTESIAN_POINT('Ctrl Pts',(-55.7835587254065,-111.112716714097,
175.233343306962));
#16570=CARTESIAN_POINT('Ctrl Pts',(-55.7842612734033,-111.119216054728,
174.985485069079));
#16571=CARTESIAN_POINT('',(-55.7498389523163,-110.801299724063,176.985485069079));
#16572=CARTESIAN_POINT('Ctrl Pts',(-55.7498389523163,-110.801299724063,
176.985485069079));
#16573=CARTESIAN_POINT('Ctrl Pts',(-55.7668185587566,-110.957859362734,
176.98548506908));
#16574=CARTESIAN_POINT('Ctrl Pts',(-55.7837570912844,-111.114424255627,
176.985485069079));
#16575=CARTESIAN_POINT('Ctrl Pts',(-55.8006548129149,-111.270994369097,
176.985485069079));
#16576=CARTESIAN_POINT('',(-55.7333536026738,-110.64941790035,174.985485069079));
#16577=CARTESIAN_POINT('Ctrl Pts',(-55.7333536026738,-110.64941790035,174.985485069079));
#16578=CARTESIAN_POINT('Ctrl Pts',(-55.7372834331241,-110.685595265291,
175.195807752872));
#16579=CARTESIAN_POINT('Ctrl Pts',(-55.7406814496559,-110.716897508472,
175.407178770022));
#16580=CARTESIAN_POINT('Ctrl Pts',(-55.7433327290313,-110.741328193525,
175.619578568996));
#16581=CARTESIAN_POINT('Ctrl Pts',(-55.7442914854839,-110.750162825271,
175.696386648785));
#16582=CARTESIAN_POINT('Ctrl Pts',(-55.7451515103665,-110.758088892097,
175.773224689473));
#16583=CARTESIAN_POINT('Ctrl Pts',(-55.7459059204445,-110.765042260031,
175.850232063412));
#16584=CARTESIAN_POINT('Ctrl Pts',(-55.7462523324549,-110.768235125867,
175.885592512583));
#16585=CARTESIAN_POINT('Ctrl Pts',(-55.7465762177677,-110.771220523207,
175.920962194947));
#16586=CARTESIAN_POINT('Ctrl Pts',(-55.7468770555128,-110.773993592097,
175.956358578691));
#16587=CARTESIAN_POINT('Ctrl Pts',(-55.7469241848152,-110.774428021633,
175.961903783369));
#16588=CARTESIAN_POINT('Ctrl Pts',(-55.746970746089,-110.77485721814,175.967449362544));
#16589=CARTESIAN_POINT('Ctrl Pts',(-55.7470167375474,-110.775281164934,
175.972995388113));
#16590=CARTESIAN_POINT('Ctrl Pts',(-55.7470405191156,-110.775500382153,
175.975863163782));
#16591=CARTESIAN_POINT('Ctrl Pts',(-55.7470641481921,-110.775718194464,
175.978731042493));
#16592=CARTESIAN_POINT('Ctrl Pts',(-55.7470876245358,-110.775934599617,
175.981599034278));
#16593=CARTESIAN_POINT('Ctrl Pts',(-55.7470982974718,-110.776032982839,
175.982902895442));
#16594=CARTESIAN_POINT('Ctrl Pts',(-55.7471089431013,-110.776131114505,
175.984207354532));
#16595=CARTESIAN_POINT('Ctrl Pts',(-55.7471193391274,-110.776226945462,
175.985484943485));
#16596=CARTESIAN_POINT('Ctrl Pts',(-55.7471278543292,-110.77630543891,175.986531394086));
#16597=CARTESIAN_POINT('Ctrl Pts',(-55.747136205884,-110.776382423951,175.987559814951));
#16598=CARTESIAN_POINT('Ctrl Pts',(-55.7471442735878,-110.776456792525,
175.988555110492));
#16599=CARTESIAN_POINT('Ctrl Pts',(-55.7471656873326,-110.776654185699,
175.991196878856));
#16600=CARTESIAN_POINT('Ctrl Pts',(-55.7471869945963,-110.776850597934,
175.993838718488));
#16601=CARTESIAN_POINT('Ctrl Pts',(-55.7472081951813,-110.777046027391,
175.996480634583));
#16602=CARTESIAN_POINT('Ctrl Pts',(-55.7472443395524,-110.777379210404,
176.000984774238));
#16603=CARTESIAN_POINT('Ctrl Pts',(-55.7472801736672,-110.777709535178,
176.005489113248));
#16604=CARTESIAN_POINT('Ctrl Pts',(-55.7473156965597,-110.77803699272,176.009993677794));
#16605=CARTESIAN_POINT('Ctrl Pts',(-55.7474552321236,-110.779323261079,
176.027687815538));
#16606=CARTESIAN_POINT('Ctrl Pts',(-55.7475899566659,-110.780565206319,
176.045384291183));
#16607=CARTESIAN_POINT('Ctrl Pts',(-55.7477198140849,-110.781762306068,
176.063084767689));
#16608=CARTESIAN_POINT('Ctrl Pts',(-55.7481667684031,-110.785882585879,
176.124007774403));
#16609=CARTESIAN_POINT('Ctrl Pts',(-55.7485556725842,-110.789467988468,
176.184924768193));
#16610=CARTESIAN_POINT('Ctrl Pts',(-55.7488846099061,-110.792500660407,
176.245913294751));
#16611=CARTESIAN_POINT('Ctrl Pts',(-55.7502194176992,-110.804807060041,
176.493401053396));
#16612=CARTESIAN_POINT('Ctrl Pts',(-55.7505439219598,-110.807799862509,
176.737802780905));
#16613=CARTESIAN_POINT('Ctrl Pts',(-55.7498389523165,-110.801299724063,
176.985485069079));
#16614=CARTESIAN_POINT('Ctrl Pts',(-55.7842612734031,-111.119216054728,
174.985485069079));
#16615=CARTESIAN_POINT('Ctrl Pts',(-55.7673330881313,-110.962611747484,
174.985485069079));
#16616=CARTESIAN_POINT('Ctrl Pts',(-55.750363952816,-110.806012352105,174.985485069079));
#16617=CARTESIAN_POINT('Ctrl Pts',(-55.7333536026738,-110.64941790035,174.985485069079));
#16618=CARTESIAN_POINT('Ctrl Pts',(-55.6389642047373,-109.784410209239,
176.985485069079));
#16619=CARTESIAN_POINT('Ctrl Pts',(-55.6389642047373,-109.784410209239,
174.585485069079));
#16620=CARTESIAN_POINT('Ctrl Pts',(-55.6158587430936,-109.573622204912,
176.985485069079));
#16621=CARTESIAN_POINT('Ctrl Pts',(-55.6158587430936,-109.573622204912,
174.585485069079));
#16622=CARTESIAN_POINT('Ctrl Pts',(-55.5927270839073,-109.363293887315,
176.98548506908));
#16623=CARTESIAN_POINT('Ctrl Pts',(-55.5927270839073,-109.363293887315,
174.58548506908));
#16624=CARTESIAN_POINT('Ctrl Pts',(-55.5695693845384,-109.153423842286,
176.98548506908));
#16625=CARTESIAN_POINT('Ctrl Pts',(-55.5695693845384,-109.153423842286,
174.58548506908));
#16626=CARTESIAN_POINT('',(-55.6385532352656,-109.780661063962,176.985485069079));
#16627=CARTESIAN_POINT('',(-55.6219312570818,-109.629147380551,174.985485069079));
#16628=CARTESIAN_POINT('Ctrl Pts',(-55.6385532352656,-109.780661063962,
176.985485069079));
#16629=CARTESIAN_POINT('Ctrl Pts',(-55.6364090528804,-109.761100746612,
176.871529272123));
#16630=CARTESIAN_POINT('Ctrl Pts',(-55.6344206303383,-109.742967391913,
176.757244549389));
#16631=CARTESIAN_POINT('Ctrl Pts',(-55.632624701929,-109.726593308319,176.64274596629));
#16632=CARTESIAN_POINT('Ctrl Pts',(-55.6302616254732,-109.705048345154,
176.492089122433));
#16633=CARTESIAN_POINT('Ctrl Pts',(-55.6282354868976,-109.686582603912,
176.34130394811));
#16634=CARTESIAN_POINT('Ctrl Pts',(-55.6266116662059,-109.671786190867,
176.189750722006));
#16635=CARTESIAN_POINT('Ctrl Pts',(-55.626204109179,-109.668072491355,176.151712912431));
#16636=CARTESIAN_POINT('Ctrl Pts',(-55.6258222679447,-109.664593332989,
176.113663047176));
#16637=CARTESIAN_POINT('Ctrl Pts',(-55.6254668827296,-109.661355382375,
176.07558107738));
#16638=CARTESIAN_POINT('Ctrl Pts',(-55.625268687235,-109.659549603192,176.054343067137));
#16639=CARTESIAN_POINT('Ctrl Pts',(-55.6250787727883,-109.657819324701,
176.033100724868));
#16640=CARTESIAN_POINT('Ctrl Pts',(-55.624897250403,-109.656165545924,176.011850174535));
#16641=CARTESIAN_POINT('Ctrl Pts',(-55.6248563305293,-109.655792741112,
176.007059746982));
#16642=CARTESIAN_POINT('Ctrl Pts',(-55.6248158382756,-109.655423834363,
176.002269038379));
#16643=CARTESIAN_POINT('Ctrl Pts',(-55.6247757748228,-109.655058836301,
175.997478002448));
#16644=CARTESIAN_POINT('Ctrl Pts',(-55.6247531302752,-109.654852533164,
175.994770027129));
#16645=CARTESIAN_POINT('Ctrl Pts',(-55.6247306228264,-109.654647479735,
175.992061960349));
#16646=CARTESIAN_POINT('Ctrl Pts',(-55.6247082526837,-109.654443677878,
175.989353793512));
#16647=CARTESIAN_POINT('Ctrl Pts',(-55.6246975274837,-109.654345966581,
175.988055382898));
#16648=CARTESIAN_POINT('Ctrl Pts',(-55.6246868325191,-109.654248530892,
175.986756735708));
#16649=CARTESIAN_POINT('Ctrl Pts',(-55.6246763889997,-109.654153386119,
175.985484943368));
#16650=CARTESIAN_POINT('Ctrl Pts',(-55.6246679437789,-109.654076446671,
175.984456500102));
#16651=CARTESIAN_POINT('Ctrl Pts',(-55.624659659271,-109.654000971477,175.983445620473));
#16652=CARTESIAN_POINT('Ctrl Pts',(-55.6246516506085,-109.653928009428,
175.98246663173));
#16653=CARTESIAN_POINT('Ctrl Pts',(-55.6246288764581,-109.653720528006,
175.97968269159));
#16654=CARTESIAN_POINT('Ctrl Pts',(-55.6246062215329,-109.653514133448,
175.976898672936));
#16655=CARTESIAN_POINT('Ctrl Pts',(-55.6245836860687,-109.653308827883,
175.974114569615));
#16656=CARTESIAN_POINT('Ctrl Pts',(-55.6245420900418,-109.652929874262,
175.968975663425));
#16657=CARTESIAN_POINT('Ctrl Pts',(-55.624500901285,-109.652554633264,175.963836501813));
#16658=CARTESIAN_POINT('Ctrl Pts',(-55.6244601212647,-109.65218311812,175.958697045889));
#16659=CARTESIAN_POINT('Ctrl Pts',(-55.6242482374254,-109.650252808753,
175.931993585618));
#16660=CARTESIAN_POINT('Ctrl Pts',(-55.6240474178744,-109.64842335603,175.90528595974));
#16661=CARTESIAN_POINT('Ctrl Pts',(-55.623857856037,-109.646696504493,175.878568359176));
#16662=CARTESIAN_POINT('Ctrl Pts',(-55.6234970668234,-109.643409822864,
175.827717290019));
#16663=CARTESIAN_POINT('Ctrl Pts',(-55.6231773197003,-109.640497190402,
175.776866909026));
#16664=CARTESIAN_POINT('Ctrl Pts',(-55.6228997282151,-109.637968646638,
175.725971544764));
#16665=CARTESIAN_POINT('Ctrl Pts',(-55.6215482370463,-109.62565809408,175.478180675772));
#16666=CARTESIAN_POINT('Ctrl Pts',(-55.6212187388722,-109.622657747841,
175.233470911589));
#16667=CARTESIAN_POINT('Ctrl Pts',(-55.6219312570821,-109.629147380551,
174.985485069079));
#16668=CARTESIAN_POINT('',(-55.586709713872,-109.308887482778,176.985485069079));
#16669=CARTESIAN_POINT('Ctrl Pts',(-55.586709713872,-109.308887482778,176.985485069079));
#16670=CARTESIAN_POINT('Ctrl Pts',(-55.6040331133308,-109.466139941617,
176.985485069079));
#16671=CARTESIAN_POINT('Ctrl Pts',(-55.6213141953808,-109.623397813748,
176.985485069079));
#16672=CARTESIAN_POINT('Ctrl Pts',(-55.6385532352656,-109.780661063962,
176.985485069079));
#16673=CARTESIAN_POINT('',(-55.5699812776309,-109.157156757027,174.985485069079));
#16674=CARTESIAN_POINT('Ctrl Pts',(-55.5699812776309,-109.157156757027,
174.98548506908));
#16675=CARTESIAN_POINT('Ctrl Pts',(-55.5732866004807,-109.187112904902,
175.159804470874));
#16676=CARTESIAN_POINT('Ctrl Pts',(-55.5762218608553,-109.213729419147,
175.334889205444));
#16677=CARTESIAN_POINT('Ctrl Pts',(-55.578660281489,-109.235847109079,175.510572458271));
#16678=CARTESIAN_POINT('Ctrl Pts',(-55.5801069603974,-109.248969207492,
175.614802734586));
#16679=CARTESIAN_POINT('Ctrl Pts',(-55.5813766993776,-109.260489063237,
175.71907795542));
#16680=CARTESIAN_POINT('Ctrl Pts',(-55.5824505396604,-109.270232848391,
175.82369743394));
#16681=CARTESIAN_POINT('Ctrl Pts',(-55.5829005685282,-109.274316309098,
175.867541743207));
#16682=CARTESIAN_POINT('Ctrl Pts',(-55.5833156970086,-109.278083353021,
175.911397741191));
#16683=CARTESIAN_POINT('Ctrl Pts',(-55.5836948941706,-109.281524510865,
175.955298099187));
#16684=CARTESIAN_POINT('Ctrl Pts',(-55.5837453433951,-109.281982330074,
175.961138699377));
#16685=CARTESIAN_POINT('Ctrl Pts',(-55.5837951534157,-109.282434351904,
175.966979712571));
#16686=CARTESIAN_POINT('Ctrl Pts',(-55.5838443221141,-109.282880556884,
175.972821222537));
#16687=CARTESIAN_POINT('Ctrl Pts',(-55.583868966911,-109.283104207936,175.975749159043));
#16688=CARTESIAN_POINT('Ctrl Pts',(-55.5838934504385,-109.283326396259,
175.978677202591));
#16689=CARTESIAN_POINT('Ctrl Pts',(-55.5839177724371,-109.283547119468,
175.981605363915));
#16690=CARTESIAN_POINT('Ctrl Pts',(-55.5839285834645,-109.283645230017,
175.982906919464));
#16691=CARTESIAN_POINT('Ctrl Pts',(-55.5839393686461,-109.283743106169,
175.984209282882));
#16692=CARTESIAN_POINT('Ctrl Pts',(-55.5839499020231,-109.283838697322,
175.985484943316));
#16693=CARTESIAN_POINT('Ctrl Pts',(-55.5839585992817,-109.283917625569,
175.986538237873));
#16694=CARTESIAN_POINT('Ctrl Pts',(-55.5839671287816,-109.283995031492,
175.987573324793));
#16695=CARTESIAN_POINT('Ctrl Pts',(-55.583975365368,-109.284069779287,175.988574716349));
#16696=CARTESIAN_POINT('Ctrl Pts',(-55.5839967509971,-109.284263855878,
175.991174748357));
#16697=CARTESIAN_POINT('Ctrl Pts',(-55.5840180319528,-109.284456983142,
175.993774849365));
#16698=CARTESIAN_POINT('Ctrl Pts',(-55.584039208044,-109.284649159328,175.996375024287));
#16699=CARTESIAN_POINT('Ctrl Pts',(-55.5840744020402,-109.28496855009,176.000696433042));
#16700=CARTESIAN_POINT('Ctrl Pts',(-55.5841093062199,-109.285285312331,
176.005018025533));
#16701=CARTESIAN_POINT('Ctrl Pts',(-55.584143919719,-109.285599438132,176.009339824886));
#16702=CARTESIAN_POINT('Ctrl Pts',(-55.5842698791708,-109.286742550346,
176.02506696862));
#16703=CARTESIAN_POINT('Ctrl Pts',(-55.5843919827929,-109.287850690552,
176.040796041382));
#16704=CARTESIAN_POINT('Ctrl Pts',(-55.5845101904938,-109.288923491222,
176.0565282034));
#16705=CARTESIAN_POINT('Ctrl Pts',(-55.584960025238,-109.293005991866,176.116396325553));
#16706=CARTESIAN_POINT('Ctrl Pts',(-55.5853530717745,-109.296573366859,
176.176259980973));
#16707=CARTESIAN_POINT('Ctrl Pts',(-55.5856874617408,-109.299608482482,
176.236191992831));
#16708=CARTESIAN_POINT('Ctrl Pts',(-55.5870865691322,-109.312307585713,
176.486951074261));
#16709=CARTESIAN_POINT('Ctrl Pts',(-55.5874344793557,-109.315466512178,
176.73451470052));
#16710=CARTESIAN_POINT('Ctrl Pts',(-55.5867097138723,-109.308887482778,
176.985485069079));
#16711=CARTESIAN_POINT('Ctrl Pts',(-55.6219312570818,-109.629147380551,
174.985485069079));
#16712=CARTESIAN_POINT('Ctrl Pts',(-55.6046568968532,-109.47181209897,174.985485069079));
#16713=CARTESIAN_POINT('Ctrl Pts',(-55.5873403294727,-109.314481880041,
174.985485069079));
#16714=CARTESIAN_POINT('Ctrl Pts',(-55.5699812776309,-109.157156757027,
174.985485069079));
#16715=CARTESIAN_POINT('Ctrl Pts',(-54.9656605004213,-103.833027927217,
176.985485069079));
#16716=CARTESIAN_POINT('Ctrl Pts',(-54.9656605004213,-103.833027927217,
174.585485069079));
#16717=CARTESIAN_POINT('Ctrl Pts',(-54.9401779838911,-103.614774580036,
176.985485069079));
#16718=CARTESIAN_POINT('Ctrl Pts',(-54.9401779838911,-103.614774580036,
174.585485069079));
#16719=CARTESIAN_POINT('Ctrl Pts',(-54.914666672271,-103.39704157916,176.985485069079));
#16720=CARTESIAN_POINT('Ctrl Pts',(-54.914666672271,-103.39704157916,174.585485069079));
#16721=CARTESIAN_POINT('Ctrl Pts',(-54.8891267634922,-103.179827143433,
176.985485069079));
#16722=CARTESIAN_POINT('Ctrl Pts',(-54.8891267634922,-103.179827143433,
174.585485069079));
#16723=CARTESIAN_POINT('',(-54.9652072510433,-103.829146005559,176.985485069079));
#16724=CARTESIAN_POINT('',(-54.9477711935236,-103.67993499333,174.985485069079));
#16725=CARTESIAN_POINT('Ctrl Pts',(-54.9652072510433,-103.829146005559,
176.985485069079));
#16726=CARTESIAN_POINT('Ctrl Pts',(-54.9603446400948,-103.787500319099,
176.739490147077));
#16727=CARTESIAN_POINT('Ctrl Pts',(-54.9562599984868,-103.752545584536,
176.492377432739));
#16728=CARTESIAN_POINT('Ctrl Pts',(-54.9532994998274,-103.727218214377,
176.24352953951));
#16729=CARTESIAN_POINT('Ctrl Pts',(-54.9525165046112,-103.720519609866,
176.177714035987));
#16730=CARTESIAN_POINT('Ctrl Pts',(-54.951813145893,-103.714503021022,176.111882747266));
#16731=CARTESIAN_POINT('Ctrl Pts',(-54.9511933972497,-103.709202033452,
176.045936596505));
#16732=CARTESIAN_POINT('Ctrl Pts',(-54.9510769059183,-103.708205630948,
176.033540998729));
#16733=CARTESIAN_POINT('Ctrl Pts',(-54.9509633911318,-103.70723470415,176.02114375147));
#16734=CARTESIAN_POINT('Ctrl Pts',(-54.9508528746203,-103.706289436525,
176.008744093197));
#16735=CARTESIAN_POINT('Ctrl Pts',(-54.9508174843107,-103.705986736833,
176.004773394702));
#16736=CARTESIAN_POINT('Ctrl Pts',(-54.950782401975,-103.705686672774,176.000802506865));
#16737=CARTESIAN_POINT('Ctrl Pts',(-54.9507476282943,-103.705389250096,
175.996831404116));
#16738=CARTESIAN_POINT('Ctrl Pts',(-54.9507254845137,-103.705199852184,
175.99430261723));
#16739=CARTESIAN_POINT('Ctrl Pts',(-54.9507034659822,-103.705011526117,
175.991773753038));
#16740=CARTESIAN_POINT('Ctrl Pts',(-54.9506815728693,-103.704824273326,
175.989244804546));
#16741=CARTESIAN_POINT('Ctrl Pts',(-54.9506706715899,-103.704731034188,
175.987985560415));
#16742=CARTESIAN_POINT('Ctrl Pts',(-54.9506597749779,-103.704637835112,
175.986723190717));
#16743=CARTESIAN_POINT('Ctrl Pts',(-54.9506491166976,-103.704546674627,
175.985484941713));
#16744=CARTESIAN_POINT('Ctrl Pts',(-54.9506394019653,-103.704463584327,
175.984356311458));
#16745=CARTESIAN_POINT('Ctrl Pts',(-54.9506298806488,-103.70438214843,175.983247723187));
#16746=CARTESIAN_POINT('Ctrl Pts',(-54.9506207267441,-103.704303855104,
175.982179810625));
#16747=CARTESIAN_POINT('Ctrl Pts',(-54.9505941095538,-103.704076198336,
175.97907459676));
#16748=CARTESIAN_POINT('Ctrl Pts',(-54.9505676481464,-103.703849874815,
175.975969288503));
#16749=CARTESIAN_POINT('Ctrl Pts',(-54.9505413428546,-103.703624887355,
175.972863877515));
#16750=CARTESIAN_POINT('Ctrl Pts',(-54.9504845796731,-103.703139395535,
175.966162830107));
#16751=CARTESIAN_POINT('Ctrl Pts',(-54.9504285440011,-103.702660129853,
175.959461372579));
#16752=CARTESIAN_POINT('Ctrl Pts',(-54.9503732391284,-103.702187118158,
175.952759420293));
#16753=CARTESIAN_POINT('Ctrl Pts',(-54.9497915780554,-103.697212285439,
175.88227259756));
#16754=CARTESIAN_POINT('Ctrl Pts',(-54.9492913032303,-103.692933925243,
175.811797486704));
#16755=CARTESIAN_POINT('Ctrl Pts',(-54.9488756720445,-103.689379602438,
175.741221887012));
#16756=CARTESIAN_POINT('Ctrl Pts',(-54.9473863602973,-103.676643564123,
175.488331648524));
#16757=CARTESIAN_POINT('Ctrl Pts',(-54.9470101313529,-103.673427333826,
175.238593067858));
#16758=CARTESIAN_POINT('Ctrl Pts',(-54.9477711935239,-103.67993499333,174.985485069079));
#16759=CARTESIAN_POINT('',(-54.9071900358701,-103.333580645004,176.985485069079));
#16760=CARTESIAN_POINT('Ctrl Pts',(-54.9071900358701,-103.333580645004,
176.985485069079));
#16761=CARTESIAN_POINT('Ctrl Pts',(-54.9265798996307,-103.498762601146,
176.985485069079));
#16762=CARTESIAN_POINT('Ctrl Pts',(-54.9459188500188,-103.663951070186,
176.985485069079));
#16763=CARTESIAN_POINT('Ctrl Pts',(-54.9652072510433,-103.829146005559,
176.985485069079));
#16764=CARTESIAN_POINT('',(-54.8895810276286,-103.183690695987,174.985485069079));
#16765=CARTESIAN_POINT('Ctrl Pts',(-54.8895810276286,-103.183690695987,
174.985485069079));
#16766=CARTESIAN_POINT('Ctrl Pts',(-54.894579533373,-103.226204268245,175.235671327022));
#16767=CARTESIAN_POINT('Ctrl Pts',(-54.8987611854365,-103.261799603572,
175.487040663794));
#16768=CARTESIAN_POINT('Ctrl Pts',(-54.9017619269949,-103.287350165154,
175.740218794686));
#16769=CARTESIAN_POINT('Ctrl Pts',(-54.9025899334085,-103.294400432046,
175.810079231545));
#16770=CARTESIAN_POINT('Ctrl Pts',(-54.9033268465538,-103.300675857414,
175.87995195485));
#16771=CARTESIAN_POINT('Ctrl Pts',(-54.9039680529975,-103.306136673011,
175.949958567431));
#16772=CARTESIAN_POINT('Ctrl Pts',(-54.9040354843144,-103.306710949815,
175.957320686338));
#16773=CARTESIAN_POINT('Ctrl Pts',(-54.9041018493881,-103.307276151311,
175.964683431554));
#16774=CARTESIAN_POINT('Ctrl Pts',(-54.904167143829,-103.307832239617,175.972046966102));
#16775=CARTESIAN_POINT('Ctrl Pts',(-54.9041956515931,-103.30807502957,175.975261909108));
#16776=CARTESIAN_POINT('Ctrl Pts',(-54.9042239550488,-103.308316080457,
175.978476977567));
#16777=CARTESIAN_POINT('Ctrl Pts',(-54.9042520538418,-103.308555389218,
175.981692185214));
#16778=CARTESIAN_POINT('Ctrl Pts',(-54.9042631575422,-103.308649956013,
175.982962727421));
#16779=CARTESIAN_POINT('Ctrl Pts',(-54.9042742534349,-103.308744456458,
175.984236107471));
#16780=CARTESIAN_POINT('Ctrl Pts',(-54.904285104508,-103.308836871984,175.98548494154));
#16781=CARTESIAN_POINT('Ctrl Pts',(-54.9042948652852,-103.308920001767,
175.986608295046));
#16782=CARTESIAN_POINT('Ctrl Pts',(-54.9043044325544,-103.30900148361,175.987711784495));
#16783=CARTESIAN_POINT('Ctrl Pts',(-54.9043136366808,-103.30907987276,175.988775477043));
#16784=CARTESIAN_POINT('Ctrl Pts',(-54.9043349662627,-103.309261531262,
175.991240471174));
#16785=CARTESIAN_POINT('Ctrl Pts',(-54.9043561967022,-103.309442345925,
175.993705526031));
#16786=CARTESIAN_POINT('Ctrl Pts',(-54.9043773278324,-103.309622315315,
175.99617064576));
#16787=CARTESIAN_POINT('Ctrl Pts',(-54.9044093023417,-103.309894635484,
175.999900734628));
#16788=CARTESIAN_POINT('Ctrl Pts',(-54.904441049357,-103.31016501933,176.003630958694));
#16789=CARTESIAN_POINT('Ctrl Pts',(-54.9044725683072,-103.31043346194,176.0073613325));
#16790=CARTESIAN_POINT('Ctrl Pts',(-54.9045625504215,-103.311199827362,
176.018011018467));
#16791=CARTESIAN_POINT('Ctrl Pts',(-54.9046506715745,-103.311950352705,
176.028661666441));
#16792=CARTESIAN_POINT('Ctrl Pts',(-54.9047369188309,-103.312684926642,
176.039313624502));
#16793=CARTESIAN_POINT('Ctrl Pts',(-54.9052649957913,-103.317182595187,
176.104533712293));
#16794=CARTESIAN_POINT('Ctrl Pts',(-54.9057223621618,-103.321078338012,
176.169746019421));
#16795=CARTESIAN_POINT('Ctrl Pts',(-54.9061064975074,-103.324350456313,
176.235041316554));
#16796=CARTESIAN_POINT('Ctrl Pts',(-54.9075838256808,-103.336934543165,
176.486157448245));
#16797=CARTESIAN_POINT('Ctrl Pts',(-54.9079526518267,-103.340077358802,
176.73415655439));
#16798=CARTESIAN_POINT('Ctrl Pts',(-54.9071900358704,-103.333580645004,
176.985485069079));
#16799=CARTESIAN_POINT('Ctrl Pts',(-54.9477711935236,-103.67993499333,174.985485069079));
#16800=CARTESIAN_POINT('Ctrl Pts',(-54.928425440487,-103.514514113942,174.985485069079));
#16801=CARTESIAN_POINT('Ctrl Pts',(-54.9090288411297,-103.349099333454,
174.985485069079));
#16802=CARTESIAN_POINT('Ctrl Pts',(-54.8895810276286,-103.183690695987,
174.985485069079));
#16803=CARTESIAN_POINT('Ctrl Pts',(-55.1378236961386,-105.319345570968,
176.985485069079));
#16804=CARTESIAN_POINT('Ctrl Pts',(-55.1378236961386,-105.319345570968,
174.585485069079));
#16805=CARTESIAN_POINT('Ctrl Pts',(-55.1130435723412,-105.103705439537,
176.985485069079));
#16806=CARTESIAN_POINT('Ctrl Pts',(-55.1130435723412,-105.103705439537,
174.585485069079));
#16807=CARTESIAN_POINT('Ctrl Pts',(-55.0882355096573,-104.888566306789,
176.985485069079));
#16808=CARTESIAN_POINT('Ctrl Pts',(-55.0882355096573,-104.888566306789,
174.585485069079));
#16809=CARTESIAN_POINT('Ctrl Pts',(-55.0633996930072,-104.673926509197,
176.985485069079));
#16810=CARTESIAN_POINT('Ctrl Pts',(-55.0633996930072,-104.673926509197,
174.585485069079));
#16811=CARTESIAN_POINT('',(-55.1373829400023,-105.315510127391,176.985485069079));
#16812=CARTESIAN_POINT('',(-55.1201342919917,-105.165536169418,174.985485069079));
#16813=CARTESIAN_POINT('Ctrl Pts',(-55.1373829400023,-105.315510127391,
176.985485069079));
#16814=CARTESIAN_POINT('Ctrl Pts',(-55.1325913532206,-105.273814769704,
176.740328641451));
#16815=CARTESIAN_POINT('Ctrl Pts',(-55.1285604769881,-105.238766921808,
176.494015528965));
#16816=CARTESIAN_POINT('Ctrl Pts',(-55.1256334249619,-105.213324102528,
176.245996586915));
#16817=CARTESIAN_POINT('Ctrl Pts',(-55.1248690958891,-105.206680323636,
176.181232419308));
#16818=CARTESIAN_POINT('Ctrl Pts',(-55.1241809619153,-105.200699557015,
176.116451480769));
#16819=CARTESIAN_POINT('Ctrl Pts',(-55.12357283239,-105.195414522072,176.051559076556));
#16820=CARTESIAN_POINT('Ctrl Pts',(-55.1234413510252,-105.194271864828,
176.037528937381));
#16821=CARTESIAN_POINT('Ctrl Pts',(-55.1233136386414,-105.193161983333,
176.023496715598));
#16822=CARTESIAN_POINT('Ctrl Pts',(-55.1231897269403,-105.192085149581,
176.009461299477));
#16823=CARTESIAN_POINT('Ctrl Pts',(-55.123153026971,-105.191766214683,176.005304312389));
#16824=CARTESIAN_POINT('Ctrl Pts',(-55.1231166610312,-105.191450184242,
176.001147116187));
#16825=CARTESIAN_POINT('Ctrl Pts',(-55.1230806299025,-105.191137064961,
175.996989681169));
#16826=CARTESIAN_POINT('Ctrl Pts',(-55.1230583616824,-105.190943548706,
175.994420272955));
#16827=CARTESIAN_POINT('Ctrl Pts',(-55.1230362214369,-105.190751145181,
175.991850784019));
#16828=CARTESIAN_POINT('Ctrl Pts',(-55.1230142093449,-105.19055985592,175.989281207067));
#16829=CARTESIAN_POINT('Ctrl Pts',(-55.1230033113244,-105.190465150052,
175.988009028935));
#16830=CARTESIAN_POINT('Ctrl Pts',(-55.1229924249308,-105.190370545369,
175.986734466882));
#16831=CARTESIAN_POINT('Ctrl Pts',(-55.1229817827353,-105.190278062947,
175.985484942294));
#16832=CARTESIAN_POINT('Ctrl Pts',(-55.1229724066987,-105.190196583653,
175.984384080328));
#16833=CARTESIAN_POINT('Ctrl Pts',(-55.1229632158595,-105.190116713862,
175.983302655394));
#16834=CARTESIAN_POINT('Ctrl Pts',(-55.122954366653,-105.190039813004,175.982259421452));
#16835=CARTESIAN_POINT('Ctrl Pts',(-55.1229288184682,-105.189817795657,
175.979247543101));
#16836=CARTESIAN_POINT('Ctrl Pts',(-55.122903415208,-105.189597038515,175.976235574927));
#16837=CARTESIAN_POINT('Ctrl Pts',(-55.1228781571759,-105.189377544189,
175.973223509272));
#16838=CARTESIAN_POINT('Ctrl Pts',(-55.1228259520709,-105.188923877635,
175.966997956796));
#16839=CARTESIAN_POINT('Ctrl Pts',(-55.1227743678426,-105.188475609844,
175.960772043696));
#16840=CARTESIAN_POINT('Ctrl Pts',(-55.1227234071325,-105.188032763539,
175.95454570169));
#16841=CARTESIAN_POINT('Ctrl Pts',(-55.1222451085664,-105.183876370262,
175.896107535319));
#16842=CARTESIAN_POINT('Ctrl Pts',(-55.1218220467802,-105.18020025562,175.837669539353));
#16843=CARTESIAN_POINT('Ctrl Pts',(-55.1214561353611,-105.177020875394,
175.779168406242));
#16844=CARTESIAN_POINT('Ctrl Pts',(-55.1204759308218,-105.168503942696,
175.622455406208));
#16845=CARTESIAN_POINT('Ctrl Pts',(-55.119912702985,-105.16361104624,175.46638507564));
#16846=CARTESIAN_POINT('Ctrl Pts',(-55.1197837579081,-105.162490824725,
175.309429212081));
#16847=CARTESIAN_POINT('Ctrl Pts',(-55.1196949631213,-105.161719412329,
175.201345500861));
#16848=CARTESIAN_POINT('Ctrl Pts',(-55.1198126567061,-105.162741844194,
175.093530246589));
#16849=CARTESIAN_POINT('Ctrl Pts',(-55.120134291992,-105.165536169417,174.985485069079));
#16850=CARTESIAN_POINT('',(-55.0812452693713,-104.828281539026,176.985485069079));
#16851=CARTESIAN_POINT('Ctrl Pts',(-55.0812452693713,-104.828281539026,
176.985485069079));
#16852=CARTESIAN_POINT('Ctrl Pts',(-55.1000058573857,-104.990684924282,
176.985485069079));
#16853=CARTESIAN_POINT('Ctrl Pts',(-55.118718302742,-105.153094468003,176.985485069079));
#16854=CARTESIAN_POINT('Ctrl Pts',(-55.1373829400023,-105.315510127391,
176.985485069079));
#16855=CARTESIAN_POINT('',(-55.0638414338548,-104.677744265764,174.985485069079));
#16856=CARTESIAN_POINT('Ctrl Pts',(-55.0638414338548,-104.677744265764,
174.985485069079));
#16857=CARTESIAN_POINT('Ctrl Pts',(-55.0687838687883,-104.720460258196,
175.235872171748));
#16858=CARTESIAN_POINT('Ctrl Pts',(-55.0729207002077,-104.756243083222,
175.487478675512));
#16859=CARTESIAN_POINT('Ctrl Pts',(-55.075887709271,-104.781914641058,175.740891960796));
#16860=CARTESIAN_POINT('Ctrl Pts',(-55.0767089826743,-104.789020574078,
175.811037210384));
#16861=CARTESIAN_POINT('Ctrl Pts',(-55.0774394594947,-104.795341706919,
175.881194595647));
#16862=CARTESIAN_POINT('Ctrl Pts',(-55.0780744901831,-104.800837317194,
175.951488371148));
#16863=CARTESIAN_POINT('Ctrl Pts',(-55.078137016347,-104.801378424002,175.958409611662));
#16864=CARTESIAN_POINT('Ctrl Pts',(-55.0781986103504,-104.801911468507,
175.96533141422));
#16865=CARTESIAN_POINT('Ctrl Pts',(-55.0782592685639,-104.802436418886,
175.972253915646));
#16866=CARTESIAN_POINT('Ctrl Pts',(-55.0782867446598,-104.802674203452,
175.975389571999));
#16867=CARTESIAN_POINT('Ctrl Pts',(-55.0783140285515,-104.802910325545,
175.978525348855));
#16868=CARTESIAN_POINT('Ctrl Pts',(-55.0783411199121,-104.803144782296,
175.981661259125));
#16869=CARTESIAN_POINT('Ctrl Pts',(-55.0783521912824,-104.803240597252,
175.982942805102));
#16870=CARTESIAN_POINT('Ctrl Pts',(-55.0783632487692,-104.803336292205,
175.984226541533));
#16871=CARTESIAN_POINT('Ctrl Pts',(-55.07837405698,-104.803429829985,175.985484942154));
#16872=CARTESIAN_POINT('Ctrl Pts',(-55.0783835000685,-104.803511553552,
175.986584401511));
#16873=CARTESIAN_POINT('Ctrl Pts',(-55.0783927572475,-104.803591668305,
175.987664518065));
#16874=CARTESIAN_POINT('Ctrl Pts',(-55.078401674109,-104.803668837928,175.988706932021));
#16875=CARTESIAN_POINT('Ctrl Pts',(-55.0784230107973,-104.803853493056,
175.991201269499));
#16876=CARTESIAN_POINT('Ctrl Pts',(-55.0784442471903,-104.80403728074,175.993695669732));
#16877=CARTESIAN_POINT('Ctrl Pts',(-55.0784653831148,-104.804220199467,
175.996190136949));
#16878=CARTESIAN_POINT('Ctrl Pts',(-55.0784980879095,-104.804503239814,
176.000049965188));
#16879=CARTESIAN_POINT('Ctrl Pts',(-55.0785305520266,-104.804784198525,
176.003909939035));
#16880=CARTESIAN_POINT('Ctrl Pts',(-55.0785627748351,-104.805063070084,
176.007770074744));
#16881=CARTESIAN_POINT('Ctrl Pts',(-55.0786597880118,-104.805902668401,
176.01939178135));
#16882=CARTESIAN_POINT('Ctrl Pts',(-55.0787546111034,-104.806723323977,
176.031014620741));
#16883=CARTESIAN_POINT('Ctrl Pts',(-55.0788472273842,-104.807524890555,
176.042639049868));
#16884=CARTESIAN_POINT('Ctrl Pts',(-55.0793396929952,-104.811787035087,
176.104449258049));
#16885=CARTESIAN_POINT('Ctrl Pts',(-55.0797693684961,-104.815506036955,
176.166254628543));
#16886=CARTESIAN_POINT('Ctrl Pts',(-55.0801341086664,-104.818663131394,
176.228133032237));
#16887=CARTESIAN_POINT('Ctrl Pts',(-55.0816280794429,-104.831594547275,
176.481586132073));
#16888=CARTESIAN_POINT('Ctrl Pts',(-55.0820065361088,-104.834871540102,
176.731806878011));
#16889=CARTESIAN_POINT('Ctrl Pts',(-55.0812452693716,-104.828281539026,
176.985485069079));
#16890=CARTESIAN_POINT('Ctrl Pts',(-55.1201342919917,-105.165536169418,
174.985485069079));
#16891=CARTESIAN_POINT('Ctrl Pts',(-55.1014181855903,-105.00293308916,174.985485069079));
#16892=CARTESIAN_POINT('Ctrl Pts',(-55.0826540121559,-104.840335774435,
174.985485069079));
#16893=CARTESIAN_POINT('Ctrl Pts',(-55.0638414338548,-104.677744265764,
174.985485069079));
#16894=CARTESIAN_POINT('Ctrl Pts',(-55.3073953193163,-106.806696489204,
176.985485069079));
#16895=CARTESIAN_POINT('Ctrl Pts',(-55.3073953193163,-106.806696489204,
174.585485069079));
#16896=CARTESIAN_POINT('Ctrl Pts',(-55.2832425016958,-106.593163773849,
176.985485069079));
#16897=CARTESIAN_POINT('Ctrl Pts',(-55.2832425016958,-106.593163773849,
174.585485069079));
#16898=CARTESIAN_POINT('Ctrl Pts',(-55.2590624577512,-106.380115649896,
176.98548506908));
#16899=CARTESIAN_POINT('Ctrl Pts',(-55.2590624577512,-106.380115649896,
174.585485069079));
#16900=CARTESIAN_POINT('Ctrl Pts',(-55.2348553614763,-106.167550552635,
176.98548506908));
#16901=CARTESIAN_POINT('Ctrl Pts',(-55.2348553614763,-106.167550552635,
174.585485069079));
#16902=CARTESIAN_POINT('',(-55.3069657208749,-106.802898527582,176.985485069079));
#16903=CARTESIAN_POINT('',(-55.2899155902424,-106.652286416981,174.985485069079));
#16904=CARTESIAN_POINT('Ctrl Pts',(-55.3069657208749,-106.802898527582,
176.985485069079));
#16905=CARTESIAN_POINT('Ctrl Pts',(-55.3021846112535,-106.76063090408,176.7379137386));
#16906=CARTESIAN_POINT('Ctrl Pts',(-55.2981676012828,-106.725146921386,
176.489140583006));
#16907=CARTESIAN_POINT('Ctrl Pts',(-55.2952666343776,-106.699528891617,
176.238615443194));
#16908=CARTESIAN_POINT('Ctrl Pts',(-55.2945707003288,-106.693383196143,
176.178515145408));
#16909=CARTESIAN_POINT('Ctrl Pts',(-55.2939397417985,-106.687811887529,
176.118397421427));
#16910=CARTESIAN_POINT('Ctrl Pts',(-55.2933767926389,-106.682841442936,
176.058185956496));
#16911=CARTESIAN_POINT('Ctrl Pts',(-55.2932273308083,-106.681521800238,
176.042199937835));
#16912=CARTESIAN_POINT('Ctrl Pts',(-55.293082699797,-106.680244837964,176.026211274459));
#16913=CARTESIAN_POINT('Ctrl Pts',(-55.2929429467073,-106.679010966758,
176.010218314697));
#16914=CARTESIAN_POINT('Ctrl Pts',(-55.2929048856235,-106.678674927852,
176.005862708802));
#16915=CARTESIAN_POINT('Ctrl Pts',(-55.2928671871104,-106.678342091856,
176.001506871925));
#16916=CARTESIAN_POINT('Ctrl Pts',(-55.2928298520657,-106.678012466596,
175.997150769662));
#16917=CARTESIAN_POINT('Ctrl Pts',(-55.2928074568339,-106.677814742603,
175.994537784448));
#16918=CARTESIAN_POINT('Ctrl Pts',(-55.2927851924799,-106.677618174731,
175.99192471504));
#16919=CARTESIAN_POINT('Ctrl Pts',(-55.2927630591915,-106.677422764618,
175.989311553739));
#16920=CARTESIAN_POINT('Ctrl Pts',(-55.2927521482605,-106.67732643432,175.988023357328));
#16921=CARTESIAN_POINT('Ctrl Pts',(-55.2927413177775,-106.67723081443,175.986740835906));
#16922=CARTESIAN_POINT('Ctrl Pts',(-55.2927307423378,-106.677137446396,
175.985484942761));
#16923=CARTESIAN_POINT('Ctrl Pts',(-55.2927237094211,-106.677075354453,
175.984649744227));
#16924=CARTESIAN_POINT('Ctrl Pts',(-55.2927167867966,-106.677014236315,
175.983826323883));
#16925=CARTESIAN_POINT('Ctrl Pts',(-55.2927100251261,-106.676954539256,
175.983020844777));
#16926=CARTESIAN_POINT('Ctrl Pts',(-55.292686356663,-106.676745576449,175.980201356218));
#16927=CARTESIAN_POINT('Ctrl Pts',(-55.2926628136723,-106.6765377221,175.977381788001));
#16928=CARTESIAN_POINT('Ctrl Pts',(-55.2926393964027,-106.676330978384,
175.974562133813));
#16929=CARTESIAN_POINT('Ctrl Pts',(-55.292595410732,-106.675942642716,175.969265855355));
#16930=CARTESIAN_POINT('Ctrl Pts',(-55.2925518689223,-106.675558228158,
175.963969309127));
#16931=CARTESIAN_POINT('Ctrl Pts',(-55.2925087726015,-106.675177748937,
175.958672453013));
#16932=CARTESIAN_POINT('Ctrl Pts',(-55.2922679928291,-106.673052005984,
175.929078840673));
#16933=CARTESIAN_POINT('Ctrl Pts',(-55.2920411600593,-106.671049466951,
175.899480614883));
#16934=CARTESIAN_POINT('Ctrl Pts',(-55.2918285395228,-106.669172449607,
175.869869906562));
#16935=CARTESIAN_POINT('Ctrl Pts',(-55.2914493101741,-106.665824607123,
175.817056336345));
#16936=CARTESIAN_POINT('Ctrl Pts',(-55.2911155951723,-106.662878742094,
175.764245125515));
#16937=CARTESIAN_POINT('Ctrl Pts',(-55.2908286328295,-106.6603456714,175.711385142418));
#16938=CARTESIAN_POINT('Ctrl Pts',(-55.2895101725791,-106.648707374234,
175.468517782654));
#16939=CARTESIAN_POINT('Ctrl Pts',(-55.2891999599628,-106.645969953786,
175.228522961519));
#16940=CARTESIAN_POINT('Ctrl Pts',(-55.2899155902426,-106.652286416981,
174.985485069079));
#16941=CARTESIAN_POINT('',(-55.2524742173424,-106.322390962095,176.985485069079));
#16942=CARTESIAN_POINT('Ctrl Pts',(-55.2524742173424,-106.322390962095,
176.985485069079));
#16943=CARTESIAN_POINT('Ctrl Pts',(-55.2706837641386,-106.482554303022,
176.985485069079));
#16944=CARTESIAN_POINT('Ctrl Pts',(-55.288847495167,-106.642723504755,176.985485069079));
#16945=CARTESIAN_POINT('Ctrl Pts',(-55.3069657208749,-106.802898527582,
176.985485069079));
#16946=CARTESIAN_POINT('',(-55.2352859196244,-106.171331405697,174.985485069079));
#16947=CARTESIAN_POINT('Ctrl Pts',(-55.2352859196244,-106.171331405697,
174.985485069079));
#16948=CARTESIAN_POINT('Ctrl Pts',(-55.2401761452878,-106.214274725582,
175.236405579021));
#16949=CARTESIAN_POINT('Ctrl Pts',(-55.2442697085661,-106.250251755796,
175.488576301999));
#16950=CARTESIAN_POINT('Ctrl Pts',(-55.2472018779028,-106.276029153754,
175.742561083287));
#16951=CARTESIAN_POINT('Ctrl Pts',(-55.2480105996487,-106.28313881895,175.812612636308));
#16952=CARTESIAN_POINT('Ctrl Pts',(-55.2487298340075,-106.289462577533,
175.882676256102));
#16953=CARTESIAN_POINT('Ctrl Pts',(-55.2493549857083,-106.294959540506,
175.952876754899));
#16954=CARTESIAN_POINT('Ctrl Pts',(-55.2494130860916,-106.295470417555,
175.959401052735));
#16955=CARTESIAN_POINT('Ctrl Pts',(-55.2494703678393,-106.295974100495,
175.96592585647));
#16956=CARTESIAN_POINT('Ctrl Pts',(-55.2495268279332,-106.29647056244,175.972451281598));
#16957=CARTESIAN_POINT('Ctrl Pts',(-55.2495533179369,-106.296703492954,
175.975512887116));
#16958=CARTESIAN_POINT('Ctrl Pts',(-55.2495796268868,-106.296934832301,
175.978574608341));
#16959=CARTESIAN_POINT('Ctrl Pts',(-55.2496057544813,-106.297164577793,
175.981636457498));
#16960=CARTESIAN_POINT('Ctrl Pts',(-55.2496167657949,-106.297261402614,
175.982926854955));
#16961=CARTESIAN_POINT('Ctrl Pts',(-55.2496277580784,-106.29735806025,175.984218873501));
#16962=CARTESIAN_POINT('Ctrl Pts',(-55.2496384985501,-106.29745250379,175.985484942653));
#16963=CARTESIAN_POINT('Ctrl Pts',(-55.24964765888,-106.297533052764,175.986564747277));
#16964=CARTESIAN_POINT('Ctrl Pts',(-55.2496566402325,-106.297612028052,
175.987625673427));
#16965=CARTESIAN_POINT('Ctrl Pts',(-55.2496653005445,-106.297688180439,
175.988650615149));
#16966=CARTESIAN_POINT('Ctrl Pts',(-55.2496866484448,-106.297875898109,
175.991177123873));
#16967=CARTESIAN_POINT('Ctrl Pts',(-55.2497078947491,-106.29806272298,175.993703697114));
#16968=CARTESIAN_POINT('Ctrl Pts',(-55.2497290392808,-106.298248653482,
175.996230339542));
#16969=CARTESIAN_POINT('Ctrl Pts',(-55.2497625202032,-106.298543061741,
176.000231105349));
#16970=CARTESIAN_POINT('Ctrl Pts',(-55.2497957458191,-106.29883522639,176.004232028344));
#16971=CARTESIAN_POINT('Ctrl Pts',(-55.2498287154289,-106.299125141216,
176.008233126624));
#16972=CARTESIAN_POINT('Ctrl Pts',(-55.249933865528,-106.30004976765,176.020993844248));
#16973=CARTESIAN_POINT('Ctrl Pts',(-55.2500364079953,-106.300951477765,
176.033755904728));
#16974=CARTESIAN_POINT('Ctrl Pts',(-55.2501363208663,-106.301830076432,
176.046519918487));
#16975=CARTESIAN_POINT('Ctrl Pts',(-55.2506462795165,-106.306314473544,
176.111667873496));
#16976=CARTESIAN_POINT('Ctrl Pts',(-55.2510872689855,-106.310192695347,
176.176807217008));
#16977=CARTESIAN_POINT('Ctrl Pts',(-55.2514568274136,-106.313442863289,
176.242030598198));
#16978=CARTESIAN_POINT('Ctrl Pts',(-55.2528664368204,-106.325840002566,
176.490812616604));
#16979=CARTESIAN_POINT('Ctrl Pts',(-55.253212525286,-106.328884801187,176.736501928978));
#16980=CARTESIAN_POINT('Ctrl Pts',(-55.2524742173427,-106.322390962095,
176.985485069079));
#16981=CARTESIAN_POINT('Ctrl Pts',(-55.2899155902424,-106.652286416981,
174.985485069079));
#16982=CARTESIAN_POINT('Ctrl Pts',(-55.2717515343084,-106.491962582169,
174.985485069079));
#16983=CARTESIAN_POINT('Ctrl Pts',(-55.2535417485206,-106.33164423255,174.985485069079));
#16984=CARTESIAN_POINT('Ctrl Pts',(-55.2352859196244,-106.171331405697,
174.985485069079));
#16985=CARTESIAN_POINT('Ctrl Pts',(-55.4744258120625,-108.295058418442,
176.985485069079));
#16986=CARTESIAN_POINT('Ctrl Pts',(-55.4744258120625,-108.295058418442,
174.585485069079));
#16987=CARTESIAN_POINT('Ctrl Pts',(-55.4508297883282,-108.083139316849,
176.985485069079));
#16988=CARTESIAN_POINT('Ctrl Pts',(-55.4508297883282,-108.083139316849,
174.585485069079));
#16989=CARTESIAN_POINT('Ctrl Pts',(-55.4272071161424,-107.871691103985,
176.985485069079));
#16990=CARTESIAN_POINT('Ctrl Pts',(-55.4272071161424,-107.871691103985,
174.585485069079));
#16991=CARTESIAN_POINT('Ctrl Pts',(-55.403557960387,-107.660712297587,176.985485069079));
#16992=CARTESIAN_POINT('Ctrl Pts',(-55.403557960387,-107.660712297587,174.585485069079));
#16993=CARTESIAN_POINT('',(-55.4740061171306,-108.291289156015,176.985485069079));
#16994=CARTESIAN_POINT('',(-55.4571650701271,-108.140163914373,174.985485069079));
#16995=CARTESIAN_POINT('Ctrl Pts',(-55.4740061171306,-108.291289156015,
176.985485069079));
#16996=CARTESIAN_POINT('Ctrl Pts',(-55.4693413328948,-108.24939575857,176.740856007555));
#16997=CARTESIAN_POINT('Ctrl Pts',(-55.4654107951634,-108.214124398444,
176.495008193215));
#16998=CARTESIAN_POINT('Ctrl Pts',(-55.4625532189185,-108.188488942206,
176.247483542904));
#16999=CARTESIAN_POINT('Ctrl Pts',(-55.4618556309792,-108.182230846687,
176.187058134815));
#17000=CARTESIAN_POINT('Ctrl Pts',(-55.461222711051,-108.176553506821,176.126614262712));
#17001=CARTESIAN_POINT('Ctrl Pts',(-55.4606575648579,-108.171484461937,
176.066074873696));
#17002=CARTESIAN_POINT('Ctrl Pts',(-55.4604862720825,-108.169948061662,
176.047725710083));
#17003=CARTESIAN_POINT('Ctrl Pts',(-55.4603212556149,-108.168467993661,
176.029373169598));
#17004=CARTESIAN_POINT('Ctrl Pts',(-55.4601625869058,-108.167044890835,
176.011014750052));
#17005=CARTESIAN_POINT('Ctrl Pts',(-55.4601231175954,-108.166690889801,
176.006448038934));
#17006=CARTESIAN_POINT('Ctrl Pts',(-55.4600840420122,-108.166340422096,
176.001881072887));
#17007=CARTESIAN_POINT('Ctrl Pts',(-55.4600453611864,-108.165993496843,
175.997313812018));
#17008=CARTESIAN_POINT('Ctrl Pts',(-55.4600228395146,-108.165791501758,
175.994654552605));
#17009=CARTESIAN_POINT('Ctrl Pts',(-55.4600004517715,-108.165590708515,
175.991995205391));
#17010=CARTESIAN_POINT('Ctrl Pts',(-55.4599781981548,-108.165391118863,
175.989335762263));
#17011=CARTESIAN_POINT('Ctrl Pts',(-55.4599673907826,-108.165294189017,
175.988044215281));
#17012=CARTESIAN_POINT('Ctrl Pts',(-55.4599566054665,-108.16519745714,175.986751447536));
#17013=CARTESIAN_POINT('Ctrl Pts',(-55.4599460696997,-108.165102963572,
175.985484943119));
#17014=CARTESIAN_POINT('Ctrl Pts',(-55.4599372288567,-108.165023671498,
175.984422185476));
#17015=CARTESIAN_POINT('Ctrl Pts',(-55.459928559729,-108.164945919612,175.98337792344));
#17016=CARTESIAN_POINT('Ctrl Pts',(-55.4599201945696,-108.16487089405,175.982368397651));
#17017=CARTESIAN_POINT('Ctrl Pts',(-55.4598965177436,-108.164658540993,
175.979511026362));
#17018=CARTESIAN_POINT('Ctrl Pts',(-55.4598729681959,-108.164447330186,
175.97665357274));
#17019=CARTESIAN_POINT('Ctrl Pts',(-55.4598495461846,-108.16423726392,175.973796030276));
#17020=CARTESIAN_POINT('Ctrl Pts',(-55.4598046375839,-108.16383448971,175.968317071527));
#17021=CARTESIAN_POINT('Ctrl Pts',(-55.459760198168,-108.163435926071,175.962837825568));
#17022=CARTESIAN_POINT('Ctrl Pts',(-55.4597162297266,-108.163041588893,
175.957358245394));
#17023=CARTESIAN_POINT('Ctrl Pts',(-55.4594468504626,-108.160625622909,
175.923786773984));
#17024=CARTESIAN_POINT('Ctrl Pts',(-55.4591952088867,-108.158368831915,
175.890210139137));
#17025=CARTESIAN_POINT('Ctrl Pts',(-55.4589616862943,-108.156274601051,
175.856616688176));
#17026=CARTESIAN_POINT('Ctrl Pts',(-55.4584694489019,-108.151860215576,
175.785805754904));
#17027=CARTESIAN_POINT('Ctrl Pts',(-55.4580584070155,-108.148174292196,
175.715019325924));
#17028=CARTESIAN_POINT('Ctrl Pts',(-55.4577313114708,-108.145241240388,
175.644129208805));
#17029=CARTESIAN_POINT('Ctrl Pts',(-55.4567150497223,-108.136128464605,
175.423878839963));
#17030=CARTESIAN_POINT('Ctrl Pts',(-55.4565239118472,-108.134414983333,
175.205818800274));
#17031=CARTESIAN_POINT('Ctrl Pts',(-55.4571650701274,-108.140163914373,
174.985485069079));
#17032=CARTESIAN_POINT('',(-55.4209415581549,-107.815922027774,176.985485069079));
#17033=CARTESIAN_POINT('Ctrl Pts',(-55.4209415581549,-107.815922027774,
176.985485069079));
#17034=CARTESIAN_POINT('Ctrl Pts',(-55.4386735345253,-107.974372135515,
176.98548506908));
#17035=CARTESIAN_POINT('Ctrl Pts',(-55.4563616238889,-108.132827857332,
176.985485069079));
#17036=CARTESIAN_POINT('Ctrl Pts',(-55.4740061171306,-108.291289156015,
176.985485069079));
#17037=CARTESIAN_POINT('',(-55.4039785947519,-107.664464934554,174.985485069079));
#17038=CARTESIAN_POINT('Ctrl Pts',(-55.4039785947519,-107.664464934554,
174.985485069079));
#17039=CARTESIAN_POINT('Ctrl Pts',(-55.4062102741904,-107.684374978846,
175.101539197611));
#17040=CARTESIAN_POINT('Ctrl Pts',(-55.4082754872338,-107.702806195974,
175.217934983052));
#17041=CARTESIAN_POINT('Ctrl Pts',(-55.4101352991462,-107.719408241535,
175.334552884646));
#17042=CARTESIAN_POINT('Ctrl Pts',(-55.4125205153015,-107.740700430823,
175.484115806038));
#17043=CARTESIAN_POINT('Ctrl Pts',(-55.414564175716,-107.758950771819,175.633801866954));
#17044=CARTESIAN_POINT('Ctrl Pts',(-55.416202564948,-107.773584610072,175.784244658626));
#17045=CARTESIAN_POINT('Ctrl Pts',(-55.4168189212164,-107.779089808568,
175.840840707876));
#17046=CARTESIAN_POINT('Ctrl Pts',(-55.4173769391772,-107.784074415306,
175.897450319742));
#17047=CARTESIAN_POINT('Ctrl Pts',(-55.4178742983759,-107.788517451289,
175.954141676001));
#17048=CARTESIAN_POINT('Ctrl Pts',(-55.4179283902715,-107.789000667925,
175.960307326366));
#17049=CARTESIAN_POINT('Ctrl Pts',(-55.4179817602064,-107.789477438801,
175.966473433208));
#17050=CARTESIAN_POINT('Ctrl Pts',(-55.4180344056584,-107.789947741094,
175.972640094678));
#17051=CARTESIAN_POINT('Ctrl Pts',(-55.4180599526251,-107.790175962082,
175.975632556317));
#17052=CARTESIAN_POINT('Ctrl Pts',(-55.4180853288254,-107.790402658372,
175.978625129339));
#17053=CARTESIAN_POINT('Ctrl Pts',(-55.4181105339787,-107.790627827424,
175.981617825086));
#17054=CARTESIAN_POINT('Ctrl Pts',(-55.4181214581951,-107.790725418398,
175.982914895397));
#17055=CARTESIAN_POINT('Ctrl Pts',(-55.4181323593493,-107.7908228035,175.98421311939));
#17056=CARTESIAN_POINT('Ctrl Pts',(-55.418143007908,-107.79091793219,175.985484943039));
#17057=CARTESIAN_POINT('Ctrl Pts',(-55.418151919882,-107.790997547135,175.986549355573));
#17058=CARTESIAN_POINT('Ctrl Pts',(-55.4181606589672,-107.791075617683,
175.987595273717));
#17059=CARTESIAN_POINT('Ctrl Pts',(-55.4181690927828,-107.791150961195,
175.988606543706));
#17060=CARTESIAN_POINT('Ctrl Pts',(-55.4181904567345,-107.791341816108,
175.991168222087));
#17061=CARTESIAN_POINT('Ctrl Pts',(-55.4182117176372,-107.791531751011,
175.993729967309));
#17062=CARTESIAN_POINT('Ctrl Pts',(-55.4182328753062,-107.791720764235,
175.996291784023));
#17063=CARTESIAN_POINT('Ctrl Pts',(-55.4182671838519,-107.792027261554,
176.000445937577));
#17064=CARTESIAN_POINT('Ctrl Pts',(-55.4183012207954,-107.79233133399,176.00460026078));
#17065=CARTESIAN_POINT('Ctrl Pts',(-55.4183349853619,-107.792632974547,
176.008754774191));
#17066=CARTESIAN_POINT('Ctrl Pts',(-55.4184496579914,-107.793657418794,
176.022864506013));
#17067=CARTESIAN_POINT('Ctrl Pts',(-55.4185611841,-107.794653769769,176.036975841278));
#17068=CARTESIAN_POINT('Ctrl Pts',(-55.418669534322,-107.79562176245,176.05108961184));
#17069=CARTESIAN_POINT('Ctrl Pts',(-55.4191639155807,-107.800038527192,
176.115488036934));
#17070=CARTESIAN_POINT('Ctrl Pts',(-55.4195917247742,-107.80386084636,176.179878137561));
#17071=CARTESIAN_POINT('Ctrl Pts',(-55.4199506167913,-107.807067548154,
176.244350243025));
#17072=CARTESIAN_POINT('Ctrl Pts',(-55.4213311808138,-107.819402893928,
176.4923576241));
#17073=CARTESIAN_POINT('Ctrl Pts',(-55.4216681944916,-107.822415133979,
176.73728037898));
#17074=CARTESIAN_POINT('Ctrl Pts',(-55.4209415581552,-107.815922027774,
176.985485069079));
#17075=CARTESIAN_POINT('Ctrl Pts',(-55.4571650701271,-108.140163914373,
174.985485069079));
#17076=CARTESIAN_POINT('Ctrl Pts',(-55.4394801322276,-107.981592323594,
174.985485069079));
#17077=CARTESIAN_POINT('Ctrl Pts',(-55.4217514048672,-107.82302598526,174.985485069079));
#17078=CARTESIAN_POINT('Ctrl Pts',(-55.4039785947519,-107.664464934554,
174.985485069079));
#17079=CARTESIAN_POINT('Origin',(-34.9583934096621,-20.6140499623174,178.485485069079));
#17080=CARTESIAN_POINT('Origin',(-57.7717014757184,-101.417541310487,178.485485069245));
#17081=CARTESIAN_POINT('',(-59.4993129890855,-102.014294800821,178.485485069079));
#17082=CARTESIAN_POINT('',(-43.8144614293464,-103.686404765925,178.485485069079));
#17083=CARTESIAN_POINT('',(-59.520560431892,-102.213601660657,178.485485069079));
#17084=CARTESIAN_POINT('',(-59.4993129890855,-102.014294800821,178.485485069079));
#17085=CARTESIAN_POINT('',(-61.0175785779007,-102.443745017979,178.485485069079));
#17086=CARTESIAN_POINT('Ctrl Pts',(-59.5205604318919,-102.213601660657,
178.485485069079));
#17087=CARTESIAN_POINT('Ctrl Pts',(-59.7687516259883,-102.246139247352,
178.485485069079));
#17088=CARTESIAN_POINT('Ctrl Pts',(-60.0238706481734,-102.283503399127,
178.485485066351));
#17089=CARTESIAN_POINT('Ctrl Pts',(-60.5302050703991,-102.361822081727,
178.485485066351));
#17090=CARTESIAN_POINT('Ctrl Pts',(-60.7757064450282,-102.402354839682,
178.485485069079));
#17091=CARTESIAN_POINT('Ctrl Pts',(-61.0175785779007,-102.443745017979,
178.485485069079));
#17092=CARTESIAN_POINT('',(-61.0705815801248,-102.940927762808,178.485485069079));
#17093=CARTESIAN_POINT('Origin',(-57.9307104902227,-102.909089544544,178.485485069245));
#17094=CARTESIAN_POINT('',(-59.6404105637488,-103.337828874669,178.485485069079));
#17095=CARTESIAN_POINT('Ctrl Pts',(-61.0705815801248,-102.940927762808,
178.485485069079));
#17096=CARTESIAN_POINT('Ctrl Pts',(-60.8351971136389,-103.017001355183,
178.485485069079));
#17097=CARTESIAN_POINT('Ctrl Pts',(-60.5932857657281,-103.091252176655,
178.485485069079));
#17098=CARTESIAN_POINT('Ctrl Pts',(-60.1227897812454,-103.223982772266,
178.485485069079));
#17099=CARTESIAN_POINT('Ctrl Pts',(-59.8821065504266,-103.285479946149,
178.485485069079));
#17100=CARTESIAN_POINT('Ctrl Pts',(-59.6404105637488,-103.337828874669,
178.485485069079));
#17101=CARTESIAN_POINT('',(-59.6795694385642,-103.705149895142,178.485485069079));
#17102=CARTESIAN_POINT('',(-59.4993129890855,-102.014294800821,178.485485069079));
#17103=CARTESIAN_POINT('',(-61.176587584573,-103.935293252465,178.485485069079));
#17104=CARTESIAN_POINT('Ctrl Pts',(-59.6795694385642,-103.705149895142,
178.485485069079));
#17105=CARTESIAN_POINT('Ctrl Pts',(-59.9277575258273,-103.737687074535,
178.485485069079));
#17106=CARTESIAN_POINT('Ctrl Pts',(-60.1828829344089,-103.775052140888,
178.485485066351));
#17107=CARTESIAN_POINT('Ctrl Pts',(-60.6892140770712,-103.853370316212,
178.485485066351));
#17108=CARTESIAN_POINT('Ctrl Pts',(-60.9347154517004,-103.893903074168,
178.485485069079));
#17109=CARTESIAN_POINT('Ctrl Pts',(-61.176587584573,-103.935293252465,178.485485069079));
#17110=CARTESIAN_POINT('',(-61.229590586797,-104.432475997293,178.485485069079));
#17111=CARTESIAN_POINT('Origin',(-58.0897195265028,-104.400637777242,178.485485069234));
#17112=CARTESIAN_POINT('',(-59.7994195704211,-104.829377109155,178.485485069079));
#17113=CARTESIAN_POINT('Ctrl Pts',(-61.229590586797,-104.432475997293,178.485485069079));
#17114=CARTESIAN_POINT('Ctrl Pts',(-60.9942061203117,-104.508549589668,
178.485485069079));
#17115=CARTESIAN_POINT('Ctrl Pts',(-60.7522947724005,-104.58280041114,178.485485069079));
#17116=CARTESIAN_POINT('Ctrl Pts',(-60.281801988239,-104.715530103916,178.485485069079));
#17117=CARTESIAN_POINT('Ctrl Pts',(-60.0411123245086,-104.777028880782,
178.485485069079));
#17118=CARTESIAN_POINT('Ctrl Pts',(-59.7994195704211,-104.829377109155,
178.485485069079));
#17119=CARTESIAN_POINT('',(-59.8385784452364,-105.196698129628,178.485485069079));
#17120=CARTESIAN_POINT('',(-59.4993129890855,-102.014294800821,178.485485069079));
#17121=CARTESIAN_POINT('',(-61.3355965912452,-105.42684148695,178.485485069079));
#17122=CARTESIAN_POINT('Ctrl Pts',(-59.8385784452364,-105.196698129628,
178.485485069079));
#17123=CARTESIAN_POINT('Ctrl Pts',(-60.0867665324994,-105.229235309021,
178.485485069079));
#17124=CARTESIAN_POINT('Ctrl Pts',(-60.3418919410807,-105.266600375374,
178.485485066351));
#17125=CARTESIAN_POINT('Ctrl Pts',(-60.8482230837444,-105.344918550698,
178.485485066351));
#17126=CARTESIAN_POINT('Ctrl Pts',(-61.0937244583751,-105.385451308654,
178.485485069079));
#17127=CARTESIAN_POINT('Ctrl Pts',(-61.3355965912452,-105.42684148695,178.485485069079));
#17128=CARTESIAN_POINT('',(-61.3885995934693,-105.924024231779,178.485485069079));
#17129=CARTESIAN_POINT('Origin',(-58.2487285178737,-105.892186012675,178.48548506924));
#17130=CARTESIAN_POINT('',(-59.9584285770933,-106.32092534364,178.485485069079));
#17131=CARTESIAN_POINT('Ctrl Pts',(-61.3885995934693,-105.924024231779,
178.485485069079));
#17132=CARTESIAN_POINT('Ctrl Pts',(-61.1532151269831,-106.000097824154,
178.485485069079));
#17133=CARTESIAN_POINT('Ctrl Pts',(-60.9113037790725,-106.074348645626,
178.485485069079));
#17134=CARTESIAN_POINT('Ctrl Pts',(-60.4408077945892,-106.207079241237,
178.485485069079));
#17135=CARTESIAN_POINT('Ctrl Pts',(-60.2001245637709,-106.268576415121,
178.485485069079));
#17136=CARTESIAN_POINT('Ctrl Pts',(-59.9584285770933,-106.32092534364,178.485485069079));
#17137=CARTESIAN_POINT('',(-59.9975874519086,-106.688246364113,178.485485069079));
#17138=CARTESIAN_POINT('',(-59.4993129890855,-102.014294800821,178.485485069079));
#17139=CARTESIAN_POINT('',(-61.4946055979174,-106.918389721436,178.485485069079));
#17140=CARTESIAN_POINT('Ctrl Pts',(-59.9975874519086,-106.688246364113,
178.485485069079));
#17141=CARTESIAN_POINT('Ctrl Pts',(-60.2457755391717,-106.720783543507,
178.485485069079));
#17142=CARTESIAN_POINT('Ctrl Pts',(-60.5009009477533,-106.758148609859,
178.485485066351));
#17143=CARTESIAN_POINT('Ctrl Pts',(-61.0072320904167,-106.836466785184,
178.485485066351));
#17144=CARTESIAN_POINT('Ctrl Pts',(-61.2527334650479,-106.876999543139,
178.485485069079));
#17145=CARTESIAN_POINT('Ctrl Pts',(-61.4946055979174,-106.918389721436,
178.485485069079));
#17146=CARTESIAN_POINT('',(-61.5476086001415,-107.415572466264,178.485485069079));
#17147=CARTESIAN_POINT('Origin',(-58.4077375311275,-107.383734246593,178.485485069251));
#17148=CARTESIAN_POINT('',(-60.1174375837655,-107.812473578126,178.485485069079));
#17149=CARTESIAN_POINT('Ctrl Pts',(-61.5476086001415,-107.415572466264,
178.485485069079));
#17150=CARTESIAN_POINT('Ctrl Pts',(-61.3122241336564,-107.49164605864,178.485485069079));
#17151=CARTESIAN_POINT('Ctrl Pts',(-61.0703127857451,-107.565896880111,
178.485485069079));
#17152=CARTESIAN_POINT('Ctrl Pts',(-60.5998168012618,-107.698627475723,
178.485485069079));
#17153=CARTESIAN_POINT('Ctrl Pts',(-60.3591335704432,-107.760124649606,
178.485485069079));
#17154=CARTESIAN_POINT('Ctrl Pts',(-60.1174375837655,-107.812473578126,
178.485485069079));
#17155=CARTESIAN_POINT('',(-60.1565964585809,-108.179794598599,178.485485069079));
#17156=CARTESIAN_POINT('',(-59.4993129890855,-102.014294800821,178.485485069079));
#17157=CARTESIAN_POINT('',(-61.6536146045896,-108.409937955921,178.485485069079));
#17158=CARTESIAN_POINT('Ctrl Pts',(-60.1565964585809,-108.179794598599,
178.485485069079));
#17159=CARTESIAN_POINT('Ctrl Pts',(-60.4047845458449,-108.212331777992,
178.485485069079));
#17160=CARTESIAN_POINT('Ctrl Pts',(-60.6599099544291,-108.249696844346,
178.485485066351));
#17161=CARTESIAN_POINT('Ctrl Pts',(-61.1662410970868,-108.328015019669,
178.485485066351));
#17162=CARTESIAN_POINT('Ctrl Pts',(-61.4117424717138,-108.368547777624,
178.485485069079));
#17163=CARTESIAN_POINT('Ctrl Pts',(-61.6536146045896,-108.409937955921,
178.485485069079));
#17164=CARTESIAN_POINT('',(-61.7066176068137,-108.90712070075,178.485485069079));
#17165=CARTESIAN_POINT('Origin',(-58.5667465453977,-108.875282480713,178.485485069256));
#17166=CARTESIAN_POINT('',(-60.2764465904377,-109.304021812611,178.485485069079));
#17167=CARTESIAN_POINT('Ctrl Pts',(-61.7066176068137,-108.90712070075,178.485485069079));
#17168=CARTESIAN_POINT('Ctrl Pts',(-61.4712331403281,-108.983194293125,
178.485485069079));
#17169=CARTESIAN_POINT('Ctrl Pts',(-61.2293217924171,-109.057445114597,
178.485485069079));
#17170=CARTESIAN_POINT('Ctrl Pts',(-60.7588258079339,-109.190175710208,
178.485485069079));
#17171=CARTESIAN_POINT('Ctrl Pts',(-60.5181425771154,-109.251672884092,
178.485485069079));
#17172=CARTESIAN_POINT('Ctrl Pts',(-60.2764465904377,-109.304021812611,
178.485485069079));
#17173=CARTESIAN_POINT('',(-60.3156054652531,-109.671342833085,178.485485069079));
#17174=CARTESIAN_POINT('',(-59.4993129890855,-102.014294800821,178.485485069079));
#17175=CARTESIAN_POINT('',(-61.8126236112619,-109.901486190407,178.485485069079));
#17176=CARTESIAN_POINT('Ctrl Pts',(-60.3156054652531,-109.671342833085,
178.485485069079));
#17177=CARTESIAN_POINT('Ctrl Pts',(-60.5637966593489,-109.70388041978,178.485485069079));
#17178=CARTESIAN_POINT('Ctrl Pts',(-60.8189156815327,-109.741244571555,
178.485485066351));
#17179=CARTESIAN_POINT('Ctrl Pts',(-61.3252501037601,-109.819563254155,
178.485485066351));
#17180=CARTESIAN_POINT('Ctrl Pts',(-61.5707514783893,-109.86009601211,178.485485069079));
#17181=CARTESIAN_POINT('Ctrl Pts',(-61.8126236112619,-109.901486190407,
178.485485069079));
#17182=CARTESIAN_POINT('',(-61.865626613486,-110.398668935236,178.485485069079));
#17183=CARTESIAN_POINT('Origin',(-58.7257555470878,-110.366830715451,178.485485069251));
#17184=CARTESIAN_POINT('',(-60.43545559711,-110.795570047097,178.485485069079));
#17185=CARTESIAN_POINT('Ctrl Pts',(-61.8656266134859,-110.398668935236,
178.485485069079));
#17186=CARTESIAN_POINT('Ctrl Pts',(-61.6302421469988,-110.474742527611,
178.485485069079));
#17187=CARTESIAN_POINT('Ctrl Pts',(-61.3883307990888,-110.548993349083,
178.485485069079));
#17188=CARTESIAN_POINT('Ctrl Pts',(-60.9178380149293,-110.681723041858,
178.485485069079));
#17189=CARTESIAN_POINT('Ctrl Pts',(-60.677148351198,-110.743221818724,178.485485069079));
#17190=CARTESIAN_POINT('Ctrl Pts',(-60.43545559711,-110.795570047097,178.485485069079));
#17191=CARTESIAN_POINT('',(-60.4746144719253,-111.16289106757,178.485485069079));
#17192=CARTESIAN_POINT('',(-59.4993129890855,-102.014294800821,178.485485069079));
#17193=CARTESIAN_POINT('',(-61.9716326179341,-111.393034424893,178.485485069079));
#17194=CARTESIAN_POINT('Ctrl Pts',(-60.4746144719253,-111.16289106757,178.485485069079));
#17195=CARTESIAN_POINT('Ctrl Pts',(-60.7228025591888,-111.195428246963,
178.485485069079));
#17196=CARTESIAN_POINT('Ctrl Pts',(-60.9779279677714,-111.232793313316,
178.485485066351));
#17197=CARTESIAN_POINT('Ctrl Pts',(-61.4842591104322,-111.31111148864,178.485485066351));
#17198=CARTESIAN_POINT('Ctrl Pts',(-61.7297604850611,-111.351644246595,
178.485485069079));
#17199=CARTESIAN_POINT('Ctrl Pts',(-61.9716326179341,-111.393034424893,
178.485485069079));
#17200=CARTESIAN_POINT('',(-62.0210982548538,-111.802120023171,178.485485069079));
#17201=CARTESIAN_POINT('Ctrl Pts',(-61.9716326179341,-111.393034424893,
178.485485069079));
#17202=CARTESIAN_POINT('Ctrl Pts',(-61.9843448484125,-111.460582087639,
178.485485069079));
#17203=CARTESIAN_POINT('Ctrl Pts',(-61.9948456687939,-111.528527230646,
178.485485069079));
#17204=CARTESIAN_POINT('Ctrl Pts',(-62.0113588747397,-111.665001931148,
178.485485069079));
#17205=CARTESIAN_POINT('Ctrl Pts',(-62.017365779563,-111.733484789515,178.485485069079));
#17206=CARTESIAN_POINT('Ctrl Pts',(-62.0210982548537,-111.802120023171,
178.485485069079));
#17207=CARTESIAN_POINT('',(-62.88786637536,-111.709716750739,178.485485069079));
#17208=CARTESIAN_POINT('',(-53.4413942236179,-112.716773792997,178.485485069079));
#17209=CARTESIAN_POINT('',(-52.5853897920404,-15.069651635714,178.485485069079));
#17210=CARTESIAN_POINT('',(-52.9717383111942,-18.6937070505612,178.485485069079));
#17211=CARTESIAN_POINT('',(-52.5342226896633,-12.3683081541722,178.485485069079));
#17212=CARTESIAN_POINT('Origin',(-67.998054881725,-13.4265585667677,178.485485069079));
#17213=CARTESIAN_POINT('',(-53.9352248596064,8.10403203946808,178.485485069079));
#17214=CARTESIAN_POINT('',(-51.890637311636,-21.772789521366,178.485485069079));
#17215=CARTESIAN_POINT('Origin',(-39.4690592605811,9.0940082318961,178.485485069079));
#17216=CARTESIAN_POINT('',(-25.2666963042872,20.9635176568304,178.485485069079));
#17217=CARTESIAN_POINT('',(-69.5889371886705,15.3762068992854,178.485485069079));
#17218=CARTESIAN_POINT('Ctrl Pts',(-50.7024802268255,-64.597022606232,178.485485069074));
#17219=CARTESIAN_POINT('Ctrl Pts',(-49.9577225357214,-60.5851660064401,
178.485485068971));
#17220=CARTESIAN_POINT('Ctrl Pts',(-49.1559388135441,-56.5870189509198,
178.485485067596));
#17221=CARTESIAN_POINT('Ctrl Pts',(-48.2824671906219,-52.6061072831419,
178.485485067469));
#17222=CARTESIAN_POINT('Ctrl Pts',(-47.5647200183799,-49.3349213424548,
178.485485067364));
#17223=CARTESIAN_POINT('Ctrl Pts',(-46.7984850518727,-46.0753929559384,
178.485485068149));
#17224=CARTESIAN_POINT('Ctrl Pts',(-45.9735869873742,-42.8299680258058,
178.485485068747));
#17225=CARTESIAN_POINT('Ctrl Pts',(-45.7314921849895,-41.8774860878194,
178.485485068923));
#17226=CARTESIAN_POINT('Ctrl Pts',(-45.4843412719279,-40.9262208647867,
178.485485068989));
#17227=CARTESIAN_POINT('Ctrl Pts',(-45.2318774001476,-39.9762334548118,
178.485485069027));
#17228=CARTESIAN_POINT('Ctrl Pts',(-44.5307934654103,-37.3381494127691,
178.485485069132));
#17229=CARTESIAN_POINT('Ctrl Pts',(-43.7882434129997,-34.7100383998247,
178.485485069079));
#17230=CARTESIAN_POINT('Ctrl Pts',(-42.9998272938232,-32.0929433338551,
178.485485069079));
#17231=CARTESIAN_POINT('Ctrl Pts',(-42.536945026492,-30.556436318724,178.485485069079));
#17232=CARTESIAN_POINT('Ctrl Pts',(-42.0582539070797,-29.0237291849288,
178.48548506908));
#17233=CARTESIAN_POINT('Ctrl Pts',(-41.562861354517,-27.4950373025228,178.485485069079));
#17234=CARTESIAN_POINT('Ctrl Pts',(-40.910610725801,-25.4823097468615,178.485485069079));
#17235=CARTESIAN_POINT('Ctrl Pts',(-40.2295198019946,-23.4765157852253,
178.485485069084));
#17236=CARTESIAN_POINT('Ctrl Pts',(-39.5206447744511,-21.477403436665,178.485485069048));
#17237=CARTESIAN_POINT('Ctrl Pts',(-39.5017999516025,-21.4242587826721,
178.485485069047));
#17238=CARTESIAN_POINT('Ctrl Pts',(-39.4829354217113,-21.3711185893304,
178.485485069046));
#17239=CARTESIAN_POINT('Ctrl Pts',(-39.4640512098165,-21.3179828737293,
178.485485069046));
#17240=CARTESIAN_POINT('Ctrl Pts',(-38.8579946469832,-19.6126827351552,
178.485485069021));
#17241=CARTESIAN_POINT('Ctrl Pts',(-38.2315032054965,-17.9121204812206,
178.485485069452));
#17242=CARTESIAN_POINT('Ctrl Pts',(-37.5896039498787,-16.2180717563625,
178.485485068683));
#17243=CARTESIAN_POINT('Ctrl Pts',(-37.4591313137947,-15.8737389021763,
178.485485068526));
#17244=CARTESIAN_POINT('Ctrl Pts',(-37.3280157001481,-15.5296410006451,
178.485485068432));
#17245=CARTESIAN_POINT('Ctrl Pts',(-37.1962973022816,-15.1857911182026,
178.48548506842));
#17246=CARTESIAN_POINT('Ctrl Pts',(-36.6597955345752,-13.7852573071025,
178.485485068374));
#17247=CARTESIAN_POINT('Ctrl Pts',(-36.1130279995534,-12.3883503107043,
178.485485069405));
#17248=CARTESIAN_POINT('Ctrl Pts',(-35.5610537102179,-10.9934715504989,
178.485485068543));
#17249=CARTESIAN_POINT('Ctrl Pts',(-35.3107978101541,-10.3610568776427,
178.485485068152));
#17250=CARTESIAN_POINT('Ctrl Pts',(-35.0594847877249,-9.72903448704139,
178.485485067774));
#17251=CARTESIAN_POINT('Ctrl Pts',(-34.807584751089,-9.09722990883248,178.485485067609));
#17252=CARTESIAN_POINT('Ctrl Pts',(-34.0000823368259,-7.07188791579596,
178.485485067081));
#17253=CARTESIAN_POINT('Ctrl Pts',(-33.1867503081442,-5.04870903840101,
178.485485068358));
#17254=CARTESIAN_POINT('Ctrl Pts',(-32.3920015482318,-3.01863635839204,
178.485485068222));
#17255=CARTESIAN_POINT('Ctrl Pts',(-32.0725147428821,-2.20255275074324,
178.485485068167));
#17256=CARTESIAN_POINT('Ctrl Pts',(-31.7561578556963,-1.38530802264268,
178.485485068002));
#17257=CARTESIAN_POINT('Ctrl Pts',(-31.4446039158297,-0.566281120802405,
178.48548506705));
#17258=CARTESIAN_POINT('Ctrl Pts',(-30.9811424894089,0.652086961355245,
178.485485065634));
#17259=CARTESIAN_POINT('Ctrl Pts',(-30.5284028502065,1.87443509955828,178.485485068243));
#17260=CARTESIAN_POINT('Ctrl Pts',(-30.0917686168577,3.10275613520199,178.485485066804));
#17261=CARTESIAN_POINT('Ctrl Pts',(-29.9026804336469,3.63469104843164,178.485485066181));
#17262=CARTESIAN_POINT('Ctrl Pts',(-29.7166555662945,4.16776221500052,178.485485065225));
#17263=CARTESIAN_POINT('Ctrl Pts',(-29.5339497743812,4.70206521212496,178.485485059336));
#17264=CARTESIAN_POINT('Ctrl Pts',(-29.1679324450908,5.77244264237208,178.48548504754));
#17265=CARTESIAN_POINT('Ctrl Pts',(-28.8155745074676,6.8476686892158,178.485485059056));
#17266=CARTESIAN_POINT('Ctrl Pts',(-28.478719177052,7.92885248014735,178.485485064871));
#17267=CARTESIAN_POINT('Ctrl Pts',(-28.3344155971724,8.39201478589668,178.485485067362));
#17268=CARTESIAN_POINT('Ctrl Pts',(-28.1929573735739,8.85627083216291,178.485485068419));
#17269=CARTESIAN_POINT('Ctrl Pts',(-28.0544916023756,9.32170993752464,178.485485068745));
#17270=CARTESIAN_POINT('Ctrl Pts',(-27.9822645276947,9.56449416305175,178.485485068915));
#17271=CARTESIAN_POINT('Ctrl Pts',(-27.9108481850166,9.80757191347016,178.485485068948));
#17272=CARTESIAN_POINT('Ctrl Pts',(-27.8402559064099,10.0509078082713,178.485485068899));
#17273=CARTESIAN_POINT('Ctrl Pts',(-27.6065126969891,10.8566349237679,178.485485068738));
#17274=CARTESIAN_POINT('Ctrl Pts',(-27.3819521686276,11.6649845310262,178.485485068755));
#17275=CARTESIAN_POINT('Ctrl Pts',(-27.1671077612216,12.4747398429342,178.485485068853));
#17276=CARTESIAN_POINT('Ctrl Pts',(-26.9023082251874,13.4727776019026,178.485485068974));
#17277=CARTESIAN_POINT('Ctrl Pts',(-26.6520104417681,14.4737369620719,178.485485069067));
#17278=CARTESIAN_POINT('Ctrl Pts',(-26.4157730331659,15.4779537724868,178.485485069074));
#17279=CARTESIAN_POINT('Ctrl Pts',(-26.4026358124523,15.5337985176555,178.485485069074));
#17280=CARTESIAN_POINT('Ctrl Pts',(-26.389542235729,15.5896525401592,178.485485069074));
#17281=CARTESIAN_POINT('Ctrl Pts',(-26.3764922522572,15.6455158264978,178.485485069074));
#17282=CARTESIAN_POINT('Ctrl Pts',(-26.0090755642338,17.2183226957897,178.485485069074));
#17283=CARTESIAN_POINT('Ctrl Pts',(-25.6763240448109,18.7984939236132,178.485485068312));
#17284=CARTESIAN_POINT('Ctrl Pts',(-25.3750312441927,20.3853496797055,178.485485068784));
#17285=CARTESIAN_POINT('Ctrl Pts',(-25.3384580343882,20.5779742906419,178.485485068841));
#17286=CARTESIAN_POINT('Ctrl Pts',(-25.3023483140838,20.7706973640245,178.485485068913));
#17287=CARTESIAN_POINT('Ctrl Pts',(-25.2666963042872,20.9635176568304,178.485485068975));
#17288=CARTESIAN_POINT('',(-37.4541011624573,-44.0244753865006,178.485485069079));
#17289=CARTESIAN_POINT('Origin',(-57.4536834643351,-98.4344448420243,178.485485069234));
#17290=CARTESIAN_POINT('Origin',(-57.6126924821839,-99.925993075306,178.485485069234));
#17291=CARTESIAN_POINT('Ctrl Pts',(-56.3380022369383,-103.524730528528,
173.488899497191));
#17292=CARTESIAN_POINT('Ctrl Pts',(-54.948621273746,-103.687204108539,173.583445126328));
#17293=CARTESIAN_POINT('Ctrl Pts',(-54.9486212737461,-103.687204108539,
174.985485069079));
#17294=CARTESIAN_POINT('Ctrl Pts',(-56.3134791922014,-103.315023500967,
173.488899497191));
#17295=CARTESIAN_POINT('Ctrl Pts',(-54.9241403737337,-103.47785747851,173.583445126328));
#17296=CARTESIAN_POINT('Ctrl Pts',(-54.92414037373,-103.477857478511,174.985485069079));
#17297=CARTESIAN_POINT('Ctrl Pts',(-56.2888745073538,-103.105325623786,
173.488899497188));
#17298=CARTESIAN_POINT('Ctrl Pts',(-54.8995781655658,-103.268521622085,
173.583445126281));
#17299=CARTESIAN_POINT('Ctrl Pts',(-54.899578165568,-103.268521622085,174.985485069033));
#17300=CARTESIAN_POINT('Ctrl Pts',(-56.264187433819,-102.895636981445,173.488899497191));
#17301=CARTESIAN_POINT('Ctrl Pts',(-54.8749339071881,-103.059196645868,
173.583445126328));
#17302=CARTESIAN_POINT('Ctrl Pts',(-54.8749339071881,-103.059196645868,
174.985485069079));
#17303=CARTESIAN_POINT('Ctrl Pts',(-56.2951298069877,-103.31239211438,173.490216228525));
#17304=CARTESIAN_POINT('Ctrl Pts',(-56.1168599625939,-103.372824172232,
173.50487235569));
#17305=CARTESIAN_POINT('Ctrl Pts',(-55.9412469787364,-103.427519480035,
173.553480952136));
#17306=CARTESIAN_POINT('Ctrl Pts',(-55.6154923586755,-103.522549593778,
173.714958502574));
#17307=CARTESIAN_POINT('Ctrl Pts',(-55.4681253804373,-103.562403698112,
173.825864100261));
#17308=CARTESIAN_POINT('Ctrl Pts',(-55.3115517495563,-103.602970854155,
173.997534195604));
#17309=CARTESIAN_POINT('Ctrl Pts',(-55.280814671631,-103.610801558914,174.03468048597));
#17310=CARTESIAN_POINT('Ctrl Pts',(-55.2394521645914,-103.621161449704,
174.089882029675));
#17311=CARTESIAN_POINT('Ctrl Pts',(-55.227372087514,-103.624162767105,174.106716353987));
#17312=CARTESIAN_POINT('Ctrl Pts',(-55.2045892632002,-103.629776810059,
174.139889226158));
#17313=CARTESIAN_POINT('Ctrl Pts',(-55.1938496699846,-103.632401432436,
174.156194945232));
#17314=CARTESIAN_POINT('Ctrl Pts',(-55.1053185916828,-103.653854269162,
174.296454686301));
#17315=CARTESIAN_POINT('Ctrl Pts',(-55.0452533006265,-103.667183335149,
174.431403235506));
#17316=CARTESIAN_POINT('Ctrl Pts',(-54.9675549889356,-103.681744085934,
174.707304465526));
#17317=CARTESIAN_POINT('Ctrl Pts',(-54.9481904031526,-103.683519554,174.846067667605));
#17318=CARTESIAN_POINT('Ctrl Pts',(-54.947771193524,-103.67993499333,174.985485069079));
#17319=CARTESIAN_POINT('Ctrl Pts',(-54.8895810276955,-103.183690695995,
174.985485069059));
#17320=CARTESIAN_POINT('Ctrl Pts',(-54.8869443160962,-103.161264788318,
174.853511827955));
#17321=CARTESIAN_POINT('Ctrl Pts',(-54.9019593409972,-103.139808319536,
174.72165986107));
#17322=CARTESIAN_POINT('Ctrl Pts',(-54.9711980898845,-103.096417623673,
174.448996361516));
#17323=CARTESIAN_POINT('Ctrl Pts',(-55.0297082307631,-103.075025668701,
174.310839512231));
#17324=CARTESIAN_POINT('Ctrl Pts',(-55.113651797122,-103.054157978782,174.175160756358));
#17325=CARTESIAN_POINT('Ctrl Pts',(-55.119038710508,-103.052849999777,174.166651653447));
#17326=CARTESIAN_POINT('Ctrl Pts',(-55.1301879436357,-103.050205117004,
174.149436885413));
#17327=CARTESIAN_POINT('Ctrl Pts',(-55.1359564487483,-103.048868971353,
174.140735847771));
#17328=CARTESIAN_POINT('Ctrl Pts',(-55.1544049602056,-103.044695439842,
174.113545908635));
#17329=CARTESIAN_POINT('Ctrl Pts',(-55.1674198033572,-103.041894792854,
174.095282862691));
#17330=CARTESIAN_POINT('Ctrl Pts',(-55.20909085459,-103.033355805697,174.039567190658));
#17331=CARTESIAN_POINT('Ctrl Pts',(-55.2391523612539,-103.027786444963,
174.003181423291));
#17332=CARTESIAN_POINT('Ctrl Pts',(-55.3993921228637,-103.000861959833,
173.827296202087));
#17333=CARTESIAN_POINT('Ctrl Pts',(-55.5542442720682,-102.983503643399,
173.712645716775));
#17334=CARTESIAN_POINT('Ctrl Pts',(-55.8932478530683,-102.957689459523,
173.551401697661));
#17335=CARTESIAN_POINT('Ctrl Pts',(-56.0726931839364,-102.948924353571,
173.503884287599));
#17336=CARTESIAN_POINT('Ctrl Pts',(-56.2564866337797,-102.944965370977,
173.489866571436));
#17337=CARTESIAN_POINT('Ctrl Pts',(-56.4935439071687,-105.015012404135,
173.4901641777));
#17338=CARTESIAN_POINT('Ctrl Pts',(-55.1209916136374,-105.172984763673,
173.59954855975));
#17339=CARTESIAN_POINT('Ctrl Pts',(-55.1209916136374,-105.172984763673,
174.985485069079));
#17340=CARTESIAN_POINT('Ctrl Pts',(-56.469641633236,-104.80733606751,173.490164177706));
#17341=CARTESIAN_POINT('Ctrl Pts',(-55.0971290533058,-104.965653481046,
173.599548559819));
#17342=CARTESIAN_POINT('Ctrl Pts',(-55.0971290532985,-104.965653481047,
174.985485069149));
#17343=CARTESIAN_POINT('Ctrl Pts',(-56.4456610218866,-104.599668529283,
173.4901641777));
#17344=CARTESIAN_POINT('Ctrl Pts',(-55.0731884626156,-104.758332519263,
173.59954855975));
#17345=CARTESIAN_POINT('Ctrl Pts',(-55.0731884626167,-104.758332519263,
174.985485069079));
#17346=CARTESIAN_POINT('Ctrl Pts',(-56.4216013700109,-104.392009869032,
173.4901641777));
#17347=CARTESIAN_POINT('Ctrl Pts',(-55.0491691443755,-104.551021978299,
173.59954855975));
#17348=CARTESIAN_POINT('Ctrl Pts',(-55.0491691443755,-104.551021978299,
174.985485069079));
#17349=CARTESIAN_POINT('Ctrl Pts',(-56.4520785736132,-104.804362764877,
173.491614708057));
#17350=CARTESIAN_POINT('Ctrl Pts',(-56.2764801204879,-104.863475756594,
173.508047709852));
#17351=CARTESIAN_POINT('Ctrl Pts',(-56.1038031321053,-104.916970336167,
173.557406804494));
#17352=CARTESIAN_POINT('Ctrl Pts',(-55.7811932477556,-105.010655798977,
173.719527388766));
#17353=CARTESIAN_POINT('Ctrl Pts',(-55.6343676897392,-105.050165862524,
173.831270860266));
#17354=CARTESIAN_POINT('Ctrl Pts',(-55.4786717532136,-105.090295312868,
174.003823442269));
#17355=CARTESIAN_POINT('Ctrl Pts',(-55.4481316679127,-105.098033854321,
174.041134856339));
#17356=CARTESIAN_POINT('Ctrl Pts',(-55.4071614184955,-105.108237599683,
174.09642283915));
#17357=CARTESIAN_POINT('Ctrl Pts',(-55.3952646257317,-105.111176528091,
174.113183051674));
#17358=CARTESIAN_POINT('Ctrl Pts',(-55.3782751432832,-105.115338825496,
174.138185978057));
#17359=CARTESIAN_POINT('Ctrl Pts',(-55.372919462571,-105.116645561674,174.146232885148));
#17360=CARTESIAN_POINT('Ctrl Pts',(-55.3625173756426,-105.119173055363,
174.162192113799));
#17361=CARTESIAN_POINT('Ctrl Pts',(-55.3574667590035,-105.120395154211,
174.170100905845));
#17362=CARTESIAN_POINT('Ctrl Pts',(-55.2754517253537,-105.140156652778,
174.301203481707));
#17363=CARTESIAN_POINT('Ctrl Pts',(-55.2162337104791,-105.153210404953,
174.435317540761));
#17364=CARTESIAN_POINT('Ctrl Pts',(-55.1396340081755,-105.167422578865,
174.709330975967));
#17365=CARTESIAN_POINT('Ctrl Pts',(-55.1205462794532,-105.169115462503,
174.847088380847));
#17366=CARTESIAN_POINT('Ctrl Pts',(-55.120134291992,-105.165536169417,174.985485069079));
#17367=CARTESIAN_POINT('Ctrl Pts',(-55.0638414339194,-104.677744265774,
174.985485069076));
#17368=CARTESIAN_POINT('Ctrl Pts',(-55.0612613713556,-104.655445553952,
174.854777352187));
#17369=CARTESIAN_POINT('Ctrl Pts',(-55.0759893823669,-104.634087195595,
174.724186106669));
#17370=CARTESIAN_POINT('Ctrl Pts',(-55.1438583050946,-104.590861516158,
174.454137517071));
#17371=CARTESIAN_POINT('Ctrl Pts',(-55.2011654935698,-104.569517652801,
174.317239125928));
#17372=CARTESIAN_POINT('Ctrl Pts',(-55.2889921927481,-104.547221220573,
174.173406546999));
#17373=CARTESIAN_POINT('Ctrl Pts',(-55.3001327143269,-104.544525990686,
174.156002076534));
#17374=CARTESIAN_POINT('Ctrl Pts',(-55.3240161880476,-104.539012928576,
174.120376941088));
#17375=CARTESIAN_POINT('Ctrl Pts',(-55.3368133160102,-104.536201898492,
174.102198371918));
#17376=CARTESIAN_POINT('Ctrl Pts',(-55.3780335382476,-104.527575963677,
174.046393296067));
#17377=CARTESIAN_POINT('Ctrl Pts',(-55.4078751234595,-104.521929130967,
174.009829877401));
#17378=CARTESIAN_POINT('Ctrl Pts',(-55.5673673802023,-104.494548164989,
173.832642158232));
#17379=CARTESIAN_POINT('Ctrl Pts',(-55.7219729516093,-104.476807485154,
173.716842686832));
#17380=CARTESIAN_POINT('Ctrl Pts',(-56.0575151920358,-104.450461151493,
173.555187437059));
#17381=CARTESIAN_POINT('Ctrl Pts',(-56.2331920134854,-104.441405509746,
173.507099973385));
#17382=CARTESIAN_POINT('Ctrl Pts',(-56.4134173387406,-104.436939704692,
173.491276679516));
#17383=CARTESIAN_POINT('Ctrl Pts',(-56.6493388241048,-106.505953769142,
173.491370349032));
#17384=CARTESIAN_POINT('Ctrl Pts',(-55.2907737759503,-106.659861440633,
173.612844366516));
#17385=CARTESIAN_POINT('Ctrl Pts',(-55.2907737759503,-106.659861440633,
174.985485069079));
#17386=CARTESIAN_POINT('Ctrl Pts',(-56.6259915569457,-106.299864099721,
173.491370349032));
#17387=CARTESIAN_POINT('Ctrl Pts',(-55.2674640931904,-106.45410353412,173.612844366521));
#17388=CARTESIAN_POINT('Ctrl Pts',(-55.2674640931895,-106.45410353412,174.985485069085));
#17389=CARTESIAN_POINT('Ctrl Pts',(-56.6025687929303,-106.093782923719,
173.491370349031));
#17390=CARTESIAN_POINT('Ctrl Pts',(-55.2440791994502,-106.248355558005,
173.612844366504));
#17391=CARTESIAN_POINT('Ctrl Pts',(-55.2440791994508,-106.248355558005,
174.985485069068));
#17392=CARTESIAN_POINT('Ctrl Pts',(-56.5790698673243,-105.887710316561,
173.491370349032));
#17393=CARTESIAN_POINT('Ctrl Pts',(-55.2206184354041,-106.042617606657,
173.612844366516));
#17394=CARTESIAN_POINT('Ctrl Pts',(-55.2206184354041,-106.042617606657,
174.985485069079));
#17395=CARTESIAN_POINT('Ctrl Pts',(-56.6091901843102,-106.296300098481,
173.492904904255));
#17396=CARTESIAN_POINT('Ctrl Pts',(-56.4357941643567,-106.354338595723,
173.51075904954));
#17397=CARTESIAN_POINT('Ctrl Pts',(-56.2655234196491,-106.406856990053,
173.560705363963));
#17398=CARTESIAN_POINT('Ctrl Pts',(-55.9455020907631,-106.499444323095,
173.723336101202));
#17399=CARTESIAN_POINT('Ctrl Pts',(-55.7991335388886,-106.53867147263,173.835759261937));
#17400=CARTESIAN_POINT('Ctrl Pts',(-55.644167499606,-106.578442369452,174.009024429013));
#17401=CARTESIAN_POINT('Ctrl Pts',(-55.6137891424861,-106.586105902736,
174.046471025385));
#17402=CARTESIAN_POINT('Ctrl Pts',(-55.5731417121054,-106.596182375197,
174.101826271024));
#17403=CARTESIAN_POINT('Ctrl Pts',(-55.5613960509843,-106.599070390997,
174.118522266282));
#17404=CARTESIAN_POINT('Ctrl Pts',(-55.5392487175406,-106.604470601648,
174.151403158858));
#17405=CARTESIAN_POINT('Ctrl Pts',(-55.5288108760151,-106.606994376912,
174.167556555571));
#17406=CARTESIAN_POINT('Ctrl Pts',(-55.4428037340027,-106.627610764056,
174.306403152543));
#17407=CARTESIAN_POINT('Ctrl Pts',(-55.3845082378286,-106.640382663779,
174.4396024977));
#17408=CARTESIAN_POINT('Ctrl Pts',(-55.3091058140703,-106.654241989031,
174.711549171121));
#17409=CARTESIAN_POINT('Ctrl Pts',(-55.2903198129642,-106.655854262022,
174.848205469326));
#17410=CARTESIAN_POINT('Ctrl Pts',(-55.2899155902427,-106.652286416981,
174.985485069079));
#17411=CARTESIAN_POINT('Ctrl Pts',(-55.2352859196864,-106.171331405706,
174.985485069073));
#17412=CARTESIAN_POINT('Ctrl Pts',(-55.2326665336894,-106.148329373114,
174.851082750799));
#17413=CARTESIAN_POINT('Ctrl Pts',(-55.2483413321261,-106.126315491714,
174.716825828879));
#17414=CARTESIAN_POINT('Ctrl Pts',(-55.3203356455073,-106.081767707275,
174.439384706467));
#17415=CARTESIAN_POINT('Ctrl Pts',(-55.3811169315066,-106.059800227937,
174.299008553436));
#17416=CARTESIAN_POINT('Ctrl Pts',(-55.4681846194273,-106.038387952022,
174.161638426905));
#17417=CARTESIAN_POINT('Ctrl Pts',(-55.4737726492823,-106.037045675612,
174.153023925989));
#17418=CARTESIAN_POINT('Ctrl Pts',(-55.4916498327172,-106.032850156698,
174.126090196313));
#17419=CARTESIAN_POINT('Ctrl Pts',(-55.5042652787232,-106.03003179675,174.107986160937));
#17420=CARTESIAN_POINT('Ctrl Pts',(-55.5451114880963,-106.021335274986,
174.052109135738));
#17421=CARTESIAN_POINT('Ctrl Pts',(-55.5747719738423,-106.015624438621,
174.015396204934));
#17422=CARTESIAN_POINT('Ctrl Pts',(-55.7336532714159,-105.987864066763,
173.837109101904));
#17423=CARTESIAN_POINT('Ctrl Pts',(-55.888067370271,-105.969805160622,173.720342048198));
#17424=CARTESIAN_POINT('Ctrl Pts',(-56.2207366814301,-105.943032892182,
173.558379859302));
#17425=CARTESIAN_POINT('Ctrl Pts',(-56.3932583175807,-105.933753654971,
173.50986981577));
#17426=CARTESIAN_POINT('Ctrl Pts',(-56.5704762085009,-105.92888783639,173.492602186486));
#17427=CARTESIAN_POINT('Ctrl Pts',(-56.8055182225545,-107.997551398667,
173.49242733338));
#17428=CARTESIAN_POINT('Ctrl Pts',(-55.4580190214013,-108.147821158181,
173.623328602317));
#17429=CARTESIAN_POINT('Ctrl Pts',(-55.4580190214013,-108.147821158181,
174.985485069079));
#17430=CARTESIAN_POINT('Ctrl Pts',(-56.782663963309,-107.792612652652,173.49242733338));
#17431=CARTESIAN_POINT('Ctrl Pts',(-55.4352004895909,-107.943202787283,
173.623328602317));
#17432=CARTESIAN_POINT('Ctrl Pts',(-55.4352004895902,-107.943202787283,
174.985485069079));
#17433=CARTESIAN_POINT('Ctrl Pts',(-56.7597366258735,-107.587682138219,
173.49242733338));
#17434=CARTESIAN_POINT('Ctrl Pts',(-55.4123091474965,-107.738594013066,
173.623328602317));
#17435=CARTESIAN_POINT('Ctrl Pts',(-55.4123091475014,-107.738594013066,
174.985485069079));
#17436=CARTESIAN_POINT('Ctrl Pts',(-56.736735577699,-107.382759927281,173.49242733338));
#17437=CARTESIAN_POINT('Ctrl Pts',(-55.3893443675666,-107.533994925185,
173.623328602317));
#17438=CARTESIAN_POINT('Ctrl Pts',(-55.3893443675666,-107.533994925185,
174.985485069079));
#17439=CARTESIAN_POINT('Ctrl Pts',(-56.7665905243134,-107.788178276074,
173.49400046535));
#17440=CARTESIAN_POINT('Ctrl Pts',(-56.5949052326937,-107.845388680746,
173.512938947022));
#17441=CARTESIAN_POINT('Ctrl Pts',(-56.4264957959128,-107.897156142464,
173.56332723609));
#17442=CARTESIAN_POINT('Ctrl Pts',(-56.1084920846803,-107.988893243531,
173.726346578407));
#17443=CARTESIAN_POINT('Ctrl Pts',(-55.9624918596245,-108.027899351649,
173.839287986585));
#17444=CARTESIAN_POINT('Ctrl Pts',(-55.8081013798708,-108.067392125105,
174.013093118869));
#17445=CARTESIAN_POINT('Ctrl Pts',(-55.7778479504432,-108.074998097689,
174.050644783342));
#17446=CARTESIAN_POINT('Ctrl Pts',(-55.7374518773692,-108.084976413728,
174.106049041317));
#17447=CARTESIAN_POINT('Ctrl Pts',(-55.7258247337975,-108.087824947824,
174.122691724583));
#17448=CARTESIAN_POINT('Ctrl Pts',(-55.7039020480952,-108.093150795867,
174.155461392321));
#17449=CARTESIAN_POINT('Ctrl Pts',(-55.6935706101721,-108.095639569752,
174.17155735823));
#17450=CARTESIAN_POINT('Ctrl Pts',(-55.608443919145,-108.115967969813,174.309888289955));
#17451=CARTESIAN_POINT('Ctrl Pts',(-55.5507627722578,-108.12854889235,174.442461042842));
#17452=CARTESIAN_POINT('Ctrl Pts',(-55.4761499414694,-108.142169695467,
174.713017710041));
#17453=CARTESIAN_POINT('Ctrl Pts',(-55.4575623940107,-108.143726509878,
174.848944909728));
#17454=CARTESIAN_POINT('Ctrl Pts',(-55.4571650701274,-108.140163914373,
174.985485069079));
#17455=CARTESIAN_POINT('Ctrl Pts',(-55.4039785948117,-107.664464934563,
174.985485069077));
#17456=CARTESIAN_POINT('Ctrl Pts',(-55.4014083953031,-107.641534765974,
174.851826866554));
#17457=CARTESIAN_POINT('Ctrl Pts',(-55.4169241878019,-107.619574533909,
174.718312672541));
#17458=CARTESIAN_POINT('Ctrl Pts',(-55.4881074621261,-107.575119044012,
174.442449886533));
#17459=CARTESIAN_POINT('Ctrl Pts',(-55.5481519170216,-107.553177440629,
174.30284539021));
#17460=CARTESIAN_POINT('Ctrl Pts',(-55.6341776305828,-107.531750474155,
174.166061967665));
#17461=CARTESIAN_POINT('Ctrl Pts',(-55.6397004507487,-107.53040670336,174.157481019746));
#17462=CARTESIAN_POINT('Ctrl Pts',(-55.6573708437641,-107.526205542954,
174.130647331335));
#17463=CARTESIAN_POINT('Ctrl Pts',(-55.669841458162,-107.523382361785,174.112605920834));
#17464=CARTESIAN_POINT('Ctrl Pts',(-55.7103922997075,-107.514630979822,
174.056672899912));
#17465=CARTESIAN_POINT('Ctrl Pts',(-55.7399114236766,-107.508869519605,
174.019839086604));
#17466=CARTESIAN_POINT('Ctrl Pts',(-55.8983246981518,-107.480807006229,
173.840659718242));
#17467=CARTESIAN_POINT('Ctrl Pts',(-56.0526068341962,-107.462494558611,
173.723111091821));
#17468=CARTESIAN_POINT('Ctrl Pts',(-56.3830049352595,-107.435395780513,
173.560934379101));
#17469=CARTESIAN_POINT('Ctrl Pts',(-56.5529996701729,-107.425951563239,
173.512127246035));
#17470=CARTESIAN_POINT('Ctrl Pts',(-56.7277951555015,-107.420782694947,
173.49375276819));
#17471=CARTESIAN_POINT('Ctrl Pts',(-56.9621866626637,-109.489802972882,
173.493261648264));
#17472=CARTESIAN_POINT('Ctrl Pts',(-55.6227768443799,-109.636849320768,
173.631005581965));
#17473=CARTESIAN_POINT('Ctrl Pts',(-55.6227768443799,-109.636849320768,
174.985485069079));
#17474=CARTESIAN_POINT('Ctrl Pts',(-56.9397670005278,-109.285587662391,
173.493261648264));
#17475=CARTESIAN_POINT('Ctrl Pts',(-55.6003912981915,-109.432944764224,
173.631005581965));
#17476=CARTESIAN_POINT('Ctrl Pts',(-55.600391298188,-109.432944764224,174.985485069079));
#17477=CARTESIAN_POINT('Ctrl Pts',(-56.9172762923776,-109.081380361356,
173.49326164826));
#17478=CARTESIAN_POINT('Ctrl Pts',(-55.5779349587329,-109.22904952246,173.63100558192));
#17479=CARTESIAN_POINT('Ctrl Pts',(-55.5779349587373,-109.229049522459,
174.985485069034));
#17480=CARTESIAN_POINT('Ctrl Pts',(-56.8947139323498,-108.87718113875,173.493261648264));
#17481=CARTESIAN_POINT('Ctrl Pts',(-55.5554072248064,-109.025163681204,
173.631005581965));
#17482=CARTESIAN_POINT('Ctrl Pts',(-55.5554072248065,-109.025163681204,
174.98548506908));
#17483=CARTESIAN_POINT('Ctrl Pts',(-56.9243786881308,-109.279976942607,
173.494832944154));
#17484=CARTESIAN_POINT('Ctrl Pts',(-56.7538963361861,-109.336606160927,
173.514535334738));
#17485=CARTESIAN_POINT('Ctrl Pts',(-56.5867932277359,-109.387847708036,
173.565235192448));
#17486=CARTESIAN_POINT('Ctrl Pts',(-56.2702263316121,-109.478982732056,
173.728531078916));
#17487=CARTESIAN_POINT('Ctrl Pts',(-56.1245025623703,-109.517830055776,
173.841827344492));
#17488=CARTESIAN_POINT('Ctrl Pts',(-55.972216810626,-109.556695013004,174.014088641704));
#17489=CARTESIAN_POINT('Ctrl Pts',(-55.9435627449903,-109.563888754681,
174.049643091631));
#17490=CARTESIAN_POINT('Ctrl Pts',(-55.9044952972728,-109.573534138044,
174.102920514733));
#17491=CARTESIAN_POINT('Ctrl Pts',(-55.8927880988003,-109.576400871192,
174.119583578313));
#17492=CARTESIAN_POINT('Ctrl Pts',(-55.8707107628622,-109.581761653968,
174.152400753911));
#17493=CARTESIAN_POINT('Ctrl Pts',(-55.8603047098438,-109.584267172477,
174.16852362561));
#17494=CARTESIAN_POINT('Ctrl Pts',(-55.7745081060717,-109.604745566871,
174.307181765745));
#17495=CARTESIAN_POINT('Ctrl Pts',(-55.7163483209697,-109.617424971451,
174.440179457196));
#17496=CARTESIAN_POINT('Ctrl Pts',(-55.6410802083126,-109.631163216239,
174.711792204332));
#17497=CARTESIAN_POINT('Ctrl Pts',(-55.6223253405858,-109.632736702427,
174.848327690676));
#17498=CARTESIAN_POINT('Ctrl Pts',(-55.6219312570821,-109.629147380551,
174.985485069079));
#17499=CARTESIAN_POINT('Ctrl Pts',(-55.5699812776884,-109.157156757033,
174.985485069059));
#17500=CARTESIAN_POINT('Ctrl Pts',(-55.5675435745271,-109.135063848326,
174.856923057509));
#17501=CARTESIAN_POINT('Ctrl Pts',(-55.5818331979452,-109.113860418937,
174.728474891724));
#17502=CARTESIAN_POINT('Ctrl Pts',(-55.6474497152721,-109.070906537188,
174.463007451237));
#17503=CARTESIAN_POINT('Ctrl Pts',(-55.7027062177817,-109.049644761822,
174.328376230069));
#17504=CARTESIAN_POINT('Ctrl Pts',(-55.7874222731387,-109.027317500699,
174.18644210645));
#17505=CARTESIAN_POINT('Ctrl Pts',(-55.7981757523871,-109.0246146387,174.169247570115));
#17506=CARTESIAN_POINT('Ctrl Pts',(-55.8212392669884,-109.019079357439,
174.134020636803));
#17507=CARTESIAN_POINT('Ctrl Pts',(-55.8336024294317,-109.016253407579,
174.1160283696));
#17508=CARTESIAN_POINT('Ctrl Pts',(-55.8739377468614,-109.007462323059,
174.060054071408));
#17509=CARTESIAN_POINT('Ctrl Pts',(-55.9033558416481,-109.001663505812,
174.023128360552));
#17510=CARTESIAN_POINT('Ctrl Pts',(-56.0614490778147,-108.97337593563,173.843266153729));
#17511=CARTESIAN_POINT('Ctrl Pts',(-56.2156626186106,-108.954874796232,
173.725124931942));
#17512=CARTESIAN_POINT('Ctrl Pts',(-56.5444000502588,-108.927543158314,
173.562816682292));
#17513=CARTESIAN_POINT('Ctrl Pts',(-56.7125053750529,-108.917985710097,
173.513819867409));
#17514=CARTESIAN_POINT('Ctrl Pts',(-56.8854801878217,-108.912602509009,
173.494655322398));
#17515=CARTESIAN_POINT('Ctrl Pts',(-57.1194187443674,-110.982706994464,
173.493819516807));
#17516=CARTESIAN_POINT('Ctrl Pts',(-55.7850950242185,-111.12692947585,173.63589097676));
#17517=CARTESIAN_POINT('Ctrl Pts',(-55.7850950242185,-111.12692947585,174.98548506908));
#17518=CARTESIAN_POINT('Ctrl Pts',(-57.097378700238,-110.778795971744,173.493819516803));
#17519=CARTESIAN_POINT('Ctrl Pts',(-55.7630877058362,-110.923321226614,
173.635890976726));
#17520=CARTESIAN_POINT('Ctrl Pts',(-55.7630877058354,-110.923321226614,
174.985485069045));
#17521=CARTESIAN_POINT('Ctrl Pts',(-57.0752692869159,-110.574892773011,
173.493819516808));
#17522=CARTESIAN_POINT('Ctrl Pts',(-55.7410112583161,-110.719722057746,
173.635890976772));
#17523=CARTESIAN_POINT('Ctrl Pts',(-55.7410112583178,-110.719722057746,
174.985485069091));
#17524=CARTESIAN_POINT('Ctrl Pts',(-57.0530899203455,-110.370997464803,
173.493819516807));
#17525=CARTESIAN_POINT('Ctrl Pts',(-55.7188651019731,-110.51613205175,173.63589097676));
#17526=CARTESIAN_POINT('Ctrl Pts',(-55.7188651019731,-110.51613205175,174.985485069079));
#17527=CARTESIAN_POINT('Ctrl Pts',(-57.0826240442755,-110.77168183954,173.495354125426));
#17528=CARTESIAN_POINT('Ctrl Pts',(-56.9128280627272,-110.827975820923,
173.515513471879));
#17529=CARTESIAN_POINT('Ctrl Pts',(-56.7464720083201,-110.878915152489,
173.566405745216));
#17530=CARTESIAN_POINT('Ctrl Pts',(-56.4307568142368,-110.969695233241,
173.729873488259));
#17531=CARTESIAN_POINT('Ctrl Pts',(-56.2852156383961,-111.008446018537,
173.843360765196));
#17532=CARTESIAN_POINT('Ctrl Pts',(-56.1332269225956,-111.047185085229,
174.015760442495));
#17533=CARTESIAN_POINT('Ctrl Pts',(-56.1046589569938,-111.05434781301,174.05130245406));
#17534=CARTESIAN_POINT('Ctrl Pts',(-56.0657248932361,-111.063947318451,
174.104535558086));
#17535=CARTESIAN_POINT('Ctrl Pts',(-56.0540665026745,-111.06679822698,174.121170947796));
#17536=CARTESIAN_POINT('Ctrl Pts',(-56.0320806105947,-111.072129489664,
174.153932246034));
#17537=CARTESIAN_POINT('Ctrl Pts',(-56.0217173672487,-111.074621245229,
174.170027146221));
#17538=CARTESIAN_POINT('Ctrl Pts',(-55.9362556453455,-111.094991086755,
174.308465969329));
#17539=CARTESIAN_POINT('Ctrl Pts',(-55.8783248745144,-111.107599808822,
174.441208052489));
#17540=CARTESIAN_POINT('Ctrl Pts',(-55.8033352673517,-111.121252864932,
174.712299263541));
#17541=CARTESIAN_POINT('Ctrl Pts',(-55.7846493192605,-111.122805905128,
174.848582874691));
#17542=CARTESIAN_POINT('Ctrl Pts',(-55.7842612734033,-111.119216054728,
174.985485069078));
#17543=CARTESIAN_POINT('Ctrl Pts',(-55.7333536027297,-110.649417900359,
174.985485069077));
#17544=CARTESIAN_POINT('Ctrl Pts',(-55.7309690326988,-110.627465945723,
174.857863999367));
#17545=CARTESIAN_POINT('Ctrl Pts',(-55.7450628622825,-110.606386714262,
174.730354705224));
#17546=CARTESIAN_POINT('Ctrl Pts',(-55.8097005466027,-110.563683118527,
174.466889269619));
#17547=CARTESIAN_POINT('Ctrl Pts',(-55.8640743698788,-110.542533757114,
174.333251213159));
#17548=CARTESIAN_POINT('Ctrl Pts',(-55.959278319169,-110.517133998281,174.172148090414));
#17549=CARTESIAN_POINT('Ctrl Pts',(-55.9829900909391,-110.511413156019,
174.135807737448));
#17550=CARTESIAN_POINT('Ctrl Pts',(-56.0358028832275,-110.499830988273,
174.062235482721));
#17551=CARTESIAN_POINT('Ctrl Pts',(-56.0651604927824,-110.494007937226,
174.025247036739));
#17552=CARTESIAN_POINT('Ctrl Pts',(-56.2230849566472,-110.465571830551,
173.844911894683));
#17553=CARTESIAN_POINT('Ctrl Pts',(-56.3772962272133,-110.446946615986,
173.726368205424));
#17554=CARTESIAN_POINT('Ctrl Pts',(-56.704987133118,-110.419471069408,173.564004403809));
#17555=CARTESIAN_POINT('Ctrl Pts',(-56.871843629646,-110.409846826172,173.514911464148));
#17556=CARTESIAN_POINT('Ctrl Pts',(-57.043608201862,-110.40433147521,173.495256480951));
#17557=CARTESIAN_POINT('Ctrl Pts',(-57.0822389279392,-110.649056444086,
178.477039335021));
#17558=CARTESIAN_POINT('Ctrl Pts',(-55.7490106450711,-110.793662661806,
178.334126158632));
#17559=CARTESIAN_POINT('Ctrl Pts',(-55.7490106450711,-110.793662661806,
176.985485069079));
#17560=CARTESIAN_POINT('Ctrl Pts',(-57.1044155270742,-110.853518393605,
178.477039335021));
#17561=CARTESIAN_POINT('Ctrl Pts',(-55.7711541904733,-110.997819865288,
178.334126158632));
#17562=CARTESIAN_POINT('Ctrl Pts',(-55.7711541904754,-110.997819865288,
176.985485069079));
#17563=CARTESIAN_POINT('Ctrl Pts',(-57.126522089051,-111.057988548884,178.477039335021));
#17564=CARTESIAN_POINT('Ctrl Pts',(-55.793227942238,-111.201986545103,178.334126158632));
#17565=CARTESIAN_POINT('Ctrl Pts',(-55.7932279422347,-111.201986545103,
176.985485069079));
#17566=CARTESIAN_POINT('Ctrl Pts',(-57.1485591984125,-111.26246684077,178.477039335021));
#17567=CARTESIAN_POINT('Ctrl Pts',(-55.8152324805442,-111.406162616148,
178.334126158632));
#17568=CARTESIAN_POINT('Ctrl Pts',(-55.8152324805442,-111.406162616148,
176.985485069079));
#17569=CARTESIAN_POINT('',(-57.1318490822761,-111.234741954516,178.475522296093));
#17570=CARTESIAN_POINT('Ctrl Pts',(-55.8006548129686,-111.270994369076,
176.985485069082));
#17571=CARTESIAN_POINT('Ctrl Pts',(-55.8030222309522,-111.292930279278,
177.113081070041));
#17572=CARTESIAN_POINT('Ctrl Pts',(-55.8212991787659,-111.31054480159,177.240557658034));
#17573=CARTESIAN_POINT('Ctrl Pts',(-55.8935168729266,-111.338617326837,
177.503776803771));
#17574=CARTESIAN_POINT('Ctrl Pts',(-55.9510512132407,-111.347819958795,
177.637222406408));
#17575=CARTESIAN_POINT('Ctrl Pts',(-56.0492820653997,-111.352596896656,
177.798114695378));
#17576=CARTESIAN_POINT('Ctrl Pts',(-56.0736131933765,-111.353196783989,
177.834404081079));
#17577=CARTESIAN_POINT('Ctrl Pts',(-56.1276211701236,-111.353403281168,
177.907968380396));
#17578=CARTESIAN_POINT('Ctrl Pts',(-56.1575481140501,-111.352916066103,
177.944995033058));
#17579=CARTESIAN_POINT('Ctrl Pts',(-56.3180516517131,-111.347464517362,
178.125655363643));
#17580=CARTESIAN_POINT('Ctrl Pts',(-56.4729341378883,-111.333173910538,
178.244439479484));
#17581=CARTESIAN_POINT('Ctrl Pts',(-56.7988031792984,-111.29103742598,178.406700803439));
#17582=CARTESIAN_POINT('Ctrl Pts',(-56.9633576095936,-111.265401839379,
178.455737245865));
#17583=CARTESIAN_POINT('Ctrl Pts',(-57.1318490822761,-111.234741954516,
178.475522296092));
#17584=CARTESIAN_POINT('',(-57.0927973172532,-110.86741985642,178.475593938758));
#17585=CARTESIAN_POINT('',(-57.1318490822761,-111.234741954516,178.475522296093));
#17586=CARTESIAN_POINT('Ctrl Pts',(-57.0927973172543,-110.867419856423,
178.475593938747));
#17587=CARTESIAN_POINT('Ctrl Pts',(-56.9147592776452,-110.848167673894,
178.455404659106));
#17588=CARTESIAN_POINT('Ctrl Pts',(-56.7412161395771,-110.833424542233,
178.404457924272));
#17589=CARTESIAN_POINT('Ctrl Pts',(-56.413411971825,-110.811230540968,178.240940728206));
#17590=CARTESIAN_POINT('Ctrl Pts',(-56.2630572878917,-110.80402401403,178.12756038466));
#17591=CARTESIAN_POINT('Ctrl Pts',(-56.1062997177754,-110.79818089641,177.95525199714));
#17592=CARTESIAN_POINT('Ctrl Pts',(-56.0768080828725,-110.797196991731,
177.919660793991));
#17593=CARTESIAN_POINT('Ctrl Pts',(-56.0366890993698,-110.796016297223,
177.866398529148));
#17594=CARTESIAN_POINT('Ctrl Pts',(-56.0247049838097,-110.795686419516,
177.849788446774));
#17595=CARTESIAN_POINT('Ctrl Pts',(-56.0021106664059,-110.795108182657,
177.81707364697));
#17596=CARTESIAN_POINT('Ctrl Pts',(-55.9914633711863,-110.794856233593,
177.800999769791));
#17597=CARTESIAN_POINT('Ctrl Pts',(-55.9036287919606,-110.792951291756,
177.662641392075));
#17598=CARTESIAN_POINT('Ctrl Pts',(-55.8443255099797,-110.792830832311,
177.529959747674));
#17599=CARTESIAN_POINT('Ctrl Pts',(-55.76806551622,-110.795283517144,177.258846135829));
#17600=CARTESIAN_POINT('Ctrl Pts',(-55.7494490397083,-110.797704553748,
177.122475998923));
#17601=CARTESIAN_POINT('Ctrl Pts',(-55.7498389523166,-110.801299724063,
176.98548506908));
#17602=CARTESIAN_POINT('Ctrl Pts',(-56.9232540372578,-109.154004151255,
178.477503703266));
#17603=CARTESIAN_POINT('Ctrl Pts',(-55.5858787857402,-109.301345064959,
178.338149647288));
#17604=CARTESIAN_POINT('Ctrl Pts',(-55.5858787857403,-109.301345064959,
176.985485069079));
#17605=CARTESIAN_POINT('Ctrl Pts',(-56.9458762959346,-109.359340524723,
178.477503703266));
#17606=CARTESIAN_POINT('Ctrl Pts',(-55.6084665105141,-109.506367983156,
178.338149647288));
#17607=CARTESIAN_POINT('Ctrl Pts',(-55.6084665105118,-109.506367983157,
176.985485069079));
#17608=CARTESIAN_POINT('Ctrl Pts',(-56.968426419469,-109.564685347002,178.477503703266));
#17609=CARTESIAN_POINT('Ctrl Pts',(-55.6309823578394,-109.7114006768,178.338149647288));
#17610=CARTESIAN_POINT('Ctrl Pts',(-55.630982357837,-109.711400676801,176.985485069079));
#17611=CARTESIAN_POINT('Ctrl Pts',(-56.9909050192882,-109.770038545797,
178.477503703266));
#17612=CARTESIAN_POINT('Ctrl Pts',(-55.6534269344576,-109.916443056728,
178.338149647288));
#17613=CARTESIAN_POINT('Ctrl Pts',(-55.6534269344576,-109.916443056728,
176.985485069079));
#17614=CARTESIAN_POINT('',(-56.9734652393652,-109.7431874274,178.475940356875));
#17615=CARTESIAN_POINT('Ctrl Pts',(-55.6385532353225,-109.78066106394,176.985485069082));
#17616=CARTESIAN_POINT('Ctrl Pts',(-55.6409594189848,-109.802611489716,
177.11336531854));
#17617=CARTESIAN_POINT('Ctrl Pts',(-55.6593416836102,-109.820220945236,
177.24112020221));
#17618=CARTESIAN_POINT('Ctrl Pts',(-55.7318960116661,-109.848235538582,
177.504810124576));
#17619=CARTESIAN_POINT('Ctrl Pts',(-55.7896567465906,-109.857385583657,
177.638440485888));
#17620=CARTESIAN_POINT('Ctrl Pts',(-55.8882344934935,-109.862070690011,
177.799495074151));
#17621=CARTESIAN_POINT('Ctrl Pts',(-55.9126451019893,-109.862647764504,
177.835811023265));
#17622=CARTESIAN_POINT('Ctrl Pts',(-55.9667916934297,-109.862803717785,
177.909375509078));
#17623=CARTESIAN_POINT('Ctrl Pts',(-55.9967740152662,-109.862289944981,
177.946377912396));
#17624=CARTESIAN_POINT('Ctrl Pts',(-56.1575492729998,-109.85670279429,178.126897146243));
#17625=CARTESIAN_POINT('Ctrl Pts',(-56.3126249340782,-109.842303243046,
178.245523765821));
#17626=CARTESIAN_POINT('Ctrl Pts',(-56.6392348626847,-109.799895618343,
178.407624573229));
#17627=CARTESIAN_POINT('Ctrl Pts',(-56.804403867627,-109.774067823015,178.4565096845));
#17628=CARTESIAN_POINT('Ctrl Pts',(-56.9734652393652,-109.7431874274,178.475940356874));
#17629=CARTESIAN_POINT('',(-56.9345361076167,-109.375864092667,178.476093934548));
#17630=CARTESIAN_POINT('',(-56.9734652393652,-109.7431874274,178.475940356875));
#17631=CARTESIAN_POINT('Ctrl Pts',(-56.9345361076177,-109.37586409267,178.476093934536));
#17632=CARTESIAN_POINT('Ctrl Pts',(-56.7555615318508,-109.356409036724,
178.456331596915));
#17633=CARTESIAN_POINT('Ctrl Pts',(-56.5810328056178,-109.341507923764,
178.405522603758));
#17634=CARTESIAN_POINT('Ctrl Pts',(-56.2522717149334,-109.319133494151,
178.242127257605));
#17635=CARTESIAN_POINT('Ctrl Pts',(-56.1018037389524,-109.311861568565,
178.129046621873));
#17636=CARTESIAN_POINT('Ctrl Pts',(-55.9447093653116,-109.305940907224,
177.956969033457));
#17637=CARTESIAN_POINT('Ctrl Pts',(-55.9150694097991,-109.304939856116,
177.921314909201));
#17638=CARTESIAN_POINT('Ctrl Pts',(-55.8747729217627,-109.303737332467,
177.867978487055));
#17639=CARTESIAN_POINT('Ctrl Pts',(-55.8627515212982,-109.303401425641,
177.851366853639));
#17640=CARTESIAN_POINT('Ctrl Pts',(-55.840083744564,-109.302811767932,177.818644194178));
#17641=CARTESIAN_POINT('Ctrl Pts',(-55.8294003481997,-109.302554418962,
177.802564065397));
#17642=CARTESIAN_POINT('Ctrl Pts',(-55.7412161662989,-109.300603909226,
177.664069577128));
#17643=CARTESIAN_POINT('Ctrl Pts',(-55.6816569414381,-109.300454409692,
177.531194877827));
#17644=CARTESIAN_POINT('Ctrl Pts',(-55.6050255745782,-109.302871854621,
177.259535984071));
#17645=CARTESIAN_POINT('Ctrl Pts',(-55.5863131000029,-109.305287236401,
177.122823740951));
#17646=CARTESIAN_POINT('Ctrl Pts',(-55.5867097138724,-109.308887482778,
176.985485069079));
#17647=CARTESIAN_POINT('Ctrl Pts',(-56.7646390135495,-107.658044645611,
178.47825681256));
#17648=CARTESIAN_POINT('Ctrl Pts',(-55.4201132624748,-107.808520799227,
178.344956154987));
#17649=CARTESIAN_POINT('Ctrl Pts',(-55.4201132624748,-107.808520799227,
176.985485069079));
#17650=CARTESIAN_POINT('Ctrl Pts',(-56.7877654331416,-107.864682481035,
178.478256812562));
#17651=CARTESIAN_POINT('Ctrl Pts',(-55.4432034350782,-108.014834762672,
178.34495615501));
#17652=CARTESIAN_POINT('Ctrl Pts',(-55.4432034350741,-108.014834762673,
176.985485069102));
#17653=CARTESIAN_POINT('Ctrl Pts',(-56.8108172327237,-108.071329050187,
178.478256812557));
#17654=CARTESIAN_POINT('Ctrl Pts',(-55.4662192622098,-108.221158854215,
178.344956154953));
#17655=CARTESIAN_POINT('Ctrl Pts',(-55.4662192622078,-108.221158854215,
176.985485069045));
#17656=CARTESIAN_POINT('Ctrl Pts',(-56.8337950559789,-108.277984277046,
178.47825681256));
#17657=CARTESIAN_POINT('Ctrl Pts',(-55.4891613824828,-108.427492979837,
178.344956154987));
#17658=CARTESIAN_POINT('Ctrl Pts',(-55.4891613824828,-108.427492979837,
176.98548506908));
#17659=CARTESIAN_POINT('',(-56.8155634335305,-108.251628031083,178.476680214078));
#17660=CARTESIAN_POINT('Ctrl Pts',(-55.4740061171911,-108.291289155992,
176.985485069082));
#17661=CARTESIAN_POINT('Ctrl Pts',(-55.4764658987439,-108.313379911227,
177.114480114835));
#17662=CARTESIAN_POINT('Ctrl Pts',(-55.4951767887661,-108.33105141348,177.24333814957));
#17663=CARTESIAN_POINT('Ctrl Pts',(-55.5689898174003,-108.359032051728,
177.509171060714));
#17664=CARTESIAN_POINT('Ctrl Pts',(-55.6277353931126,-108.368063831478,
177.6437815552));
#17665=CARTESIAN_POINT('Ctrl Pts',(-55.7154894664664,-108.371922802339,
177.785651423283));
#17666=CARTESIAN_POINT('Ctrl Pts',(-55.7265931139023,-108.372284875476,
177.802828744998));
#17667=CARTESIAN_POINT('Ctrl Pts',(-55.7503497799542,-108.372807237009,
177.838021307392));
#17668=CARTESIAN_POINT('Ctrl Pts',(-55.7630532947064,-108.372950036688,
177.855996422835));
#17669=CARTESIAN_POINT('Ctrl Pts',(-55.804450631013,-108.372999404612,177.911981060336));
#17670=CARTESIAN_POINT('Ctrl Pts',(-55.8345248860353,-108.372437876787,
177.948929958811));
#17671=CARTESIAN_POINT('Ctrl Pts',(-55.9957097052851,-108.366608583803,
178.129104713902));
#17672=CARTESIAN_POINT('Ctrl Pts',(-56.1510382185471,-108.35202200111,178.247387779987));
#17673=CARTESIAN_POINT('Ctrl Pts',(-56.4789706596083,-108.309128697421,
178.409249582182));
#17674=CARTESIAN_POINT('Ctrl Pts',(-56.6453603770763,-108.282932908725,
178.457893915397));
#17675=CARTESIAN_POINT('Ctrl Pts',(-56.8155634335305,-108.251628031083,
178.476680214078));
#17676=CARTESIAN_POINT('',(-56.7767448738944,-107.884303575429,178.476907478761));
#17677=CARTESIAN_POINT('',(-56.8155634335305,-108.251628031083,178.476680214078));
#17678=CARTESIAN_POINT('Ctrl Pts',(-56.7767448738954,-107.884303575432,
178.476907478748));
#17679=CARTESIAN_POINT('Ctrl Pts',(-56.5962729667804,-107.864513578287,
178.457879613496));
#17680=CARTESIAN_POINT('Ctrl Pts',(-56.4201604123224,-107.849352852162,
178.407328813957));
#17681=CARTESIAN_POINT('Ctrl Pts',(-56.0898126794775,-107.826678692935,
178.244160776659));
#17682=CARTESIAN_POINT('Ctrl Pts',(-55.9391249447214,-107.819299905284,
178.131544466062));
#17683=CARTESIAN_POINT('Ctrl Pts',(-55.7814712700151,-107.813254304601,
177.959821319822));
#17684=CARTESIAN_POINT('Ctrl Pts',(-55.7516010922104,-107.812225889799,
177.924078918995));
#17685=CARTESIAN_POINT('Ctrl Pts',(-55.7110190459911,-107.81098815467,177.870628909897));
#17686=CARTESIAN_POINT('Ctrl Pts',(-55.6989308113585,-107.810642364463,
177.854006513428));
#17687=CARTESIAN_POINT('Ctrl Pts',(-55.6761329314457,-107.810034054685,
177.821255733448));
#17688=CARTESIAN_POINT('Ctrl Pts',(-55.6653863067212,-107.809767916626,
177.805158398335));
#17689=CARTESIAN_POINT('Ctrl Pts',(-55.5766160932854,-107.807743752311,
177.666411573885));
#17690=CARTESIAN_POINT('Ctrl Pts',(-55.5166331037104,-107.807547831138,
177.533195240923));
#17691=CARTESIAN_POINT('Ctrl Pts',(-55.4394039866848,-107.809908992442,
177.260632619921));
#17692=CARTESIAN_POINT('Ctrl Pts',(-55.4205378716355,-107.812314749534,
177.123376449463));
#17693=CARTESIAN_POINT('Ctrl Pts',(-55.4209415581552,-107.815922027774,
176.98548506908));
#17694=CARTESIAN_POINT('Ctrl Pts',(-56.6063169754422,-106.161159974594,
178.479251376));
#17695=CARTESIAN_POINT('Ctrl Pts',(-55.2516552698864,-106.315188128166,
178.354564947683));
#17696=CARTESIAN_POINT('Ctrl Pts',(-55.2516552698864,-106.315188128166,
176.985485069079));
#17697=CARTESIAN_POINT('Ctrl Pts',(-56.6300126762584,-106.369561216403,
178.479251375997));
#17698=CARTESIAN_POINT('Ctrl Pts',(-55.2753127466082,-106.523253193008,
178.354564947649));
#17699=CARTESIAN_POINT('Ctrl Pts',(-55.2753127466048,-106.523253193008,
176.985485069044));
#17700=CARTESIAN_POINT('Ctrl Pts',(-56.6536308295825,-106.577971524729,
178.479251376));
#17701=CARTESIAN_POINT('Ctrl Pts',(-55.2988929703655,-106.731328799967,
178.354564947683));
#17702=CARTESIAN_POINT('Ctrl Pts',(-55.2988929703647,-106.731328799967,
176.985485069079));
#17703=CARTESIAN_POINT('Ctrl Pts',(-56.6771721177013,-106.786390819126,
178.479251376));
#17704=CARTESIAN_POINT('Ctrl Pts',(-55.3223966179213,-106.939414849226,
178.354564947683));
#17705=CARTESIAN_POINT('Ctrl Pts',(-55.3223966179213,-106.939414849226,
176.985485069079));
#17706=CARTESIAN_POINT('',(-56.6580826427064,-106.760064354331,178.477700244368));
#17707=CARTESIAN_POINT('Ctrl Pts',(-55.3069657209396,-106.802898527557,
176.985485069082));
#17708=CARTESIAN_POINT('Ctrl Pts',(-55.3095589298666,-106.825823912651,
177.119764397273));
#17709=CARTESIAN_POINT('Ctrl Pts',(-55.329756417029,-106.843953781154,177.253864484605));
#17710=CARTESIAN_POINT('Ctrl Pts',(-55.4096086469019,-106.87214148342,177.530214923199));
#17711=CARTESIAN_POINT('Ctrl Pts',(-55.4732767885331,-106.880780792608,
177.669761195188));
#17712=CARTESIAN_POINT('Ctrl Pts',(-55.5621868299431,-106.883447490003,
177.806441021704));
#17713=CARTESIAN_POINT('Ctrl Pts',(-55.5678844737477,-106.883587748771,
177.815010837929));
#17714=CARTESIAN_POINT('Ctrl Pts',(-55.5860916690433,-106.883941267773,
177.841809516667));
#17715=CARTESIAN_POINT('Ctrl Pts',(-55.5989085506571,-106.884053392005,
177.859827009987));
#17716=CARTESIAN_POINT('Ctrl Pts',(-55.6405535382393,-106.884002227609,
177.915774224524));
#17717=CARTESIAN_POINT('Ctrl Pts',(-55.6707558780194,-106.883371657133,
177.952640181471));
#17718=CARTESIAN_POINT('Ctrl Pts',(-55.8324857653739,-106.877193480759,
178.132266860809));
#17719=CARTESIAN_POINT('Ctrl Pts',(-55.988124979762,-106.86234169041,178.250020609912));
#17720=CARTESIAN_POINT('Ctrl Pts',(-56.3179590299471,-106.81874460688,178.411558382723));
#17721=CARTESIAN_POINT('Ctrl Pts',(-56.4861730086404,-106.792001449029,
178.459861811937));
#17722=CARTESIAN_POINT('Ctrl Pts',(-56.6580826427064,-106.760064354331,
178.477700244367));
#17723=CARTESIAN_POINT('',(-56.6193547970192,-106.392738970839,178.477987698341));
#17724=CARTESIAN_POINT('',(-56.6580826427064,-106.760064354331,178.477700244368));
#17725=CARTESIAN_POINT('Ctrl Pts',(-56.6193547970202,-106.392738970842,
178.477987698327));
#17726=CARTESIAN_POINT('Ctrl Pts',(-56.4368347272708,-106.372479290791,
178.460016009567));
#17727=CARTESIAN_POINT('Ctrl Pts',(-56.2585452960474,-106.356954969072,
178.409857125584));
#17728=CARTESIAN_POINT('Ctrl Pts',(-55.9259821398569,-106.33385926111,178.247031357291));
#17729=CARTESIAN_POINT('Ctrl Pts',(-55.7749667750593,-106.326331504666,
178.135042067197));
#17730=CARTESIAN_POINT('Ctrl Pts',(-55.6165302667828,-106.320112685004,
177.963795620031));
#17731=CARTESIAN_POINT('Ctrl Pts',(-55.5863473744548,-106.319046346214,
177.927940434316));
#17732=CARTESIAN_POINT('Ctrl Pts',(-55.5453711490126,-106.317759594012,
177.874338528708));
#17733=CARTESIAN_POINT('Ctrl Pts',(-55.5331865443366,-106.31739996492,177.857696549508));
#17734=CARTESIAN_POINT('Ctrl Pts',(-55.515785173297,-106.316919677115,177.832865301265));
#17735=CARTESIAN_POINT('Ctrl Pts',(-55.5102973815779,-106.316773369357,
177.824869653524));
#17736=CARTESIAN_POINT('Ctrl Pts',(-55.4943714687919,-106.316363895439,
177.801173623749));
#17737=CARTESIAN_POINT('Ctrl Pts',(-55.4841525646855,-106.316120843354,
177.785328044534));
#17738=CARTESIAN_POINT('Ctrl Pts',(-55.3998699166634,-106.314282856012,
177.649024294688));
#17739=CARTESIAN_POINT('Ctrl Pts',(-55.3430285159645,-106.314163697371,
177.518809435036));
#17740=CARTESIAN_POINT('Ctrl Pts',(-55.2699140586195,-106.31654102514,177.253130960667));
#17741=CARTESIAN_POINT('Ctrl Pts',(-55.2520765286572,-106.318893063481,
177.119599537937));
#17742=CARTESIAN_POINT('Ctrl Pts',(-55.2524742173427,-106.322390962095,
176.985485069079));
#17743=CARTESIAN_POINT('Ctrl Pts',(-56.4481805239386,-104.663337987308,
178.480419827436));
#17744=CARTESIAN_POINT('Ctrl Pts',(-55.0804443419474,-104.821348467162,
178.366983319731));
#17745=CARTESIAN_POINT('Ctrl Pts',(-55.0804443419474,-104.821348467162,
176.98548506908));
#17746=CARTESIAN_POINT('Ctrl Pts',(-56.4725158438094,-104.873984126249,
178.480419827432));
#17747=CARTESIAN_POINT('Ctrl Pts',(-55.1047391646424,-105.031644063198,
178.366983319684));
#17748=CARTESIAN_POINT('Ctrl Pts',(-55.1047391646466,-105.031644063197,
176.985485069032));
#17749=CARTESIAN_POINT('Ctrl Pts',(-56.4967701946591,-105.084639717741,
178.480419827436));
#17750=CARTESIAN_POINT('Ctrl Pts',(-55.1289533365054,-105.241950684034,
178.366983319731));
#17751=CARTESIAN_POINT('Ctrl Pts',(-55.1289533365085,-105.241950684034,
176.985485069079));
#17752=CARTESIAN_POINT('Ctrl Pts',(-56.5209443047536,-105.295304676109,
178.480419827436));
#17753=CARTESIAN_POINT('Ctrl Pts',(-55.1530875797156,-105.452268222959,
178.366983319731));
#17754=CARTESIAN_POINT('Ctrl Pts',(-55.1530875797156,-105.452268222959,
176.985485069079));
#17755=CARTESIAN_POINT('',(-56.5009308898174,-105.268497296389,178.478938088823));
#17756=CARTESIAN_POINT('Ctrl Pts',(-55.1373829400717,-105.315510127364,
176.985485069083));
#17757=CARTESIAN_POINT('Ctrl Pts',(-55.139935036767,-105.337717924091,177.116060375578));
#17758=CARTESIAN_POINT('Ctrl Pts',(-55.1591285187234,-105.355388783739,
177.246478394228));
#17759=CARTESIAN_POINT('Ctrl Pts',(-55.2347312636371,-105.383111126789,
177.515243096824));
#17760=CARTESIAN_POINT('Ctrl Pts',(-55.2948363692995,-105.391860549335,
177.65114778878));
#17761=CARTESIAN_POINT('Ctrl Pts',(-55.3845226483519,-105.39524301998,177.794070257923));
#17762=CARTESIAN_POINT('Ctrl Pts',(-55.3958619777939,-105.395543966573,
177.811358415504));
#17763=CARTESIAN_POINT('Ctrl Pts',(-55.4201164687611,-105.395934349373,
177.846761528336));
#17764=CARTESIAN_POINT('Ctrl Pts',(-55.4330826876001,-105.396005988558,
177.864835189548));
#17765=CARTESIAN_POINT('Ctrl Pts',(-55.475048770948,-105.395822915869,177.920729993758));
#17766=CARTESIAN_POINT('Ctrl Pts',(-55.5054144853479,-105.395102052341,
177.95748353685));
#17767=CARTESIAN_POINT('Ctrl Pts',(-55.6678208283352,-105.388468834203,
178.136360265097));
#17768=CARTESIAN_POINT('Ctrl Pts',(-55.8238259562453,-105.373274146514,
178.253401157095));
#17769=CARTESIAN_POINT('Ctrl Pts',(-56.1561325155399,-105.328751722564,
178.414520859981));
#17770=CARTESIAN_POINT('Ctrl Pts',(-56.3267651109123,-105.301278060031,
178.462368244637));
#17771=CARTESIAN_POINT('Ctrl Pts',(-56.5009308898174,-105.268497296389,
178.478938088822));
#17772=CARTESIAN_POINT('',(-56.462266632785,-104.901171252502,178.479267413549));
#17773=CARTESIAN_POINT('',(-56.5009308898174,-105.268497296389,178.478938088823));
#17774=CARTESIAN_POINT('Ctrl Pts',(-56.4622666327859,-104.901171252505,
178.479267413534));
#17775=CARTESIAN_POINT('Ctrl Pts',(-56.2771642179805,-104.880304301774,
178.46269045673));
#17776=CARTESIAN_POINT('Ctrl Pts',(-56.0961152238312,-104.864309854259,
178.413073717723));
#17777=CARTESIAN_POINT('Ctrl Pts',(-55.7607146838184,-104.840668369511,
178.250716473028));
#17778=CARTESIAN_POINT('Ctrl Pts',(-55.6092642890516,-104.832949042415,
178.139513891316));
#17779=CARTESIAN_POINT('Ctrl Pts',(-55.4486812284957,-104.82646180254,177.967642939846));
#17780=CARTESIAN_POINT('Ctrl Pts',(-55.4170806160678,-104.825313937519,
177.930322194352));
#17781=CARTESIAN_POINT('Ctrl Pts',(-55.3748234624629,-104.823951063456,
177.875140746089));
#17782=CARTESIAN_POINT('Ctrl Pts',(-55.3626241599256,-104.823580554528,
177.85850795651));
#17783=CARTESIAN_POINT('Ctrl Pts',(-55.3452002756585,-104.823084593115,
177.83368874429));
#17784=CARTESIAN_POINT('Ctrl Pts',(-55.3397048128954,-104.822933313132,
177.825696206482));
#17785=CARTESIAN_POINT('Ctrl Pts',(-55.3290289750007,-104.822649521151,
177.809840195386));
#17786=CARTESIAN_POINT('Ctrl Pts',(-55.3238443417221,-104.822516596407,
177.801980167301));
#17787=CARTESIAN_POINT('Ctrl Pts',(-55.2393275090736,-104.820430490539,
177.671169918897));
#17788=CARTESIAN_POINT('Ctrl Pts',(-55.1784777690603,-104.820106204412,
177.537275226144));
#17789=CARTESIAN_POINT('Ctrl Pts',(-55.1000138889637,-104.822301340755,
177.262882339598));
#17790=CARTESIAN_POINT('Ctrl Pts',(-55.0808280652764,-104.824669959404,
177.124510689081));
#17791=CARTESIAN_POINT('Ctrl Pts',(-55.0812452693716,-104.828281539026,
176.985485069079));
#17792=CARTESIAN_POINT('Ctrl Pts',(-56.2900948296076,-103.164573183438,
178.481676597204));
#17793=CARTESIAN_POINT('Ctrl Pts',(-54.9064184039505,-103.327007356746,
178.382209459588));
#17794=CARTESIAN_POINT('Ctrl Pts',(-54.9064184039505,-103.327007356746,
176.985485069079));
#17795=CARTESIAN_POINT('Ctrl Pts',(-56.315136870002,-103.377890863102,178.481676597204));
#17796=CARTESIAN_POINT('Ctrl Pts',(-54.9314173573655,-103.53995800504,178.382209459588));
#17797=CARTESIAN_POINT('Ctrl Pts',(-54.9314173573688,-103.539958005039,
176.985485069079));
#17798=CARTESIAN_POINT('Ctrl Pts',(-56.3400940264076,-103.591218433758,
178.481676597204));
#17799=CARTESIAN_POINT('Ctrl Pts',(-54.9563317726869,-103.752920229724,
178.382209459588));
#17800=CARTESIAN_POINT('Ctrl Pts',(-54.9563317726919,-103.752920229724,
176.985485069079));
#17801=CARTESIAN_POINT('Ctrl Pts',(-56.3649670808697,-103.80455580367,178.481676597204));
#17802=CARTESIAN_POINT('Ctrl Pts',(-54.9811624251918,-103.965893916035,
178.382209459588));
#17803=CARTESIAN_POINT('Ctrl Pts',(-54.9811624251918,-103.965893916035,
176.985485069079));
#17804=CARTESIAN_POINT('',(-56.343987871522,-103.776928050381,178.480312727066));
#17805=CARTESIAN_POINT('Ctrl Pts',(-54.9652072511181,-103.82914600553,176.985485069083));
#17806=CARTESIAN_POINT('Ctrl Pts',(-54.9678127841589,-103.851461015716,
177.117296539967));
#17807=CARTESIAN_POINT('Ctrl Pts',(-54.9873706365605,-103.869145711318,
177.248936771374));
#17808=CARTESIAN_POINT('Ctrl Pts',(-55.064373529731,-103.896698018697,177.520046945381));
#17809=CARTESIAN_POINT('Ctrl Pts',(-55.1255699889516,-103.90523950117,177.657007192595));
#17810=CARTESIAN_POINT('Ctrl Pts',(-55.2110381744666,-103.908065861991,
177.791675329049));
#17811=CARTESIAN_POINT('Ctrl Pts',(-55.2165132019378,-103.908217279327,
177.800118301497));
#17812=CARTESIAN_POINT('Ctrl Pts',(-55.2278316868487,-103.908471032756,
177.817203493515));
#17813=CARTESIAN_POINT('Ctrl Pts',(-55.2336809623173,-103.908571361852,
177.82584119157));
#17814=CARTESIAN_POINT('Ctrl Pts',(-55.2523681669576,-103.908796662826,
177.852841814393));
#17815=CARTESIAN_POINT('Ctrl Pts',(-55.2655194584768,-103.908817732493,
177.870984653547));
#17816=CARTESIAN_POINT('Ctrl Pts',(-55.307878468054,-103.908471243195,177.926811129217));
#17817=CARTESIAN_POINT('Ctrl Pts',(-55.3384414676804,-103.907638988345,
177.963422725913));
#17818=CARTESIAN_POINT('Ctrl Pts',(-55.5016508194093,-103.900445816394,
178.141351970913));
#17819=CARTESIAN_POINT('Ctrl Pts',(-55.6580750812902,-103.884831359886,
178.257501037053));
#17820=CARTESIAN_POINT('Ctrl Pts',(-55.9934121427347,-103.839158416831,
178.418096294027));
#17821=CARTESIAN_POINT('Ctrl Pts',(-56.1670410556707,-103.810767352649,
178.465352870717));
#17822=CARTESIAN_POINT('Ctrl Pts',(-56.343987871522,-103.776928050381,178.480312727065));
#17823=CARTESIAN_POINT('',(-56.3053536374455,-103.40960168206,178.480661415526));
#17824=CARTESIAN_POINT('',(-56.343987871522,-103.776928050381,178.480312727066));
#17825=CARTESIAN_POINT('Ctrl Pts',(-56.3053536374462,-103.409601682063,
178.480661415514));
#17826=CARTESIAN_POINT('Ctrl Pts',(-56.1171541463156,-103.387986491668,
178.46583662156));
#17827=CARTESIAN_POINT('Ctrl Pts',(-55.9327747632696,-103.371412441811,
178.41693017353));
#17828=CARTESIAN_POINT('Ctrl Pts',(-55.5939279603077,-103.347098934845,
178.255178416131));
#17829=CARTESIAN_POINT('Ctrl Pts',(-55.4419403876366,-103.339145250376,
178.144919795626));
#17830=CARTESIAN_POINT('Ctrl Pts',(-55.280402017082,-103.332395517122,177.974063117867));
#17831=CARTESIAN_POINT('Ctrl Pts',(-55.2485609792392,-103.331193876366,
177.936905101778));
#17832=CARTESIAN_POINT('Ctrl Pts',(-55.1679090691248,-103.328475257935,
177.832858015124));
#17833=CARTESIAN_POINT('Ctrl Pts',(-55.1227396789694,-103.327318672735,
177.763371477236));
#17834=CARTESIAN_POINT('Ctrl Pts',(-55.024038606154,-103.325685197287,177.579627296491));
#17835=CARTESIAN_POINT('Ctrl Pts',(-54.9788266623195,-103.325876624763,
177.461694894587));
#17836=CARTESIAN_POINT('Ctrl Pts',(-54.9208912318742,-103.328342249097,
177.223551059475));
#17837=CARTESIAN_POINT('Ctrl Pts',(-54.9068282367496,-103.330498483767,
177.104719966844));
#17838=CARTESIAN_POINT('Ctrl Pts',(-54.9071900358704,-103.333580645004,
176.985485069079));
#17839=CARTESIAN_POINT('Origin',(-57.8503443722502,-102.190085871961,175.985485069079));
#17840=CARTESIAN_POINT('Ctrl Pts',(-60.4746144719253,-111.16289106757,178.485485069079));
#17841=CARTESIAN_POINT('Ctrl Pts',(-59.7173985122241,-111.170711378967,
178.985485106928));
#17842=CARTESIAN_POINT('Ctrl Pts',(-58.8107269732545,-111.198740106278,
178.985485069079));
#17843=CARTESIAN_POINT('Ctrl Pts',(-57.8942367159207,-111.227072368185,
178.985485030821));
#17844=CARTESIAN_POINT('Ctrl Pts',(-57.1318490822761,-111.234741954516,
178.475522296093));
#17845=CARTESIAN_POINT('Ctrl Pts',(-57.0927973172532,-110.86741985642,178.475593938758));
#17846=CARTESIAN_POINT('Ctrl Pts',(-57.8551481998615,-110.85974917265,178.985485030824));
#17847=CARTESIAN_POINT('Ctrl Pts',(-58.7715680984392,-110.831419085805,
178.985485069079));
#17848=CARTESIAN_POINT('Ctrl Pts',(-59.6782396374026,-110.803390358494,
178.985485106928));
#17849=CARTESIAN_POINT('Ctrl Pts',(-60.43545559711,-110.795570047097,178.485485069079));
#17850=CARTESIAN_POINT('Origin',(-57.8503443722502,-102.190085871961,175.985485069079));
#17851=CARTESIAN_POINT('Ctrl Pts',(-60.3156054652531,-109.671342833085,
178.485485069079));
#17852=CARTESIAN_POINT('Ctrl Pts',(-59.5583895055519,-109.679163144481,
178.985485106928));
#17853=CARTESIAN_POINT('Ctrl Pts',(-58.6517179665823,-109.707191871792,
178.985485069079));
#17854=CARTESIAN_POINT('Ctrl Pts',(-57.7356383282381,-109.735511439877,
178.985485030838));
#17855=CARTESIAN_POINT('Ctrl Pts',(-56.9734652393652,-109.7431874274,178.475940356875));
#17856=CARTESIAN_POINT('Ctrl Pts',(-56.9345361076167,-109.375864092667,
178.476093934548));
#17857=CARTESIAN_POINT('Ctrl Pts',(-57.6966303278291,-109.368185755292,
178.985485030845));
#17858=CARTESIAN_POINT('Ctrl Pts',(-58.612559091767,-109.339870851319,178.985485069079));
#17859=CARTESIAN_POINT('Ctrl Pts',(-59.5192306307304,-109.311842124008,
178.985485106928));
#17860=CARTESIAN_POINT('Ctrl Pts',(-60.2764465904377,-109.304021812611,
178.485485069079));
#17861=CARTESIAN_POINT('Origin',(-57.8503443722502,-102.190085871961,175.985485069079));
#17862=CARTESIAN_POINT('Ctrl Pts',(-60.1565964585809,-108.179794598599,
178.485485069079));
#17863=CARTESIAN_POINT('Ctrl Pts',(-59.3993804988796,-108.187614909996,
178.985485106928));
#17864=CARTESIAN_POINT('Ctrl Pts',(-58.4927089599101,-108.215643637307,
178.985485069079));
#17865=CARTESIAN_POINT('Ctrl Pts',(-57.5773563068175,-108.243940731463,
178.985485030869));
#17866=CARTESIAN_POINT('Ctrl Pts',(-56.8155634335305,-108.251628031083,
178.476680214078));
#17867=CARTESIAN_POINT('Ctrl Pts',(-56.7767448738943,-107.884303575429,
178.476907478761));
#17868=CARTESIAN_POINT('Ctrl Pts',(-57.5384208193584,-107.876612805222,
178.985485030878));
#17869=CARTESIAN_POINT('Ctrl Pts',(-58.4535500850947,-107.848322616834,
178.985485069079));
#17870=CARTESIAN_POINT('Ctrl Pts',(-59.3602216240582,-107.820293889523,
178.985485106928));
#17871=CARTESIAN_POINT('Ctrl Pts',(-60.1174375837655,-107.812473578126,
178.485485069079));
#17872=CARTESIAN_POINT('Origin',(-57.8503443722502,-102.190085871961,175.985485069079));
#17873=CARTESIAN_POINT('Ctrl Pts',(-59.9975874519086,-106.688246364113,
178.485485069079));
#17874=CARTESIAN_POINT('Ctrl Pts',(-59.2403714922074,-106.69606667551,178.985485106928));
#17875=CARTESIAN_POINT('Ctrl Pts',(-58.3336999532379,-106.724095402821,
178.985485069079));
#17876=CARTESIAN_POINT('Ctrl Pts',(-57.4193502102051,-106.752361493145,
178.98548503091));
#17877=CARTESIAN_POINT('Ctrl Pts',(-56.6580826427064,-106.760064354331,
178.477700244368));
#17878=CARTESIAN_POINT('Ctrl Pts',(-56.6193547970191,-106.392738970839,
178.477987698341));
#17879=CARTESIAN_POINT('Ctrl Pts',(-57.3804740961378,-106.385031731442,
178.985485030922));
#17880=CARTESIAN_POINT('Ctrl Pts',(-58.2945410784225,-106.356774382348,
178.985485069079));
#17881=CARTESIAN_POINT('Ctrl Pts',(-59.201212617386,-106.328745655037,178.985485106928));
#17882=CARTESIAN_POINT('Ctrl Pts',(-59.9584285770933,-106.32092534364,178.485485069079));
#17883=CARTESIAN_POINT('Origin',(-57.8503443722502,-102.190085871961,175.985485069079));
#17884=CARTESIAN_POINT('Ctrl Pts',(-59.8385784452364,-105.196698129628,
178.485485069079));
#17885=CARTESIAN_POINT('Ctrl Pts',(-59.0813624855352,-105.204518441025,
178.985485106928));
#17886=CARTESIAN_POINT('Ctrl Pts',(-58.1746909465656,-105.232547168336,
178.985485069079));
#17887=CARTESIAN_POINT('Ctrl Pts',(-57.2615592502346,-105.26077560412,178.985485030961));
#17888=CARTESIAN_POINT('Ctrl Pts',(-56.5009308898174,-105.268497296389,
178.478938088823));
#17889=CARTESIAN_POINT('Ctrl Pts',(-56.462266632785,-104.901171252502,178.479267413548));
#17890=CARTESIAN_POINT('Ctrl Pts',(-57.2227246142167,-104.89344456017,178.985485030975));
#17891=CARTESIAN_POINT('Ctrl Pts',(-58.1355320717503,-104.865226147862,
178.985485069079));
#17892=CARTESIAN_POINT('Ctrl Pts',(-59.0422036107137,-104.837197420552,
178.985485106928));
#17893=CARTESIAN_POINT('Ctrl Pts',(-59.7994195704211,-104.829377109155,
178.485485069079));
#17894=CARTESIAN_POINT('Origin',(-57.8503443722502,-102.190085871961,175.985485069079));
#17895=CARTESIAN_POINT('Ctrl Pts',(-59.6795694385642,-103.705149895142,
178.485485069079));
#17896=CARTESIAN_POINT('Ctrl Pts',(-58.922353478863,-103.712970206539,178.985485106928));
#17897=CARTESIAN_POINT('Ctrl Pts',(-58.0156819398934,-103.74099893385,178.985485069079));
#17898=CARTESIAN_POINT('Ctrl Pts',(-57.1039041585715,-103.76918551488,178.985485031018));
#17899=CARTESIAN_POINT('Ctrl Pts',(-56.343987871522,-103.776928050381,178.480312727066));
#17900=CARTESIAN_POINT('Ctrl Pts',(-56.3053536374455,-103.40960168206,178.480661415526));
#17901=CARTESIAN_POINT('Ctrl Pts',(-57.0650889275684,-103.401853871046,
178.985485031032));
#17902=CARTESIAN_POINT('Ctrl Pts',(-57.9765230650781,-103.373677913377,
178.985485069079));
#17903=CARTESIAN_POINT('Ctrl Pts',(-58.8831946040415,-103.345649186066,
178.985485106928));
#17904=CARTESIAN_POINT('Ctrl Pts',(-59.6404105637488,-103.337828874669,
178.485485069079));
#17905=CARTESIAN_POINT('Origin',(-57.8503443722502,-102.190085871961,175.985485069079));
#17906=CARTESIAN_POINT('',(-57.1028900759218,-102.269769493613,178.889785775842));
#17907=CARTESIAN_POINT('Ctrl Pts',(-59.5205604318919,-102.213601660657,
178.485485069079));
#17908=CARTESIAN_POINT('Ctrl Pts',(-58.7633444721907,-102.221421972053,
178.985485106928));
#17909=CARTESIAN_POINT('Ctrl Pts',(-57.8566729332212,-102.249450699364,
178.985485069079));
#17910=CARTESIAN_POINT('Ctrl Pts',(-57.4738337760053,-102.261285739818,
178.985485053098));
#17911=CARTESIAN_POINT('Ctrl Pts',(-57.1028900759218,-102.269769493613,
178.889785775842));
#17912=CARTESIAN_POINT('Origin',(-57.8503443722502,-102.190085871961,175.985485069079));
#17913=CARTESIAN_POINT('Origin',(-57.8503443722502,-102.190085871961,175.985485069079));
#17914=CARTESIAN_POINT('Ctrl Pts',(-53.872882413622,-102.614109889754,175.985485078249));
#17915=CARTESIAN_POINT('Ctrl Pts',(-53.9451038903198,-102.606410597834,
176.390205984865));
#17916=CARTESIAN_POINT('Ctrl Pts',(-54.0841826712686,-102.591583870614,
176.77982118409));
#17917=CARTESIAN_POINT('Ctrl Pts',(-54.4695645888159,-102.550499583507,
177.466598590891));
#17918=CARTESIAN_POINT('Ctrl Pts',(-54.7036701793867,-102.525542363518,
177.764282984435));
#17919=CARTESIAN_POINT('Ctrl Pts',(-55.2319645793612,-102.469222651002,
178.254741908794));
#17920=CARTESIAN_POINT('Ctrl Pts',(-55.5765915421303,-102.432483114354,
178.512021649406));
#17921=CARTESIAN_POINT('Ctrl Pts',(-56.3676195021526,-102.348154249042,
178.819447246742));
#17922=CARTESIAN_POINT('Ctrl Pts',(-56.7334438797843,-102.309154926352,
178.888970429676));
#17923=CARTESIAN_POINT('Ctrl Pts',(-57.1028900759218,-102.269769493613,
178.889785775842));
#17924=CARTESIAN_POINT('Ctrl Pts',(-51.366074883876,-77.3517457257593,176.985485069079));
#17925=CARTESIAN_POINT('Ctrl Pts',(-51.366074883876,-77.3517457257593,174.585485069075));
#17926=CARTESIAN_POINT('Ctrl Pts',(-48.8928953354189,-61.7130539582536,
176.985485069079));
#17927=CARTESIAN_POINT('Ctrl Pts',(-48.8928953354189,-61.7130539582536,
174.585485069075));
#17928=CARTESIAN_POINT('Ctrl Pts',(-46.2601081177707,-49.5877530345566,
176.985485069079));
#17929=CARTESIAN_POINT('Ctrl Pts',(-46.2601081177707,-49.5877530345566,
174.585485069075));
#17930=CARTESIAN_POINT('Ctrl Pts',(-40.9615423766251,-29.8520086479652,
176.985485069079));
#17931=CARTESIAN_POINT('Ctrl Pts',(-40.9615423766251,-29.8520086479652,
174.585485069075));
#17932=CARTESIAN_POINT('Ctrl Pts',(-38.2937855838775,-22.2407276361426,
176.985485069079));
#17933=CARTESIAN_POINT('Ctrl Pts',(-38.2937855838775,-22.2407276361426,
174.585485069075));
#17934=CARTESIAN_POINT('Ctrl Pts',(-34.518838241635,-12.3909742448081,176.985485069079));
#17935=CARTESIAN_POINT('Ctrl Pts',(-34.518838241635,-12.3909742448081,174.585485069075));
#17936=CARTESIAN_POINT('Ctrl Pts',(-33.2992245946195,-9.36991678274843,
176.985485069079));
#17937=CARTESIAN_POINT('Ctrl Pts',(-33.2992245946195,-9.36991678274843,
174.585485069075));
#17938=CARTESIAN_POINT('Ctrl Pts',(-30.9798899307116,-3.54783868987816,
176.985485069079));
#17939=CARTESIAN_POINT('Ctrl Pts',(-30.9798899307116,-3.54783868987816,
174.585485069075));
#17940=CARTESIAN_POINT('Ctrl Pts',(-29.8803502640751,-0.747159372776982,
176.985485069079));
#17941=CARTESIAN_POINT('Ctrl Pts',(-29.8803502640751,-0.747159372776982,
174.585485069075));
#17942=CARTESIAN_POINT('Ctrl Pts',(-26.8076803368812,7.8043162165179,176.985485069079));
#17943=CARTESIAN_POINT('Ctrl Pts',(-26.8076803368812,7.8043162165179,174.585485069075));
#17944=CARTESIAN_POINT('Ctrl Pts',(-25.0550914662622,13.705075012501,176.985485069079));
#17945=CARTESIAN_POINT('Ctrl Pts',(-25.0550914662622,13.705075012501,174.585485069075));
#17946=CARTESIAN_POINT('Ctrl Pts',(-23.70581036359,21.1602846666598,176.985485069079));
#17947=CARTESIAN_POINT('Ctrl Pts',(-23.70581036359,21.1602846666598,174.585485069075));
#17948=CARTESIAN_POINT('',(-23.7058173975717,21.1602848469763,176.985485069079));
#17949=CARTESIAN_POINT('Ctrl Pts',(-23.7058173975717,21.1602848469763,176.985485069079));
#17950=CARTESIAN_POINT('Ctrl Pts',(-24.0609786331059,19.1981320867072,176.985485069079));
#17951=CARTESIAN_POINT('Ctrl Pts',(-24.4622947014093,17.2457191252609,176.985485069079));
#17952=CARTESIAN_POINT('Ctrl Pts',(-24.915822344951,15.30429507165,176.985485069079));
#17953=CARTESIAN_POINT('Ctrl Pts',(-24.9867712230002,15.0005829156591,176.985485069079));
#17954=CARTESIAN_POINT('Ctrl Pts',(-25.0589937084744,14.6971400997934,176.985485069079));
#17955=CARTESIAN_POINT('Ctrl Pts',(-25.1324952265289,14.3939806501629,176.985485069079));
#17956=CARTESIAN_POINT('Ctrl Pts',(-25.3191212342609,13.6242354899502,176.985485069079));
#17957=CARTESIAN_POINT('Ctrl Pts',(-25.5139981706041,12.8562891283856,176.985485069079));
#17958=CARTESIAN_POINT('Ctrl Pts',(-25.7172982514514,12.0900656566086,176.985485069079));
#17959=CARTESIAN_POINT('Ctrl Pts',(-25.977816914546,11.1081894386201,176.985485069079));
#17960=CARTESIAN_POINT('Ctrl Pts',(-26.2524109786123,10.1283936032505,176.985485069079));
#17961=CARTESIAN_POINT('Ctrl Pts',(-26.5400675250715,9.15302099692352,176.985485069079));
#17962=CARTESIAN_POINT('Ctrl Pts',(-26.5655456245349,9.06663102741372,176.985485069079));
#17963=CARTESIAN_POINT('Ctrl Pts',(-26.5911262304682,8.98027576367801,176.985485069079));
#17964=CARTESIAN_POINT('Ctrl Pts',(-26.6168086578218,8.89395683843848,176.985485069079));
#17965=CARTESIAN_POINT('Ctrl Pts',(-26.6778123577222,8.68892272158753,176.985485069079));
#17966=CARTESIAN_POINT('Ctrl Pts',(-26.7393942284263,8.48411023451817,176.985485069079));
#17967=CARTESIAN_POINT('Ctrl Pts',(-26.801542811029,8.27950502525835,176.985485069079));
#17968=CARTESIAN_POINT('Ctrl Pts',(-27.106086550375,7.27688786315808,176.985485069079));
#17969=CARTESIAN_POINT('Ctrl Pts',(-27.4242172429184,6.27931159291589,176.985485069079));
#17970=CARTESIAN_POINT('Ctrl Pts',(-27.7542866099677,5.2861618395196,176.985485069079));
#17971=CARTESIAN_POINT('Ctrl Pts',(-27.9852612027692,4.59117956372655,176.985485069079));
#17972=CARTESIAN_POINT('Ctrl Pts',(-28.2220826504089,3.89836521129347,176.985485069079));
#17973=CARTESIAN_POINT('Ctrl Pts',(-28.4641913869893,3.20751217561695,176.985485069079));
#17974=CARTESIAN_POINT('Ctrl Pts',(-28.5351702186733,3.00497532366267,176.985485069079));
#17975=CARTESIAN_POINT('Ctrl Pts',(-28.6066033326334,2.80260753664105,176.985485069079));
#17976=CARTESIAN_POINT('Ctrl Pts',(-28.6784772662389,2.6004019699,176.985485069079));
#17977=CARTESIAN_POINT('Ctrl Pts',(-29.0461821574925,1.56592434776952,176.985485069079));
#17978=CARTESIAN_POINT('Ctrl Pts',(-29.4252407716952,0.535662626378677,
176.985485069079));
#17979=CARTESIAN_POINT('Ctrl Pts',(-29.8124487382319,-0.491577100740066,
176.985485069079));
#17980=CARTESIAN_POINT('Ctrl Pts',(-30.107037119717,-1.27310257222217,176.985485069079));
#17981=CARTESIAN_POINT('Ctrl Pts',(-30.4063418212305,-2.05287902408378,
176.985485069079));
#17982=CARTESIAN_POINT('Ctrl Pts',(-30.7089334673433,-2.83143712039792,
176.985485069079));
#17983=CARTESIAN_POINT('Ctrl Pts',(-30.8040693059046,-3.07621842322983,
176.985485069079));
#17984=CARTESIAN_POINT('Ctrl Pts',(-30.8995300442216,-3.32087962702539,
176.985485069079));
#17985=CARTESIAN_POINT('Ctrl Pts',(-30.995270588929,-3.56543656328317,176.985485069079));
#17986=CARTESIAN_POINT('Ctrl Pts',(-31.3932109940057,-4.58192426529273,
176.985485069079));
#17987=CARTESIAN_POINT('Ctrl Pts',(-31.7957954668658,-5.59669181926987,
176.985485069079));
#17988=CARTESIAN_POINT('Ctrl Pts',(-32.1999884451959,-6.61086118226492,
176.985485069079));
#17989=CARTESIAN_POINT('Ctrl Pts',(-32.5227346634746,-7.42067071421904,
176.985485069079));
#17990=CARTESIAN_POINT('Ctrl Pts',(-32.8465051550323,-8.23009945981376,
176.985485069079));
#17991=CARTESIAN_POINT('Ctrl Pts',(-33.1697310400329,-9.03972997500453,
176.985485069079));
#17992=CARTESIAN_POINT('Ctrl Pts',(-33.2512988465853,-9.24404463019352,
176.985485069079));
#17993=CARTESIAN_POINT('Ctrl Pts',(-33.3328318656186,-9.44837214946192,
176.985485069079));
#17994=CARTESIAN_POINT('Ctrl Pts',(-33.4143043110506,-9.65272099823434,
176.985485069079));
#17995=CARTESIAN_POINT('Ctrl Pts',(-33.9541840790767,-11.0068451869285,
176.985485069079));
#17996=CARTESIAN_POINT('Ctrl Pts',(-34.4913531539213,-12.3619920566898,
176.985485069079));
#17997=CARTESIAN_POINT('Ctrl Pts',(-35.0211191261436,-13.719879020288,176.985485069079));
#17998=CARTESIAN_POINT('Ctrl Pts',(-35.2812503229336,-14.3866427980076,
176.985485069079));
#17999=CARTESIAN_POINT('Ctrl Pts',(-35.5395970138749,-15.0540710424698,
176.985485069079));
#18000=CARTESIAN_POINT('Ctrl Pts',(-35.7955956003909,-15.7223555157655,
176.985485069079));
#18001=CARTESIAN_POINT('Ctrl Pts',(-36.1833029487603,-16.7344657958424,
176.985485069079));
#18002=CARTESIAN_POINT('Ctrl Pts',(-36.5657733621123,-17.7488150534779,
176.985485069079));
#18003=CARTESIAN_POINT('Ctrl Pts',(-36.9419659969045,-18.7652067279702,
176.985485069079));
#18004=CARTESIAN_POINT('Ctrl Pts',(-37.1160044343593,-19.2354211939403,
176.985485069079));
#18005=CARTESIAN_POINT('Ctrl Pts',(-37.2886992867772,-19.7060727594894,
176.985485069079));
#18006=CARTESIAN_POINT('Ctrl Pts',(-37.4599477597535,-20.177141788797,176.985485069079));
#18007=CARTESIAN_POINT('Ctrl Pts',(-37.6325033302003,-20.6518063721319,
176.985485069079));
#18008=CARTESIAN_POINT('Ctrl Pts',(-37.8035923350539,-21.1269004506383,
176.985485069079));
#18009=CARTESIAN_POINT('Ctrl Pts',(-37.9731001370556,-21.6023762842089,
176.985485069079));
#18010=CARTESIAN_POINT('Ctrl Pts',(-37.9989925350158,-21.6750054455681,
176.985485069079));
#18011=CARTESIAN_POINT('Ctrl Pts',(-38.0248480785516,-21.7476436183096,
176.985485069079));
#18012=CARTESIAN_POINT('Ctrl Pts',(-38.0506664067205,-21.8202907608508,
176.985485069079));
#18013=CARTESIAN_POINT('Ctrl Pts',(-38.4931055792047,-23.0652180628431,
176.985485069079));
#18014=CARTESIAN_POINT('Ctrl Pts',(-38.9246977909074,-24.3127099825977,
176.985485069079));
#18015=CARTESIAN_POINT('Ctrl Pts',(-39.3451931578191,-25.5628721161241,
176.985485069079));
#18016=CARTESIAN_POINT('Ctrl Pts',(-39.5292547595282,-26.1101001305087,
176.985485069079));
#18017=CARTESIAN_POINT('Ctrl Pts',(-39.711191090252,-26.6578421174245,176.985485069079));
#18018=CARTESIAN_POINT('Ctrl Pts',(-39.8909793753221,-27.206099092718,176.985485069079));
#18019=CARTESIAN_POINT('Ctrl Pts',(-39.9730744745014,-27.4564447186574,
176.985485069079));
#18020=CARTESIAN_POINT('Ctrl Pts',(-40.0547213113963,-27.7068964984478,
176.985485069079));
#18021=CARTESIAN_POINT('Ctrl Pts',(-40.1359182742855,-27.9574560644933,
176.985485069079));
#18022=CARTESIAN_POINT('Ctrl Pts',(-40.8013599420204,-30.01089217298,176.985485069079));
#18023=CARTESIAN_POINT('Ctrl Pts',(-41.4364827421166,-32.0716508915739,
176.985485069079));
#18024=CARTESIAN_POINT('Ctrl Pts',(-42.0434667820996,-34.1391767207459,
176.985485069079));
#18025=CARTESIAN_POINT('Ctrl Pts',(-42.4136817475693,-35.4002131781069,
176.985485069079));
#18026=CARTESIAN_POINT('Ctrl Pts',(-42.7734294290581,-36.663766907072,176.985485069079));
#18027=CARTESIAN_POINT('Ctrl Pts',(-43.123209233354,-37.9297105093382,176.985485069079));
#18028=CARTESIAN_POINT('Ctrl Pts',(-43.346909105782,-38.7393382204009,176.985485069079));
#18029=CARTESIAN_POINT('Ctrl Pts',(-43.5665312274966,-39.5499404131169,
176.985485069079));
#18030=CARTESIAN_POINT('Ctrl Pts',(-43.7822103601003,-40.3614968011214,
176.985485069079));
#18031=CARTESIAN_POINT('Ctrl Pts',(-44.519585351179,-43.1360878203846,176.985485069079));
#18032=CARTESIAN_POINT('Ctrl Pts',(-45.211388601689,-45.9216172075444,176.985485069079));
#18033=CARTESIAN_POINT('Ctrl Pts',(-45.8641427980324,-48.7165333394889,
176.985485069079));
#18034=CARTESIAN_POINT('Ctrl Pts',(-46.1914364418981,-50.1179158051206,
176.985485069079));
#18035=CARTESIAN_POINT('Ctrl Pts',(-46.5089121176543,-51.5216577766851,
176.985485069079));
#18036=CARTESIAN_POINT('Ctrl Pts',(-46.8173885348151,-52.9275664406215,
176.985485069079));
#18037=CARTESIAN_POINT('Ctrl Pts',(-47.4870367014129,-55.9795474246911,
176.985485069079));
#18038=CARTESIAN_POINT('Ctrl Pts',(-48.114346647767,-59.0416984673988,176.985485069079));
#18039=CARTESIAN_POINT('Ctrl Pts',(-48.7060174445671,-62.1124135687292,
176.985485069079));
#18040=CARTESIAN_POINT('Ctrl Pts',(-48.9313936321896,-63.2820945240097,
176.985485069079));
#18041=CARTESIAN_POINT('Ctrl Pts',(-49.1515981816455,-64.4530182376069,
176.985485069079));
#18042=CARTESIAN_POINT('Ctrl Pts',(-49.3669995999362,-65.6250971770435,
176.985485069079));
#18043=CARTESIAN_POINT('Ctrl Pts',(-50.0153496236315,-69.1530099186912,
176.985485069079));
#18044=CARTESIAN_POINT('Ctrl Pts',(-50.6201441923267,-72.6913972594903,
176.985485069162));
#18045=CARTESIAN_POINT('Ctrl Pts',(-51.1888177613378,-76.2384559838746,
176.985485069122));
#18046=CARTESIAN_POINT('',(-23.70581036359,21.1602846666598,174.985485069079));
#18047=CARTESIAN_POINT('',(-23.70581036359,21.1602846666598,175.985485069079));
#18048=CARTESIAN_POINT('Ctrl Pts',(-51.1887931847522,-76.2384284136363,
174.985485069079));
#18049=CARTESIAN_POINT('Ctrl Pts',(-50.5213346265716,-72.0755903721384,
174.985485069079));
#18050=CARTESIAN_POINT('Ctrl Pts',(-49.8042721930313,-67.9239395141956,
174.985485069079));
#18051=CARTESIAN_POINT('Ctrl Pts',(-48.2454967538896,-59.6487390071956,
174.985485069079));
#18052=CARTESIAN_POINT('Ctrl Pts',(-47.4038384436995,-55.5251770226586,
174.985485069079));
#18053=CARTESIAN_POINT('Ctrl Pts',(-45.5617895517713,-47.3138520117311,
174.985485069079));
#18054=CARTESIAN_POINT('Ctrl Pts',(-44.5612309815417,-43.2261268718582,
174.985485069079));
#18055=CARTESIAN_POINT('Ctrl Pts',(-42.3590336034264,-35.0960263054489,
174.985485069079));
#18056=CARTESIAN_POINT('Ctrl Pts',(-41.1560792064761,-31.0539475842857,
174.985485069079));
#18057=CARTESIAN_POINT('Ctrl Pts',(-39.1758099410217,-25.0304862486367,
174.985485069079));
#18058=CARTESIAN_POINT('Ctrl Pts',(-38.486561950554,-23.0292418728959,174.985485069079));
#18059=CARTESIAN_POINT('Ctrl Pts',(-37.0529631635479,-19.039180481201,174.985485069079));
#18060=CARTESIAN_POINT('Ctrl Pts',(-36.3087744035167,-17.0515279744533,
174.985485069079));
#18061=CARTESIAN_POINT('Ctrl Pts',(-34.7825960540618,-13.0925681835044,
174.985485069079));
#18062=CARTESIAN_POINT('Ctrl Pts',(-34.0001212951122,-11.1203014222748,
174.985485069079));
#18063=CARTESIAN_POINT('Ctrl Pts',(-32.4270421820337,-7.17879282084528,
174.985485069079));
#18064=CARTESIAN_POINT('Ctrl Pts',(-31.6366800593758,-5.20946084933443,
174.985485069079));
#18065=CARTESIAN_POINT('Ctrl Pts',(-30.0940103202672,-1.25663729890807,
174.985485069079));
#18066=CARTESIAN_POINT('Ctrl Pts',(-29.342391793721,0.727110681771283,174.985485069079));
#18067=CARTESIAN_POINT('Ctrl Pts',(-27.9248341481098,4.7264868826472,174.985485069079));
#18068=CARTESIAN_POINT('Ctrl Pts',(-27.2593908283077,6.74229958356928,174.985485069079));
#18069=CARTESIAN_POINT('Ctrl Pts',(-26.0425659871153,10.8163659588052,174.985485069079));
#18070=CARTESIAN_POINT('Ctrl Pts',(-25.4928841138196,12.8686487455774,174.985485069079));
#18071=CARTESIAN_POINT('Ctrl Pts',(-24.5138232792971,16.9962588567196,174.985485069079));
#18072=CARTESIAN_POINT('Ctrl Pts',(-24.0836324787232,19.072696737701,174.985485069079));
#18073=CARTESIAN_POINT('Ctrl Pts',(-23.7058105558977,21.1602836040985,174.985485069079));
#18074=CARTESIAN_POINT('Ctrl Pts',(-53.0167365461859,-78.193620158077,173.485485069079));
#18075=CARTESIAN_POINT('Ctrl Pts',(-51.5346787297268,-78.4249308337329,
173.485485069079));
#18076=CARTESIAN_POINT('Ctrl Pts',(-51.5346787297268,-78.4249308337329,
174.985485069079));
#18077=CARTESIAN_POINT('Ctrl Pts',(-52.3478408594839,-73.9078599867829,
173.485485069079));
#18078=CARTESIAN_POINT('Ctrl Pts',(-50.8676276544628,-74.1509894892529,
173.485485069079));
#18079=CARTESIAN_POINT('Ctrl Pts',(-50.8676276544411,-74.150989489256,174.985485069079));
#18080=CARTESIAN_POINT('Ctrl Pts',(-51.6285617065834,-69.6334497110788,
173.485485069079));
#18081=CARTESIAN_POINT('Ctrl Pts',(-50.1505302305787,-69.8896731372056,
173.485485069079));
#18082=CARTESIAN_POINT('Ctrl Pts',(-50.150530230561,-69.8896731372089,174.985485069079));
#18083=CARTESIAN_POINT('Ctrl Pts',(-50.0631495457321,-61.113268493176,173.485485069079));
#18084=CARTESIAN_POINT('Ctrl Pts',(-48.5905691191417,-61.3991607376064,
173.485485069079));
#18085=CARTESIAN_POINT('Ctrl Pts',(-48.5905691191594,-61.3991607376031,
174.985485069079));
#18086=CARTESIAN_POINT('Ctrl Pts',(-49.2170840953273,-56.8674733632373,
173.485485069079));
#18087=CARTESIAN_POINT('Ctrl Pts',(-47.7477702624369,-57.16994536236,173.485485069079));
#18088=CARTESIAN_POINT('Ctrl Pts',(-47.7477702623948,-57.1699453623542,
174.985485069079));
#18089=CARTESIAN_POINT('Ctrl Pts',(-47.3628470711911,-48.4124583507524,
173.485485069079));
#18090=CARTESIAN_POINT('Ctrl Pts',(-45.9018015025242,-48.7526322710164,
173.485485069079));
#18091=CARTESIAN_POINT('Ctrl Pts',(-45.9018015025663,-48.7526322710222,
174.985485069079));
#18092=CARTESIAN_POINT('Ctrl Pts',(-46.3545427330907,-44.2032684234675,
173.485485069079));
#18093=CARTESIAN_POINT('Ctrl Pts',(-44.8985120597276,-44.5646201418261,
173.485485069079));
#18094=CARTESIAN_POINT('Ctrl Pts',(-44.8985120596695,-44.5646201418415,
174.985485069079));
#18095=CARTESIAN_POINT('Ctrl Pts',(-44.1311171174038,-35.8315517093622,
173.485485069079));
#18096=CARTESIAN_POINT('Ctrl Pts',(-42.6876656315475,-36.2402670065083,
173.485485069079));
#18097=CARTESIAN_POINT('Ctrl Pts',(-42.6876656316057,-36.2402670064929,
174.985485069079));
#18098=CARTESIAN_POINT('Ctrl Pts',(-42.9147512260831,-31.6693057388972,
173.485485069079));
#18099=CARTESIAN_POINT('Ctrl Pts',(-41.4789698205316,-32.1044366637925,
173.485485069079));
#18100=CARTESIAN_POINT('Ctrl Pts',(-41.4789698205142,-32.1044366638057,
174.985485069079));
#18101=CARTESIAN_POINT('Ctrl Pts',(-40.906208719954,-25.467450415631,173.485485069079));
#18102=CARTESIAN_POINT('Ctrl Pts',(-39.4835575759942,-25.9431241632503,
173.485485069079));
#18103=CARTESIAN_POINT('Ctrl Pts',(-39.4835575760029,-25.9431241632437,
174.985485069079));
#18104=CARTESIAN_POINT('Ctrl Pts',(-40.206142545412,-23.4070586143658,173.485485069079));
#18105=CARTESIAN_POINT('Ctrl Pts',(-38.7881219432854,-23.8963460449173,
173.485485069079));
#18106=CARTESIAN_POINT('Ctrl Pts',(-38.7881219432977,-23.8963460449054,
174.985485069079));
#18107=CARTESIAN_POINT('Ctrl Pts',(-38.7470879355323,-19.2995693663361,
173.485485069079));
#18108=CARTESIAN_POINT('Ctrl Pts',(-37.3381634907308,-19.8144640416042,
173.485485069079));
#18109=CARTESIAN_POINT('Ctrl Pts',(-37.3381634907185,-19.8144640416161,
174.985485069079));
#18110=CARTESIAN_POINT('Ctrl Pts',(-37.9878548350367,-17.2526269837786,
173.485485069079));
#18111=CARTESIAN_POINT('Ctrl Pts',(-36.5834023703057,-17.7795215046325,
173.485485069079));
#18112=CARTESIAN_POINT('Ctrl Pts',(-36.5834023703931,-17.7795215045991,
174.985485069079));
#18113=CARTESIAN_POINT('Ctrl Pts',(-36.4271652313825,-13.1772568450141,
173.485485069079));
#18114=CARTESIAN_POINT('Ctrl Pts',(-35.0300266743469,-13.7232498983064,
173.485485069079));
#18115=CARTESIAN_POINT('Ctrl Pts',(-35.0300266742596,-13.7232498983399,
174.985485069079));
#18116=CARTESIAN_POINT('Ctrl Pts',(-35.6251003133685,-11.1476565297151,
173.485485069079));
#18117=CARTESIAN_POINT('Ctrl Pts',(-34.2307808988101,-11.7007208831933,
173.485485069079));
#18118=CARTESIAN_POINT('Ctrl Pts',(-34.2307808989649,-11.7007208831316,
174.985485069079));
#18119=CARTESIAN_POINT('Ctrl Pts',(-34.008647106654,-7.09304295664572,173.485485069079));
#18120=CARTESIAN_POINT('Ctrl Pts',(-32.6162603377718,-7.65095504179,173.485485069079));
#18121=CARTESIAN_POINT('Ctrl Pts',(-32.616260337617,-7.65095504185172,174.985485069079));
#18122=CARTESIAN_POINT('Ctrl Pts',(-33.1944598949962,-5.06795485306577,
173.485485069079));
#18123=CARTESIAN_POINT('Ctrl Pts',(-31.8011075370691,-5.62352303603581,
173.485485069079));
#18124=CARTESIAN_POINT('Ctrl Pts',(-31.8011075372865,-5.62352303595069,
174.985485069079));
#18125=CARTESIAN_POINT('Ctrl Pts',(-31.6032144550666,-1.00395833775079,
173.485485069079));
#18126=CARTESIAN_POINT('Ctrl Pts',(-30.2030685122845,-1.54217589428156,
173.485485069079));
#18127=CARTESIAN_POINT('Ctrl Pts',(-30.2030685120672,-1.54217589436668,
174.985485069079));
#18128=CARTESIAN_POINT('Ctrl Pts',(-30.8269429206595,1.03524290056039,173.485485069079));
#18129=CARTESIAN_POINT('Ctrl Pts',(-29.420943080133,0.512133922373698,173.485485069079));
#18130=CARTESIAN_POINT('Ctrl Pts',(-29.4209430803042,0.512133922435039,
174.985485069079));
#18131=CARTESIAN_POINT('Ctrl Pts',(-29.364921121899,5.14733958959975,173.485485069079));
#18132=CARTESIAN_POINT('Ctrl Pts',(-27.9442645188942,4.66545436370176,173.485485069079));
#18133=CARTESIAN_POINT('Ctrl Pts',(-27.944264518723,4.66545436364042,174.985485069079));
#18134=CARTESIAN_POINT('Ctrl Pts',(-28.6798159809479,7.22047517089018,173.485485069079));
#18135=CARTESIAN_POINT('Ctrl Pts',(-27.2504765600523,6.76457334823395,173.485485069079));
#18136=CARTESIAN_POINT('Ctrl Pts',(-27.2504765601174,6.76457334825143,174.985485069079));
#18137=CARTESIAN_POINT('Ctrl Pts',(-27.4323595727382,11.4124383027362,173.485485069079));
#18138=CARTESIAN_POINT('Ctrl Pts',(-25.9863143172519,11.0126749088339,173.485485069079));
#18139=CARTESIAN_POINT('Ctrl Pts',(-25.9863143171867,11.0126749088164,174.985485069079));
#18140=CARTESIAN_POINT('Ctrl Pts',(-26.872482605583,13.5225670882055,173.485485069079));
#18141=CARTESIAN_POINT('Ctrl Pts',(-25.418512449069,13.1526523639037,173.485485069079));
#18142=CARTESIAN_POINT('Ctrl Pts',(-25.4185124490178,13.1526523638918,174.985485069079));
#18143=CARTESIAN_POINT('Ctrl Pts',(-25.8817163327183,17.7633008300245,173.485485069079));
#18144=CARTESIAN_POINT('Ctrl Pts',(-24.4143553121838,17.4507024379655,173.485485069079));
#18145=CARTESIAN_POINT('Ctrl Pts',(-24.414355312235,17.4507024379774,174.985485069079));
#18146=CARTESIAN_POINT('Ctrl Pts',(-25.4498962389785,19.8950365279689,173.485485069079));
#18147=CARTESIAN_POINT('Ctrl Pts',(-23.9770093214825,19.6099821711675,173.485485069079));
#18148=CARTESIAN_POINT('Ctrl Pts',(-23.9770093216439,19.6099821711937,174.985485069079));
#18149=CARTESIAN_POINT('Ctrl Pts',(-25.0731194387121,22.0366182599054,173.485485069079));
#18150=CARTESIAN_POINT('Ctrl Pts',(-23.595808607555,21.7767092216907,173.485485069079));
#18151=CARTESIAN_POINT('Ctrl Pts',(-23.595808607555,21.7767092216907,174.985485069079));
#18152=CARTESIAN_POINT('',(-25.2666963042962,20.9635176568293,173.485485069079));
#18153=CARTESIAN_POINT('Ctrl Pts',(-25.2666963042962,20.9635176568293,173.485485069184));
#18154=CARTESIAN_POINT('Ctrl Pts',(-25.5390668113124,19.4904292891436,173.485485069662));
#18155=CARTESIAN_POINT('Ctrl Pts',(-25.8381519757544,18.0230368201297,173.485485069241));
#18156=CARTESIAN_POINT('Ctrl Pts',(-26.1664788972763,16.5619707154367,173.485485069193));
#18157=CARTESIAN_POINT('Ctrl Pts',(-26.2353834496847,16.2553430849141,173.485485069182));
#18158=CARTESIAN_POINT('Ctrl Pts',(-26.3055757539796,15.9489940033786,173.485485069186));
#18159=CARTESIAN_POINT('Ctrl Pts',(-26.3770789088467,15.6429291555935,173.485485069228));
#18160=CARTESIAN_POINT('Ctrl Pts',(-26.3900846439141,15.5872589081597,173.485485069236));
#18161=CARTESIAN_POINT('Ctrl Pts',(-26.4031343886611,15.5315972847617,173.485485069245));
#18162=CARTESIAN_POINT('Ctrl Pts',(-26.4162281158535,15.4759443627374,173.485485069255));
#18163=CARTESIAN_POINT('Ctrl Pts',(-26.6573637297862,14.4510336308838,173.485485069454));
#18164=CARTESIAN_POINT('Ctrl Pts',(-26.9133448526214,13.4293094309892,173.48548507148));
#18165=CARTESIAN_POINT('Ctrl Pts',(-27.1842247243902,12.4107800921172,173.485485073504));
#18166=CARTESIAN_POINT('Ctrl Pts',(-27.3942455790166,11.6210853805271,173.485485075074));
#18167=CARTESIAN_POINT('Ctrl Pts',(-27.6132236088869,10.8333114203593,173.485485075017));
#18168=CARTESIAN_POINT('Ctrl Pts',(-27.8412042451402,10.0474684120255,173.485485072249));
#18169=CARTESIAN_POINT('Ctrl Pts',(-27.9119589207625,9.80357898326325,173.48548507139));
#18170=CARTESIAN_POINT('Ctrl Pts',(-27.9835604982678,9.55990044821291,173.485485071169));
#18171=CARTESIAN_POINT('Ctrl Pts',(-28.056011326395,9.31643398646967,173.4854850712));
#18172=CARTESIAN_POINT('Ctrl Pts',(-28.3631180387437,8.28442115009738,173.485485071334));
#18173=CARTESIAN_POINT('Ctrl Pts',(-28.684880487986,7.25832458735522,173.485485080559));
#18174=CARTESIAN_POINT('Ctrl Pts',(-29.0197368390196,6.23709829128275,173.485485084382));
#18175=CARTESIAN_POINT('Ctrl Pts',(-29.1887218714363,5.72173712756616,173.485485086311));
#18176=CARTESIAN_POINT('Ctrl Pts',(-29.3610422350258,5.20761689664156,173.485485084578));
#18177=CARTESIAN_POINT('Ctrl Pts',(-29.536500843974,4.69460639756019,173.485485078889));
#18178=CARTESIAN_POINT('Ctrl Pts',(-29.7197047622074,4.15894995932641,173.48548507295));
#18179=CARTESIAN_POINT('Ctrl Pts',(-29.9062419246547,3.62453460775134,173.485485071986));
#18180=CARTESIAN_POINT('Ctrl Pts',(-30.0958541508489,3.09126355889583,173.485485071356));
#18181=CARTESIAN_POINT('Ctrl Pts',(-30.5325765715419,1.86301246973321,173.485485069905));
#18182=CARTESIAN_POINT('Ctrl Pts',(-30.9853820483243,0.640745301943924,
173.485485072493));
#18183=CARTESIAN_POINT('Ctrl Pts',(-31.4488862792226,-0.577537461199393,
173.485485071091));
#18184=CARTESIAN_POINT('Ctrl Pts',(-31.7612655378603,-1.39860065974716,
173.485485070145));
#18185=CARTESIAN_POINT('Ctrl Pts',(-32.0784620377525,-2.2178705925264,173.485485069987));
#18186=CARTESIAN_POINT('Ctrl Pts',(-32.3987898977171,-3.0359751066965,173.485485069939));
#18187=CARTESIAN_POINT('Ctrl Pts',(-33.1944157816222,-5.06797172193035,
173.485485069819));
#18188=CARTESIAN_POINT('Ctrl Pts',(-34.0085729745541,-7.09307153439624,
173.485485071134));
#18189=CARTESIAN_POINT('Ctrl Pts',(-34.8168112016355,-9.12037466340095,
173.485485070589));
#18190=CARTESIAN_POINT('Ctrl Pts',(-35.0680967005658,-9.75067382667439,
173.485485070419));
#18191=CARTESIAN_POINT('Ctrl Pts',(-35.3187906222336,-10.3811932006048,
173.485485070032));
#18192=CARTESIAN_POINT('Ctrl Pts',(-35.5684276654212,-11.0121060305728,
173.485485069631));
#18193=CARTESIAN_POINT('Ctrl Pts',(-36.1217247789942,-12.4104651974658,
173.485485068744));
#18194=CARTESIAN_POINT('Ctrl Pts',(-36.6697688098148,-13.8108892372659,
173.485485069808));
#18195=CARTESIAN_POINT('Ctrl Pts',(-37.2074679799087,-15.2149580189824,
173.485485069755));
#18196=CARTESIAN_POINT('Ctrl Pts',(-37.3382977633442,-15.5565877347367,
173.485485069743));
#18197=CARTESIAN_POINT('Ctrl Pts',(-37.468532295522,-15.8984661779842,173.485485069646));
#18198=CARTESIAN_POINT('Ctrl Pts',(-37.5981312331992,-16.2405772327452,
173.485485069487));
#18199=CARTESIAN_POINT('Ctrl Pts',(-38.2042320224057,-17.8405423559423,
173.485485068741));
#18200=CARTESIAN_POINT('Ctrl Pts',(-38.7966004837565,-19.4464162536689,
173.485485069125));
#18201=CARTESIAN_POINT('Ctrl Pts',(-39.3708921954468,-21.0563433907389,
173.485485069113));
#18202=CARTESIAN_POINT('Ctrl Pts',(-39.4061988551619,-21.1553194832674,
173.485485069112));
#18203=CARTESIAN_POINT('Ctrl Pts',(-39.4414372081829,-21.2543108915996,
173.485485069111));
#18204=CARTESIAN_POINT('Ctrl Pts',(-39.4766062520292,-21.3533171832087,
173.48548506911));
#18205=CARTESIAN_POINT('Ctrl Pts',(-39.4944222863477,-21.403472072172,173.485485069109));
#18206=CARTESIAN_POINT('Ctrl Pts',(-39.5122206800506,-21.4536306880927,
173.485485069108));
#18207=CARTESIAN_POINT('Ctrl Pts',(-39.5300014121829,-21.5037930140745,
173.485485069108));
#18208=CARTESIAN_POINT('Ctrl Pts',(-40.2403129504007,-23.5076969401649,
173.485485069076));
#18209=CARTESIAN_POINT('Ctrl Pts',(-40.9225571901282,-25.5179357583437,
173.48548506908));
#18210=CARTESIAN_POINT('Ctrl Pts',(-41.5757221904205,-27.5347357495206,
173.48548506908));
#18211=CARTESIAN_POINT('Ctrl Pts',(-42.0697840289797,-29.0602674470261,
173.485485069079));
#18212=CARTESIAN_POINT('Ctrl Pts',(-42.5471460562807,-30.5895671389256,
173.485485069079));
#18213=CARTESIAN_POINT('Ctrl Pts',(-43.0087134036266,-32.1224297907549,
173.485485069079));
#18214=CARTESIAN_POINT('Ctrl Pts',(-43.7981108509673,-34.744014422848,173.485485069079));
#18215=CARTESIAN_POINT('Ctrl Pts',(-44.5413060994664,-37.376009024523,173.48548506902));
#18216=CARTESIAN_POINT('Ctrl Pts',(-45.2428170647038,-40.017413482018,173.485485069138));
#18217=CARTESIAN_POINT('Ctrl Pts',(-45.493755279941,-40.9622730111334,173.485485069181));
#18218=CARTESIAN_POINT('Ctrl Pts',(-45.7394230807557,-41.9083222817218,
173.485485069254));
#18219=CARTESIAN_POINT('Ctrl Pts',(-45.9800756370086,-42.855504556733,173.485485069449));
#18220=CARTESIAN_POINT('Ctrl Pts',(-46.8055463757926,-46.1044675617001,
173.485485070117));
#18221=CARTESIAN_POINT('Ctrl Pts',(-47.5720486324278,-49.3667352679054,
173.485485070976));
#18222=CARTESIAN_POINT('Ctrl Pts',(-48.2898944467056,-52.6399814576805,
173.485485070847));
#18223=CARTESIAN_POINT('Ctrl Pts',(-49.1606867247392,-56.6106356698621,
173.485485070692));
#18224=CARTESIAN_POINT('Ctrl Pts',(-49.9599970866321,-60.5974185446697,
173.485485069199));
#18225=CARTESIAN_POINT('Ctrl Pts',(-50.7024802268295,-64.5970226062537,
173.485485069085));
#18226=CARTESIAN_POINT('Ctrl Pts',(-23.7058176254365,21.1602837512234,174.985485069079));
#18227=CARTESIAN_POINT('Ctrl Pts',(-23.7058176254338,21.1602837512238,174.885642109295));
#18228=CARTESIAN_POINT('Ctrl Pts',(-23.7161844830976,21.1589768936689,174.786144799866));
#18229=CARTESIAN_POINT('Ctrl Pts',(-23.7586235790639,21.1536269742447,174.584144405165));
#18230=CARTESIAN_POINT('Ctrl Pts',(-23.7919598395692,21.1494245683377,174.482671933397));
#18231=CARTESIAN_POINT('Ctrl Pts',(-23.9170832171616,21.1336513768272,174.206914149823));
#18232=CARTESIAN_POINT('Ctrl Pts',(-24.0329636094545,21.1190433662763,174.046600077944));
#18233=CARTESIAN_POINT('Ctrl Pts',(-24.3205549456233,21.0827892840302,173.776548691605));
#18234=CARTESIAN_POINT('Ctrl Pts',(-24.4902654671712,21.0613953877858,173.670082332604));
#18235=CARTESIAN_POINT('Ctrl Pts',(-24.8631831017534,21.0143849778922,173.523272452218));
#18236=CARTESIAN_POINT('Ctrl Pts',(-25.0642980581857,20.9890322038205,173.485487368252));
#18237=CARTESIAN_POINT('Ctrl Pts',(-25.2666963042962,20.9635176568293,173.485485069184));
#18238=CARTESIAN_POINT('Ctrl Pts',(-25.0731721461106,22.0363186756089,178.485485069079));
#18239=CARTESIAN_POINT('Ctrl Pts',(-23.5958619350554,21.7764061127883,178.485485069079));
#18240=CARTESIAN_POINT('Ctrl Pts',(-23.5958619350554,21.7764061127883,176.985485069079));
#18241=CARTESIAN_POINT('Ctrl Pts',(-25.449767355314,19.8957990247877,178.485485069079));
#18242=CARTESIAN_POINT('Ctrl Pts',(-23.9768789732964,19.6107533436813,178.485485069079));
#18243=CARTESIAN_POINT('Ctrl Pts',(-23.9768789734403,19.6107533437049,176.985485069079));
#18244=CARTESIAN_POINT('Ctrl Pts',(-25.8813662389046,17.7650280978455,178.485485069079));
#18245=CARTESIAN_POINT('Ctrl Pts',(-24.4140007103611,17.4524520931911,178.485485069079));
#18246=CARTESIAN_POINT('Ctrl Pts',(-24.4140007103993,17.4524520932,176.985485069079));
#18247=CARTESIAN_POINT('Ctrl Pts',(-26.6240610131928,14.5857610350515,178.485485069079));
#18248=CARTESIAN_POINT('Ctrl Pts',(-25.166733162246,14.2302165608794,178.485485069079));
#18249=CARTESIAN_POINT('Ctrl Pts',(-25.1667331622269,14.230216560875,176.985485069079));
#18250=CARTESIAN_POINT('Ctrl Pts',(-26.8874605581482,13.5288117467589,178.485485069079));
#18251=CARTESIAN_POINT('Ctrl Pts',(-25.4337662241453,13.1586775991956,178.485485069079));
#18252=CARTESIAN_POINT('Ctrl Pts',(-25.4337662241455,13.1586775991956,176.985485069079));
#18253=CARTESIAN_POINT('Ctrl Pts',(-27.446805326032,11.4206813014582,178.485485069079));
#18254=CARTESIAN_POINT('Ctrl Pts',(-26.0008302787574,11.0214537140216,178.485485069079));
#18255=CARTESIAN_POINT('Ctrl Pts',(-26.0008302787573,11.0214537140216,176.985485069079));
#18256=CARTESIAN_POINT('Ctrl Pts',(-27.7430372661709,10.3686225285901,178.485485069079));
#18257=CARTESIAN_POINT('Ctrl Pts',(-26.3011521526689,9.95488187865359,178.485485069079));
#18258=CARTESIAN_POINT('Ctrl Pts',(-26.3011521526342,9.95488187864326,176.985485069079));
#18259=CARTESIAN_POINT('Ctrl Pts',(-28.6774913665414,7.22791185787921,178.485485069079));
#18260=CARTESIAN_POINT('Ctrl Pts',(-27.2481216681276,6.77210675800827,178.485485069079));
#18261=CARTESIAN_POINT('Ctrl Pts',(-27.248121668197,6.77210675802894,176.985485069079));
#18262=CARTESIAN_POINT('Ctrl Pts',(-29.3617331966933,5.15683817240694,178.485485069079));
#18263=CARTESIAN_POINT('Ctrl Pts',(-27.9410378920011,4.67506713939723,178.485485069079));
#18264=CARTESIAN_POINT('Ctrl Pts',(-27.9410378918206,4.67506713933211,176.985485069079));
#18265=CARTESIAN_POINT('Ctrl Pts',(-30.8219597323256,1.04872943986564,178.485485069079));
#18266=CARTESIAN_POINT('Ctrl Pts',(-29.4159166404766,0.525736800402789,
178.485485069079));
#18267=CARTESIAN_POINT('Ctrl Pts',(-29.4159166406572,0.525736800467916,
176.985485069079));
#18268=CARTESIAN_POINT('Ctrl Pts',(-31.5973036296917,-0.988543361219867,
178.485485069079));
#18269=CARTESIAN_POINT('Ctrl Pts',(-30.1971187077986,-1.52665999924347,
178.485485069079));
#18270=CARTESIAN_POINT('Ctrl Pts',(-30.1971187075851,-1.52665999932655,
176.985485069079));
#18271=CARTESIAN_POINT('Ctrl Pts',(-33.1867939298434,-5.04869237462202,
178.485485069079));
#18272=CARTESIAN_POINT('Ctrl Pts',(-31.7934224700594,-5.60421312732288,
178.485485069079));
#18273=CARTESIAN_POINT('Ctrl Pts',(-31.7934224702728,-5.6042131272398,176.985485069079));
#18274=CARTESIAN_POINT('Ctrl Pts',(-34.0001554699584,-7.07185978834832,
178.485485069079));
#18275=CARTESIAN_POINT('Ctrl Pts',(-32.6077646596627,-7.62976159871099,
178.485485069079));
#18276=CARTESIAN_POINT('Ctrl Pts',(-32.6077646595,-7.62976159877585,176.985485069079));
#18277=CARTESIAN_POINT('Ctrl Pts',(-35.6151374324291,-11.1225508305231,
178.485485069079));
#18278=CARTESIAN_POINT('Ctrl Pts',(-34.2208439624386,-11.6756803977577,
178.485485069079));
#18279=CARTESIAN_POINT('Ctrl Pts',(-34.2208439626013,-11.6756803976928,
176.985485069079));
#18280=CARTESIAN_POINT('Ctrl Pts',(-36.4165552279516,-13.1501496379901,
178.485485069079));
#18281=CARTESIAN_POINT('Ctrl Pts',(-35.019457301644,-13.6962459918701,178.485485069079));
#18282=CARTESIAN_POINT('Ctrl Pts',(-35.0194573015643,-13.6962459919006,
176.985485069079));
#18283=CARTESIAN_POINT('Ctrl Pts',(-37.9761224198699,-17.2214007871766,
178.485485069079));
#18284=CARTESIAN_POINT('Ctrl Pts',(-36.5717338991378,-17.7484650396609,
178.485485069079));
#18285=CARTESIAN_POINT('Ctrl Pts',(-36.5717338992174,-17.7484650396304,
176.985485069079));
#18286=CARTESIAN_POINT('Ctrl Pts',(-38.734830150851,-19.2660838657735,178.485485069079));
#18287=CARTESIAN_POINT('Ctrl Pts',(-37.325978725329,-19.7811777344504,178.485485069079));
#18288=CARTESIAN_POINT('Ctrl Pts',(-37.3259787253131,-19.7811777344522,
176.985485069079));
#18289=CARTESIAN_POINT('Ctrl Pts',(-40.1932912302604,-23.3698751428974,
178.485485069079));
#18290=CARTESIAN_POINT('Ctrl Pts',(-38.775354088112,-23.8594037872512,178.485485069079));
#18291=CARTESIAN_POINT('Ctrl Pts',(-38.7753540881279,-23.8594037872493,
176.985485069079));
#18292=CARTESIAN_POINT('Ctrl Pts',(-40.8932729804717,-25.4288026626252,
178.485485069079));
#18293=CARTESIAN_POINT('Ctrl Pts',(-39.4707067838494,-25.9047302427165,
178.485485069079));
#18294=CARTESIAN_POINT('Ctrl Pts',(-39.4707067838488,-25.9047302427205,
176.985485069079));
#18295=CARTESIAN_POINT('Ctrl Pts',(-42.9020403232724,-31.6275058626836,
178.485485069079));
#18296=CARTESIAN_POINT('Ctrl Pts',(-41.4663412551578,-32.062907708047,178.485485069079));
#18297=CARTESIAN_POINT('Ctrl Pts',(-41.466341255159,-32.062907708039,176.985485069079));
#18298=CARTESIAN_POINT('Ctrl Pts',(-44.1191756103108,-35.7893157557914,
178.485485069079));
#18299=CARTESIAN_POINT('Ctrl Pts',(-42.6757961471886,-36.1982867984866,
178.485485069079));
#18300=CARTESIAN_POINT('Ctrl Pts',(-42.6757961472487,-36.1982867984707,
176.985485069079));
#18301=CARTESIAN_POINT('Ctrl Pts',(-46.3446034332256,-44.1631447109512,
178.485485069079));
#18302=CARTESIAN_POINT('Ctrl Pts',(-44.8886245730121,-44.5247068037562,
178.485485069079));
#18303=CARTESIAN_POINT('Ctrl Pts',(-44.888624572952,-44.5247068037722,176.985485069079));
#18304=CARTESIAN_POINT('Ctrl Pts',(-47.3541432037895,-48.3748639172974,
178.485485069079));
#18305=CARTESIAN_POINT('Ctrl Pts',(-45.8931392134411,-48.7152180852625,
178.485485069079));
#18306=CARTESIAN_POINT('Ctrl Pts',(-45.8931392134804,-48.7152180852388,
176.985485069079));
#18307=CARTESIAN_POINT('Ctrl Pts',(-49.2109269784403,-56.8373208523129,
178.485485069079));
#18308=CARTESIAN_POINT('Ctrl Pts',(-47.7416378561892,-57.1399147959804,
178.485485069079));
#18309=CARTESIAN_POINT('Ctrl Pts',(-47.7416378561499,-57.1399147960041,
176.985485069079));
#18310=CARTESIAN_POINT('Ctrl Pts',(-50.0583093223098,-61.0880253217963,
178.485485069079));
#18311=CARTESIAN_POINT('Ctrl Pts',(-48.5857467556546,-61.3740109382993,
178.485485069079));
#18312=CARTESIAN_POINT('Ctrl Pts',(-48.5857467557009,-61.3740109382908,
176.985485069079));
#18313=CARTESIAN_POINT('Ctrl Pts',(-51.6262769651782,-69.6199183168499,
178.485485069079));
#18314=CARTESIAN_POINT('Ctrl Pts',(-50.1482524442177,-69.8761834157877,
178.485485069079));
#18315=CARTESIAN_POINT('Ctrl Pts',(-50.1482524441714,-69.8761834157962,
176.985485069079));
#18316=CARTESIAN_POINT('Ctrl Pts',(-52.3467978062058,-73.9011331254681,
178.485485069079));
#18317=CARTESIAN_POINT('Ctrl Pts',(-50.8665874458362,-74.144280974491,178.4854850692));
#18318=CARTESIAN_POINT('Ctrl Pts',(-50.8665874457456,-74.1442809745042,
176.9854850692));
#18319=CARTESIAN_POINT('Ctrl Pts',(-53.0168669615071,-78.1944557616716,
178.485485069079));
#18320=CARTESIAN_POINT('Ctrl Pts',(-51.5348087855333,-78.4257641338267,
178.485485069079));
#18321=CARTESIAN_POINT('Ctrl Pts',(-51.5348087855333,-78.4257641338267,
176.985485069079));
#18322=CARTESIAN_POINT('Ctrl Pts',(-25.2666963042872,20.9635176568304,178.485485068975));
#18323=CARTESIAN_POINT('Ctrl Pts',(-25.0646700006886,20.9889853163368,178.485482782905));
#18324=CARTESIAN_POINT('Ctrl Pts',(-24.8639197630959,21.0142921135478,178.44783645175));
#18325=CARTESIAN_POINT('Ctrl Pts',(-24.491242863047,21.0612721761796,178.301420092223));
#18326=CARTESIAN_POINT('Ctrl Pts',(-24.3214536667684,21.0826759902477,178.195070264549));
#18327=CARTESIAN_POINT('Ctrl Pts',(-24.0336437827003,21.1189576228839,177.925200211993));
#18328=CARTESIAN_POINT('Ctrl Pts',(-23.917632133555,21.1335821798189,177.76494125067));
#18329=CARTESIAN_POINT('Ctrl Pts',(-23.7922348975327,21.1493898942263,177.489079529908));
#18330=CARTESIAN_POINT('Ctrl Pts',(-23.758791421472,21.1536058158449,177.387454832855));
#18331=CARTESIAN_POINT('Ctrl Pts',(-23.71621735197,21.1589727501825,177.185140312999));
#18332=CARTESIAN_POINT('Ctrl Pts',(-23.7058175952175,21.1602837550329,177.085486338622));
#18333=CARTESIAN_POINT('Ctrl Pts',(-23.70581759522,21.1602837550326,176.985485069079));
#18334=CARTESIAN_POINT('Origin',(-53.4413942236179,-112.716773792997,173.485485069079));
#18335=CARTESIAN_POINT('',(-41.1490507210046,24.0009423880185,173.485485069079));
#18336=CARTESIAN_POINT('',(-55.4013296080738,22.2042843320105,173.485485069079));
#18337=CARTESIAN_POINT('',(-41.1020539958444,25.42062214227,173.485485069079));
#18338=CARTESIAN_POINT('Origin',(-36.6843857876575,24.5637629925993,173.485485069079));
#18339=CARTESIAN_POINT('',(-37.1738630900728,31.4290895869696,173.485485069079));
#18340=CARTESIAN_POINT('Origin',(-31.7758655563387,23.6116972707429,173.485485069079));
#18341=CARTESIAN_POINT('Origin',(-44.1060283439209,41.4682670878081,173.485485069079));
#18342=CARTESIAN_POINT('',(-7.55021677450188,-106.931681155043,173.485485069079));
#18343=CARTESIAN_POINT('Origin',(-55.4013296080738,22.2042843320105,180.985485069079));
#18344=CARTESIAN_POINT('',(-20.9569943874949,26.5463753651883,174.985485069079));
#18345=CARTESIAN_POINT('',(-24.5594210254598,26.0922494747562,171.485485069079));
#18346=CARTESIAN_POINT('Ctrl Pts',(-20.9569943874949,26.5463753651883,174.985485069079));
#18347=CARTESIAN_POINT('Ctrl Pts',(-20.9569943874949,26.5463753651883,174.886701580263));
#18348=CARTESIAN_POINT('Ctrl Pts',(-20.9613070986962,26.5458317000395,174.788168805464));
#18349=CARTESIAN_POINT('Ctrl Pts',(-20.9698519031794,26.5447545325259,174.690100174553));
#18350=CARTESIAN_POINT('Ctrl Pts',(-20.9784443243535,26.5436713623995,174.591485047383));
#18351=CARTESIAN_POINT('Ctrl Pts',(-20.991316196275,26.5420487199739,174.493338524244));
#18352=CARTESIAN_POINT('Ctrl Pts',(-21.0084374856327,26.5398903912816,174.395878356477));
#18353=CARTESIAN_POINT('Ctrl Pts',(-21.0149108898769,26.5390743467755,174.359029550847));
#18354=CARTESIAN_POINT('Ctrl Pts',(-21.0219922837033,26.5381816584295,174.322278925862));
#18355=CARTESIAN_POINT('Ctrl Pts',(-21.0296819391904,26.5372122919451,174.28563861018));
#18356=CARTESIAN_POINT('Ctrl Pts',(-21.0779351095987,26.5311294438597,174.055717855038));
#18357=CARTESIAN_POINT('Ctrl Pts',(-21.148865448191,26.5221878868457,173.834574324614));
#18358=CARTESIAN_POINT('Ctrl Pts',(-21.2414406256354,26.5105177574819,173.62180845516));
#18359=CARTESIAN_POINT('Ctrl Pts',(-21.3340158030797,26.498847628118,173.409042585707));
#18360=CARTESIAN_POINT('Ctrl Pts',(-21.4500317046224,26.4842225351218,173.202497940917));
#18361=CARTESIAN_POINT('Ctrl Pts',(-21.5836610718905,26.4673770691353,173.012195588691));
#18362=CARTESIAN_POINT('Ctrl Pts',(-21.7172904391586,26.4505316031489,172.821893236465));
#18363=CARTESIAN_POINT('Ctrl Pts',(-21.8682914407053,26.4314962497122,172.646838591098));
#18364=CARTESIAN_POINT('Ctrl Pts',(-22.0362862751098,26.4103186348906,172.486700043083));
#18365=CARTESIAN_POINT('Ctrl Pts',(-22.2042811095142,26.3891410200689,172.326561495067));
#18366=CARTESIAN_POINT('Ctrl Pts',(-22.390389099386,26.365680040815,172.181282504032));
#18367=CARTESIAN_POINT('Ctrl Pts',(-22.5853450510322,26.3411036777037,172.057259029844));
#18368=CARTESIAN_POINT('Ctrl Pts',(-22.7803010026784,26.3165273145925,171.933235555656));
#18369=CARTESIAN_POINT('Ctrl Pts',(-22.985880824076,26.290611694698,171.828488317195));
#18370=CARTESIAN_POINT('Ctrl Pts',(-23.2021330341362,26.2633507016728,171.743105349009));
#18371=CARTESIAN_POINT('Ctrl Pts',(-23.4183852441963,26.2360897086476,171.657722380822));
#18372=CARTESIAN_POINT('Ctrl Pts',(-23.6431960794103,26.2077498058597,171.593014493226));
#18373=CARTESIAN_POINT('Ctrl Pts',(-23.8695731252959,26.1792124648205,171.550160201754));
#18374=CARTESIAN_POINT('Ctrl Pts',(-24.0959501711816,26.1506751237814,171.507305910282));
#18375=CARTESIAN_POINT('Ctrl Pts',(-24.325855444624,26.1216930104701,171.485485069079));
#18376=CARTESIAN_POINT('Ctrl Pts',(-24.5594210254598,26.0922494747562,171.485485069079));
#18377=CARTESIAN_POINT('',(-55.4013296080738,22.2042843320105,171.485485069079));
#18378=CARTESIAN_POINT('Origin',(-41.1490507210046,24.0009423880185,173.985485069079));
#18379=CARTESIAN_POINT('',(-21.3209582807514,26.5004936738394,178.485485069079));
#18380=CARTESIAN_POINT('',(-41.1490507210046,24.0009423880185,178.485485069079));
#18381=CARTESIAN_POINT('',(-55.4013296080738,22.2042843320105,178.485485069079));
#18382=CARTESIAN_POINT('Origin',(-41.1490507210046,24.0009423880185,177.985485069079));
#18383=CARTESIAN_POINT('',(-24.559421025453,26.0922494747571,180.485485069079));
#18384=CARTESIAN_POINT('',(-24.4216473560585,26.109617376058,180.485485069079));
#18385=CARTESIAN_POINT('',(-20.9569943874949,26.5463753651883,176.985485069079));
#18386=CARTESIAN_POINT('Ctrl Pts',(-24.559421025453,26.0922494747571,180.485485069079));
#18387=CARTESIAN_POINT('Ctrl Pts',(-24.4824800351446,26.1019487411811,180.485485069079));
#18388=CARTESIAN_POINT('Ctrl Pts',(-24.4058343548432,26.1116107822155,180.48308261772));
#18389=CARTESIAN_POINT('Ctrl Pts',(-24.3294786223864,26.1212362572639,180.47833836426));
#18390=CARTESIAN_POINT('Ctrl Pts',(-24.2518299481371,26.1310247217639,180.473513775724));
#18391=CARTESIAN_POINT('Ctrl Pts',(-24.1744804020117,26.1407754583192,180.466267294623));
#18392=CARTESIAN_POINT('Ctrl Pts',(-24.0974265496722,26.1504889123961,180.456608401495));
#18393=CARTESIAN_POINT('Ctrl Pts',(-24.0203726973327,26.160202366473,180.446949508367));
#18394=CARTESIAN_POINT('Ctrl Pts',(-23.9436138073681,26.1698786341731,180.434877975413));
#18395=CARTESIAN_POINT('Ctrl Pts',(-23.8671595938527,26.1795165367008,180.420352216777));
#18396=CARTESIAN_POINT('Ctrl Pts',(-23.7777409465118,26.1907887500636,180.40336330761));
#18397=CARTESIAN_POINT('Ctrl Pts',(-23.6887478791473,26.202007371553,180.383010105823));
#18398=CARTESIAN_POINT('Ctrl Pts',(-23.600672382606,26.2131103107849,180.359405636771));
#18399=CARTESIAN_POINT('Ctrl Pts',(-23.5135638682412,26.2240913506831,180.336060321533));
#18400=CARTESIAN_POINT('Ctrl Pts',(-23.4273536194521,26.2349591363698,180.309535144864));
#18401=CARTESIAN_POINT('Ctrl Pts',(-23.3424927384906,26.2456567990874,180.279983354262));
#18402=CARTESIAN_POINT('Ctrl Pts',(-23.294289980915,26.2517332955456,180.263197318314));
#18403=CARTESIAN_POINT('Ctrl Pts',(-23.2465220763462,26.2577549698662,180.245435520943));
#18404=CARTESIAN_POINT('Ctrl Pts',(-23.1992667660851,26.2637120265967,180.226731704473));
#18405=CARTESIAN_POINT('Ctrl Pts',(-22.9847021376151,26.2907602812183,180.141806276839));
#18406=CARTESIAN_POINT('Ctrl Pts',(-22.7786882935836,26.3167306144865,180.037038838794));
#18407=CARTESIAN_POINT('Ctrl Pts',(-22.5816792108732,26.3415657975729,179.911375942728));
#18408=CARTESIAN_POINT('Ctrl Pts',(-22.3846701281627,26.3664009806592,179.785713046663));
#18409=CARTESIAN_POINT('Ctrl Pts',(-22.2017889982585,26.389455178373,179.642261663978));
#18410=CARTESIAN_POINT('Ctrl Pts',(-22.0344375412165,26.410551688332,179.482506548126));
#18411=CARTESIAN_POINT('Ctrl Pts',(-21.8670860841744,26.431648198291,179.322751432275));
#18412=CARTESIAN_POINT('Ctrl Pts',(-21.7133004196351,26.4510345894276,179.144165737668));
#18413=CARTESIAN_POINT('Ctrl Pts',(-21.5797898545736,26.4678650790763,178.953250199313));
#18414=CARTESIAN_POINT('Ctrl Pts',(-21.4462792895122,26.4846955687251,178.762334660957));
#18415=CARTESIAN_POINT('Ctrl Pts',(-21.3330091361679,26.4989745296635,178.560114310074));
#18416=CARTESIAN_POINT('Ctrl Pts',(-21.2402555850145,26.5106671450146,178.346434887201));
#18417=CARTESIAN_POINT('Ctrl Pts',(-21.147502033861,26.5223597603657,178.132755464328));
#18418=CARTESIAN_POINT('Ctrl Pts',(-21.0757990733503,26.5313987149541,177.906973211641));
#18419=CARTESIAN_POINT('Ctrl Pts',(-21.0284937221365,26.5373620799025,177.679645756147));
#18420=CARTESIAN_POINT('Ctrl Pts',(-20.9811883709227,26.5433254448509,177.452318300652));
#18421=CARTESIAN_POINT('Ctrl Pts',(-20.9569943874949,26.5463753651884,177.220993816469));
#18422=CARTESIAN_POINT('Ctrl Pts',(-20.9569943874949,26.5463753651884,176.985485069079));
#18423=CARTESIAN_POINT('',(-20.9569943874949,26.5463753651883,180.985485069079));
#18424=CARTESIAN_POINT('Origin',(-52.9434576820456,-13.7117130172939,180.985485069079));
#18425=CARTESIAN_POINT('',(-53.0330559861815,-12.4024452642559,171.485485069079));
#18426=CARTESIAN_POINT('',(-52.9434576820456,-13.7117130172939,171.485485069079));
#18427=CARTESIAN_POINT('',(-53.0330559861815,-12.4024452642559,173.485485069079));
#18428=CARTESIAN_POINT('',(-53.0330559861815,-12.4024452642559,180.985485069079));
#18429=CARTESIAN_POINT('',(-52.9434576820456,-13.7117130172939,173.485485069079));
#18430=CARTESIAN_POINT('Origin',(-63.3850491201885,-111.656713748515,180.985485069079));
#18431=CARTESIAN_POINT('',(-53.082572536869,-15.0166486334899,173.485485069079));
#18432=CARTESIAN_POINT('',(-53.082572536869,-15.0166486334899,171.485485069079));
#18433=CARTESIAN_POINT('',(-53.082572536869,-15.0166486334899,170.985485069079));
#18434=CARTESIAN_POINT('',(-63.3850491201885,-111.656713748515,171.485485069079));
#18435=CARTESIAN_POINT('',(-63.3850491201885,-111.656713748515,171.485485069079));
#18436=CARTESIAN_POINT('',(-63.3850491201885,-111.656713748515,173.485485069079));
#18437=CARTESIAN_POINT('',(-63.3850491201885,-111.656713748515,180.985485069079));
#18438=CARTESIAN_POINT('',(-63.3850491201885,-111.656713748515,173.485485069079));
#18439=CARTESIAN_POINT('Origin',(-53.4413942236179,-112.716773792997,180.985485069079));
#18440=CARTESIAN_POINT('',(-57.0153382075497,-112.335767487168,173.541420416595));
#18441=CARTESIAN_POINT('',(-60.8888270505344,-111.922827698136,172.515418850865));
#18442=CARTESIAN_POINT('Ctrl Pts',(-57.0153382075498,-112.335767487168,
173.541420416595));
#18443=CARTESIAN_POINT('Ctrl Pts',(-57.2280258358028,-112.313093565052,
173.272225027772));
#18444=CARTESIAN_POINT('Ctrl Pts',(-57.4821106107221,-112.286006430532,
173.039327830791));
#18445=CARTESIAN_POINT('Ctrl Pts',(-58.0784446078591,-112.222433242393,
172.646611798095));
#18446=CARTESIAN_POINT('Ctrl Pts',(-58.4215062269221,-112.185860581843,
172.497875229972));
#18447=CARTESIAN_POINT('Ctrl Pts',(-58.9537897151705,-112.129115605866,
172.368671149366));
#18448=CARTESIAN_POINT('Ctrl Pts',(-59.1339560066465,-112.109908675522,
172.340024858843));
#18449=CARTESIAN_POINT('Ctrl Pts',(-59.5707164861963,-112.063347090452,
172.299854718465));
#18450=CARTESIAN_POINT('Ctrl Pts',(-59.8357943853675,-112.035088015443,
172.303335717215));
#18451=CARTESIAN_POINT('Ctrl Pts',(-60.3675672608762,-111.978397474195,
172.366333772718));
#18452=CARTESIAN_POINT('Ctrl Pts',(-60.6324827847851,-111.950155709474,
172.427035584321));
#18453=CARTESIAN_POINT('Ctrl Pts',(-60.8888270505344,-111.922827698136,
172.515418850865));
#18454=CARTESIAN_POINT('',(-62.0210982548684,-111.80212002317,173.485485069079));
#18455=CARTESIAN_POINT('Ctrl Pts',(-60.8888270505344,-111.922827698136,
172.515418850865));
#18456=CARTESIAN_POINT('Ctrl Pts',(-61.1058388649012,-111.899692788891,
172.639451350805));
#18457=CARTESIAN_POINT('Ctrl Pts',(-61.310701839086,-111.877853027175,172.783834155405));
#18458=CARTESIAN_POINT('Ctrl Pts',(-61.6906606007499,-111.837346884718,
173.109414086522));
#18459=CARTESIAN_POINT('Ctrl Pts',(-61.8649365864974,-111.818767900318,
173.289924177764));
#18460=CARTESIAN_POINT('Ctrl Pts',(-62.0210982548684,-111.80212002317,173.485485069079));
#18461=CARTESIAN_POINT('',(-53.4413942236179,-112.716773792997,173.485485069079));
#18462=CARTESIAN_POINT('',(-62.88786637536,-111.709716750739,170.985485069079));
#18463=CARTESIAN_POINT('Origin',(-62.88786637536,-111.709716750739,171.485485069079));
#18464=CARTESIAN_POINT('',(-57.4188561822461,-112.292749775204,170.985485069079));
#18465=CARTESIAN_POINT('',(-53.4413942236179,-112.716773792997,170.985485069079));
#18466=CARTESIAN_POINT('',(-53.4413942236179,-112.716773792997,174.985485069079));
#18467=CARTESIAN_POINT('Origin',(-57.4188561822461,-112.292749775204,174.985485069079));
#18468=CARTESIAN_POINT('',(-53.4413942236179,-112.716773792997,176.985485069079));
#18469=CARTESIAN_POINT('',(-53.4413942236179,-112.716773792997,180.985485069079));
#18470=CARTESIAN_POINT('',(-57.4188561822461,-112.292749775204,180.985485069079));
#18471=CARTESIAN_POINT('Origin',(-57.4188561822461,-112.292749775204,176.985485069079));
#18472=CARTESIAN_POINT('',(-62.88786637536,-111.709716750739,180.985485069079));
#18473=CARTESIAN_POINT('',(-53.4413942236179,-112.716773792997,180.985485069079));
#18474=CARTESIAN_POINT('',(-63.3850491201885,-111.656713748515,180.485485069079));
#18475=CARTESIAN_POINT('Origin',(-62.88786637536,-111.709716750739,180.485485069079));
#18476=CARTESIAN_POINT('',(-63.3850491201885,-111.656713748515,178.985485069079));
#18477=CARTESIAN_POINT('',(-63.3850491201885,-111.656713748515,180.985485069079));
#18478=CARTESIAN_POINT('Origin',(-62.88786637536,-111.709716750739,178.985485069079));
#18479=CARTESIAN_POINT('',(-60.8888270454861,-111.922827698674,179.455551290205));
#18480=CARTESIAN_POINT('Ctrl Pts',(-62.0210982548537,-111.802120023171,
178.485485069079));
#18481=CARTESIAN_POINT('Ctrl Pts',(-61.8656334742916,-111.818693607423,
178.680173249399));
#18482=CARTESIAN_POINT('Ctrl Pts',(-61.6922139029917,-111.837181292321,
178.859946907849));
#18483=CARTESIAN_POINT('Ctrl Pts',(-61.3125284291585,-111.87765830047,179.185847773914));
#18484=CARTESIAN_POINT('Ctrl Pts',(-61.1068076160046,-111.899589513552,
179.330965100789));
#18485=CARTESIAN_POINT('Ctrl Pts',(-60.8888270454861,-111.922827698674,
179.455551290205));
#18486=CARTESIAN_POINT('',(-57.0153371209007,-112.335767603012,178.42954834513));
#18487=CARTESIAN_POINT('Ctrl Pts',(-60.888827045486,-111.922827698674,179.455551290205));
#18488=CARTESIAN_POINT('Ctrl Pts',(-60.6328315485644,-111.950118528925,
179.543814307164));
#18489=CARTESIAN_POINT('Ctrl Pts',(-60.3682870318124,-111.978320741804,
179.604471510014));
#18490=CARTESIAN_POINT('Ctrl Pts',(-59.8372616671249,-112.034931593404,
179.667537944491));
#18491=CARTESIAN_POINT('Ctrl Pts',(-59.5725535707745,-112.063151244962,
179.671129691791));
#18492=CARTESIAN_POINT('Ctrl Pts',(-59.136191489744,-112.109670358089,179.631251769103));
#18493=CARTESIAN_POINT('Ctrl Pts',(-58.956303432779,-112.128847626775,179.602744942888));
#18494=CARTESIAN_POINT('Ctrl Pts',(-58.4237297979111,-112.18562353432,179.473976739277));
#18495=CARTESIAN_POINT('Ctrl Pts',(-58.0800579015758,-112.222261254505,
179.325242151835));
#18496=CARTESIAN_POINT('Ctrl Pts',(-57.4827491337447,-112.285938359712,
178.932226803426));
#18497=CARTESIAN_POINT('Ctrl Pts',(-57.228292602565,-112.313065125933,178.699083057342));
#18498=CARTESIAN_POINT('Ctrl Pts',(-57.0153371209008,-112.335767603012,
178.42954834513));
#18499=CARTESIAN_POINT('',(-55.9273125369417,-112.451758292321,176.985485069089));
#18500=CARTESIAN_POINT('Origin',(-57.4188631216847,-112.292749035413,176.985488314375));
#18501=CARTESIAN_POINT('',(-55.9273079477605,-112.451758781876,174.985485069079));
#18502=CARTESIAN_POINT('',(-55.9273079477605,-112.451758781876,176.985485069079));
#18503=CARTESIAN_POINT('Origin',(-57.4188561822461,-112.292749775204,174.985485069079));
#18504=CARTESIAN_POINT('Origin',(-67.998054881725,-13.4265585667677,180.985485069079));
#18505=CARTESIAN_POINT('',(-53.0330559861815,-12.4024452642559,178.985485069079));
#18506=CARTESIAN_POINT('',(-53.0330559861815,-12.4024452642559,180.485485069079));
#18507=CARTESIAN_POINT('',(-53.0330559861815,-12.4024452642559,180.985485069079));
#18508=CARTESIAN_POINT('',(-53.082572536869,-15.0166486334899,178.985485069079));
#18509=CARTESIAN_POINT('Origin',(-67.998054881725,-13.4265585667677,178.985485069079));
#18510=CARTESIAN_POINT('',(-53.082572536869,-15.0166486334899,180.485485069079));
#18511=CARTESIAN_POINT('',(-53.082572536869,-15.0166486334899,170.985485069079));
#18512=CARTESIAN_POINT('Origin',(-67.998054881725,-13.4265585667677,180.485485069079));
#18513=CARTESIAN_POINT('Ctrl Pts',(-53.4413942236179,-112.716773792997,
176.985485069079));
#18514=CARTESIAN_POINT('Ctrl Pts',(-53.4413942236179,-112.716773792997,
174.585485069079));
#18515=CARTESIAN_POINT('Ctrl Pts',(-42.7208173800685,-12.1548131952256,
176.985485069079));
#18516=CARTESIAN_POINT('Ctrl Pts',(-42.7208173800685,-12.1548131952256,
174.585485069079));
#18517=CARTESIAN_POINT('Ctrl Pts',(-26.1502242325394,-14.6226249149956,
176.985485069079));
#18518=CARTESIAN_POINT('Ctrl Pts',(-26.1502242325394,-14.6226249149956,
174.585485069079));
#18519=CARTESIAN_POINT('Ctrl Pts',(-20.3993997473094,25.9801832318931,176.985485069079));
#18520=CARTESIAN_POINT('Ctrl Pts',(-20.3993997473094,25.9801832318931,174.585485069079));
#18521=CARTESIAN_POINT('',(-20.3993997459831,25.9801832412571,174.985485069079));
#18522=CARTESIAN_POINT('Ctrl Pts',(-53.4413942236179,-112.716773792997,
174.985485069079));
#18523=CARTESIAN_POINT('Ctrl Pts',(-52.8096223112116,-106.790579420312,
174.985485069079));
#18524=CARTESIAN_POINT('Ctrl Pts',(-52.1206641754933,-100.87124426812,174.98548506908));
#18525=CARTESIAN_POINT('Ctrl Pts',(-50.5942726079286,-89.0503828822984,
174.98548506908));
#18526=CARTESIAN_POINT('Ctrl Pts',(-49.757265425744,-83.1507260725826,174.985485069079));
#18527=CARTESIAN_POINT('Ctrl Pts',(-47.888174002584,-71.4000958425799,174.985485069079));
#18528=CARTESIAN_POINT('Ctrl Pts',(-46.8562222321137,-65.5467331693134,
174.985485069079));
#18529=CARTESIAN_POINT('Ctrl Pts',(-44.5210591976856,-53.901141681327,174.985485069079));
#18530=CARTESIAN_POINT('Ctrl Pts',(-43.2178767803996,-48.1089063654215,
174.985485069079));
#18531=CARTESIAN_POINT('Ctrl Pts',(-40.9750678687189,-39.4854680169988,
174.985485069079));
#18532=CARTESIAN_POINT('Ctrl Pts',(-40.1790492411628,-36.6219000231504,
174.985485069079));
#18533=CARTESIAN_POINT('Ctrl Pts',(-38.4756477469119,-30.9198622377508,
174.985485069079));
#18534=CARTESIAN_POINT('Ctrl Pts',(-37.5677629527721,-28.0815055657851,
174.985485069079));
#18535=CARTESIAN_POINT('Ctrl Pts',(-35.6349943284908,-22.4311603405326,
174.985485069079));
#18536=CARTESIAN_POINT('Ctrl Pts',(-34.608328317987,-19.6177595316176,174.985485069079));
#18537=CARTESIAN_POINT('Ctrl Pts',(-32.4706666932395,-14.0256929237095,
174.985485069079));
#18538=CARTESIAN_POINT('Ctrl Pts',(-31.3585525008225,-11.2457550461466,
174.985485069079));
#18539=CARTESIAN_POINT('Ctrl Pts',(-29.1380236708638,-5.6845035686739,174.985485069079));
#18540=CARTESIAN_POINT('Ctrl Pts',(-28.0318787018384,-2.90234596622778,
174.985485069079));
#18541=CARTESIAN_POINT('Ctrl Pts',(-25.959804002289,2.7141098997671,174.985485069079));
#18542=CARTESIAN_POINT('Ctrl Pts',(-24.9969151286383,5.54953894117839,174.985485069079));
#18543=CARTESIAN_POINT('Ctrl Pts',(-23.2984117431506,11.3049116288563,174.985485069079));
#18544=CARTESIAN_POINT('Ctrl Pts',(-22.5666401222046,14.2084908208118,174.985485069079));
#18545=CARTESIAN_POINT('Ctrl Pts',(-21.3283637469275,20.0618248638162,174.985485069079));
#18546=CARTESIAN_POINT('Ctrl Pts',(-20.8198378348718,23.0117450437847,174.985485069079));
#18547=CARTESIAN_POINT('Ctrl Pts',(-20.3993997459139,25.9801832417458,174.985485069079));
#18548=CARTESIAN_POINT('',(-20.399399745983,25.9801832412581,176.985485069079));
#18549=CARTESIAN_POINT('',(-20.3993997459139,25.9801832417458,174.985485069079));
#18550=CARTESIAN_POINT('Ctrl Pts',(-20.3993997459139,25.9801832417458,176.985485069079));
#18551=CARTESIAN_POINT('Ctrl Pts',(-20.8194918499154,23.0141878171383,176.985485069079));
#18552=CARTESIAN_POINT('Ctrl Pts',(-21.32754882053,20.0665006828847,176.985485069079));
#18553=CARTESIAN_POINT('Ctrl Pts',(-22.2553679339636,15.6794644341189,176.985485069079));
#18554=CARTESIAN_POINT('Ctrl Pts',(-22.5922397393381,14.2228632003925,176.985485069079));
#18555=CARTESIAN_POINT('Ctrl Pts',(-23.3244477728418,11.3218290413609,176.985485069079));
#18556=CARTESIAN_POINT('Ctrl Pts',(-23.7201299995547,9.87649782832845,176.985485069079));
#18557=CARTESIAN_POINT('Ctrl Pts',(-24.9920882209669,5.56474808425753,176.985485069079));
#18558=CARTESIAN_POINT('Ctrl Pts',(-25.9534941549082,2.73229051813628,176.985485069079));
#18559=CARTESIAN_POINT('Ctrl Pts',(-28.0226448730915,-2.87838666024527,
176.985485069079));
#18560=CARTESIAN_POINT('Ctrl Pts',(-29.1273699516833,-5.65772547397114,
176.985485069079));
#18561=CARTESIAN_POINT('Ctrl Pts',(-31.3455088620405,-11.2131827659292,
176.985485069079));
#18562=CARTESIAN_POINT('Ctrl Pts',(-32.4566496657803,-13.9901437025305,
176.985485069079));
#18563=CARTESIAN_POINT('Ctrl Pts',(-34.5927847123162,-19.5759943027127,
176.985485069079));
#18564=CARTESIAN_POINT('Ctrl Pts',(-35.6188539822851,-22.3860236816944,
176.985485069079));
#18565=CARTESIAN_POINT('Ctrl Pts',(-37.5513960609844,-28.0316432492908,
176.985485069079));
#18566=CARTESIAN_POINT('Ctrl Pts',(-38.4595477409101,-30.8684137262953,
176.985485069079));
#18567=CARTESIAN_POINT('Ctrl Pts',(-40.1639162339715,-36.5688422501229,
176.985485069079));
#18568=CARTESIAN_POINT('Ctrl Pts',(-40.9606327724711,-39.4323802592758,
176.98548506908));
#18569=CARTESIAN_POINT('Ctrl Pts',(-43.2058271638625,-48.0578135867489,
176.985485069079));
#18570=CARTESIAN_POINT('Ctrl Pts',(-44.5109607325329,-53.8541412455957,
176.98548506908));
#18571=CARTESIAN_POINT('Ctrl Pts',(-46.8499201547131,-65.5119666514209,
176.98548506908));
#18572=CARTESIAN_POINT('Ctrl Pts',(-47.8837400389295,-71.3734658322673,
176.98548506908));
#18573=CARTESIAN_POINT('Ctrl Pts',(-49.7562860675246,-83.1433271304293,
176.98548506908));
#18574=CARTESIAN_POINT('Ctrl Pts',(-50.5938605211195,-89.0473685697446,
176.985485069079));
#18575=CARTESIAN_POINT('Ctrl Pts',(-52.120387756833,-100.868926655335,176.985485069079));
#18576=CARTESIAN_POINT('Ctrl Pts',(-52.8094746128609,-106.789193969142,
176.985485069079));
#18577=CARTESIAN_POINT('Ctrl Pts',(-53.4413942236179,-112.716773792997,
176.985485069079));
#18578=CARTESIAN_POINT('Origin',(-52.9434576820456,-13.7117130172939,180.985485069079));
#18579=CARTESIAN_POINT('',(-52.9434576820456,-13.7117130172939,178.985485069079));
#18580=CARTESIAN_POINT('',(-54.4340581561246,8.06989492938438,180.485485069079));
#18581=CARTESIAN_POINT('Origin',(-63.3850491201885,-111.656713748515,180.985485069079));
#18582=CARTESIAN_POINT('',(-63.3850491201885,-111.656713748515,178.985485069079));
#18583=CARTESIAN_POINT('',(-53.082572536869,-15.0166486334899,180.485485069079));
#18584=CARTESIAN_POINT('Origin',(-34.9583934096621,-20.6140499623174,180.985485069079));
#18585=CARTESIAN_POINT('',(-24.4968853993556,25.596175592946,180.985485069079));
#18586=CARTESIAN_POINT('Ctrl Pts',(-57.4188561822461,-112.292749775204,
180.985485069079));
#18587=CARTESIAN_POINT('Ctrl Pts',(-56.790512649408,-106.398714547387,180.985485069079));
#18588=CARTESIAN_POINT('Ctrl Pts',(-56.1058731125984,-100.511880940133,
180.98548506906));
#18589=CARTESIAN_POINT('Ctrl Pts',(-55.3484913384761,-94.6343530226705,
180.985485069073));
#18590=CARTESIAN_POINT('Ctrl Pts',(-55.338924151294,-94.5601085508923,180.985485069073));
#18591=CARTESIAN_POINT('Ctrl Pts',(-55.3293453578738,-94.4858656122032,
180.985485069073));
#18592=CARTESIAN_POINT('Ctrl Pts',(-55.3197549249144,-94.4116242090743,
180.985485069073));
#18593=CARTESIAN_POINT('Ctrl Pts',(-54.9352546151986,-91.4351326765513,
180.985485069079));
#18594=CARTESIAN_POINT('Ctrl Pts',(-54.5319470084521,-88.4611202257547,
180.985485069078));
#18595=CARTESIAN_POINT('Ctrl Pts',(-54.1069203483626,-85.4898333910159,
180.985485069077));
#18596=CARTESIAN_POINT('Ctrl Pts',(-53.7033042231981,-82.6682238507177,
180.985485069076));
#18597=CARTESIAN_POINT('Ctrl Pts',(-53.2799637223225,-79.8481667017225,
180.985485069075));
#18598=CARTESIAN_POINT('Ctrl Pts',(-52.8343681747547,-77.0334451025294,
180.985485069077));
#18599=CARTESIAN_POINT('Ctrl Pts',(-52.8106597636878,-76.8836846817239,
180.985485069077));
#18600=CARTESIAN_POINT('Ctrl Pts',(-52.7868882204028,-76.7339390343581,
180.985485069077));
#18601=CARTESIAN_POINT('Ctrl Pts',(-52.7630531680916,-76.5842087401903,
180.985485069077));
#18602=CARTESIAN_POINT('Ctrl Pts',(-51.8554066519163,-70.8824306155612,
180.985485069076));
#18603=CARTESIAN_POINT('Ctrl Pts',(-50.8566834398535,-65.2025739806144,
180.985485068139));
#18604=CARTESIAN_POINT('Ctrl Pts',(-49.7333492755762,-59.5526619928141,
180.985485068761));
#18605=CARTESIAN_POINT('Ctrl Pts',(-49.6887622529058,-59.3284074816482,
180.985485068785));
#18606=CARTESIAN_POINT('Ctrl Pts',(-49.643978469431,-59.1042002714389,180.985485068806));
#18607=CARTESIAN_POINT('Ctrl Pts',(-49.5989958321339,-58.8800408668684,
180.985485068823));
#18608=CARTESIAN_POINT('Ctrl Pts',(-48.480916301155,-53.3083790660962,180.985485069247));
#18609=CARTESIAN_POINT('Ctrl Pts',(-47.2399537491611,-47.7662638000103,
180.985485068065));
#18610=CARTESIAN_POINT('Ctrl Pts',(-45.8293087716645,-42.2649422848648,
180.985485068732));
#18611=CARTESIAN_POINT('Ctrl Pts',(-45.7533507434525,-41.9687164154809,
180.985485068768));
#18612=CARTESIAN_POINT('Ctrl Pts',(-45.6769001981415,-41.6726090103213,
180.985485068799));
#18613=CARTESIAN_POINT('Ctrl Pts',(-45.5999497834957,-41.3766218285166,
180.985485068827));
#18614=CARTESIAN_POINT('Ctrl Pts',(-44.8469362038317,-38.4801804210025,
180.985485069096));
#18615=CARTESIAN_POINT('Ctrl Pts',(-44.0456768427767,-35.5953424896882,
180.985485069068));
#18616=CARTESIAN_POINT('Ctrl Pts',(-43.1891752015397,-32.7237825622821,
180.985485069046));
#18617=CARTESIAN_POINT('Ctrl Pts',(-42.4423310849265,-30.2198671766812,
180.985485069027));
#18618=CARTESIAN_POINT('Ctrl Pts',(-41.6531322686351,-27.7261321945819,
180.985485069014));
#18619=CARTESIAN_POINT('Ctrl Pts',(-40.8200495521006,-25.2429405912916,
180.985485068515));
#18620=CARTESIAN_POINT('Ctrl Pts',(-40.6977329751789,-24.8783483476563,
180.985485068442));
#18621=CARTESIAN_POINT('Ctrl Pts',(-40.5744720942236,-24.5139805152869,
180.985485068402));
#18622=CARTESIAN_POINT('Ctrl Pts',(-40.4502615514014,-24.1498393561786,
180.98548506839));
#18623=CARTESIAN_POINT('Ctrl Pts',(-39.616810792004,-21.7064579918356,180.985485068307));
#18624=CARTESIAN_POINT('Ctrl Pts',(-38.739353495722,-19.2722820499251,180.985485070954));
#18625=CARTESIAN_POINT('Ctrl Pts',(-37.8282880086107,-16.8505834688252,
180.985485066549));
#18626=CARTESIAN_POINT('Ctrl Pts',(-37.6788085609924,-16.4532529022283,
180.985485065826));
#18627=CARTESIAN_POINT('Ctrl Pts',(-37.5284339691997,-16.056244665969,180.985485065289));
#18628=CARTESIAN_POINT('Ctrl Pts',(-37.3772084254297,-15.6595731913905,
180.985485065039));
#18629=CARTESIAN_POINT('Ctrl Pts',(-36.4693625270572,-13.2782521379502,
180.985485063537));
#18630=CARTESIAN_POINT('Ctrl Pts',(-35.5299993620731,-10.9085007698185,
180.985485072686));
#18631=CARTESIAN_POINT('Ctrl Pts',(-34.5852825795174,-8.54078321761435,
180.985485064032));
#18632=CARTESIAN_POINT('Ctrl Pts',(-34.4134917762452,-8.11022867711563,
180.985485062458));
#18633=CARTESIAN_POINT('Ctrl Pts',(-34.2415483012594,-7.67973099356383,
180.985485061337));
#18634=CARTESIAN_POINT('Ctrl Pts',(-34.0696087116074,-7.24923200405654,
180.98548506096));
#18635=CARTESIAN_POINT('Ctrl Pts',(-33.138509657603,-4.91796436120965,180.985485058921));
#18636=CARTESIAN_POINT('Ctrl Pts',(-32.2088990960437,-2.58615052122322,
180.985485069115));
#18637=CARTESIAN_POINT('Ctrl Pts',(-31.3204104332397,-0.23907854190687,
180.985485069028));
#18638=CARTESIAN_POINT('Ctrl Pts',(-31.1425632790713,0.230730572857145,
180.985485069011));
#18639=CARTESIAN_POINT('Ctrl Pts',(-30.9663469447662,0.701142876122788,
180.985485068984));
#18640=CARTESIAN_POINT('Ctrl Pts',(-30.7920966781887,1.17228422073675,180.985485067611));
#18641=CARTESIAN_POINT('Ctrl Pts',(-30.2848140693334,2.54388505171172,180.985485063616));
#18642=CARTESIAN_POINT('Ctrl Pts',(-29.7950938569279,3.9220018739976,180.985485032927));
#18643=CARTESIAN_POINT('Ctrl Pts',(-29.3283958544553,5.30867284540019,180.985485020463));
#18644=CARTESIAN_POINT('Ctrl Pts',(-29.006637155384,6.26469460987012,180.985485011869));
#18645=CARTESIAN_POINT('Ctrl Pts',(-28.6958217757076,7.22478169314873,180.985485026902));
#18646=CARTESIAN_POINT('Ctrl Pts',(-28.3977441390982,8.18958797408848,180.985485051181));
#18647=CARTESIAN_POINT('Ctrl Pts',(-28.2377424180365,8.70747541843852,180.985485064214));
#18648=CARTESIAN_POINT('Ctrl Pts',(-28.0812847212611,9.22671577439412,180.985485065958));
#18649=CARTESIAN_POINT('Ctrl Pts',(-27.9286546962701,9.74743161800556,180.985485067269));
#18650=CARTESIAN_POINT('Ctrl Pts',(-27.6620631180387,10.6569411235348,180.985485069558));
#18651=CARTESIAN_POINT('Ctrl Pts',(-27.4072505288242,11.5694243155145,180.98548506854));
#18652=CARTESIAN_POINT('Ctrl Pts',(-27.1645811034528,12.4843659981785,180.985485068803));
#18653=CARTESIAN_POINT('Ctrl Pts',(-27.0208715104168,13.0261973255743,180.985485068958));
#18654=CARTESIAN_POINT('Ctrl Pts',(-26.8813686318622,13.5689896620425,180.985485068973));
#18655=CARTESIAN_POINT('Ctrl Pts',(-26.7461389996539,14.1125915128495,180.985485068982));
#18656=CARTESIAN_POINT('Ctrl Pts',(-26.5222826941656,15.01245864989,180.985485068997));
#18657=CARTESIAN_POINT('Ctrl Pts',(-26.3100078534052,15.9148533438117,180.985485068952));
#18658=CARTESIAN_POINT('Ctrl Pts',(-26.1088919070564,16.8196034741691,180.985485069001));
#18659=CARTESIAN_POINT('Ctrl Pts',(-25.9838202837391,17.3822568567309,180.985485069031));
#18660=CARTESIAN_POINT('Ctrl Pts',(-25.8630558838012,17.9458267556442,180.985485069048));
#18661=CARTESIAN_POINT('Ctrl Pts',(-25.7464863690264,18.5102872637228,180.985485069058));
#18662=CARTESIAN_POINT('Ctrl Pts',(-25.4428718519307,19.9804692826755,180.985485069085));
#18663=CARTESIAN_POINT('Ctrl Pts',(-25.1676456839084,21.4566808478938,180.985485069079));
#18664=CARTESIAN_POINT('Ctrl Pts',(-24.9177905698878,22.9382808324062,180.985485069079));
#18665=CARTESIAN_POINT('Ctrl Pts',(-24.7929746613216,23.6784187676397,180.98548506908));
#18666=CARTESIAN_POINT('Ctrl Pts',(-24.6744808830026,24.4198997434739,180.985485069079));
#18667=CARTESIAN_POINT('Ctrl Pts',(-24.5619054245002,25.1626388829568,180.985485069079));
#18668=CARTESIAN_POINT('Ctrl Pts',(-24.5400091817329,25.3071037310443,180.985485069079));
#18669=CARTESIAN_POINT('Ctrl Pts',(-24.5183368251832,25.4516161749795,180.985485069079));
#18670=CARTESIAN_POINT('Ctrl Pts',(-24.4968853949886,25.5961755921264,180.985485069079));
#18671=CARTESIAN_POINT('',(-41.2825923197859,23.4801507949034,180.985485069079));
#18672=CARTESIAN_POINT('',(-41.2825923197859,23.4801507949034,180.985485069079));
#18673=CARTESIAN_POINT('',(-53.9352248596064,8.10403203946808,180.985485069079));
#18674=CARTESIAN_POINT('Origin',(-39.4690592605811,9.0940082318961,180.985485069079));
#18675=CARTESIAN_POINT('',(-52.5342226896633,-12.3683081541722,180.985485069079));
#18676=CARTESIAN_POINT('',(-52.5342226896634,-12.3683081541722,180.985485069079));
#18677=CARTESIAN_POINT('',(-52.5853897920404,-15.069651635714,180.985485069079));
#18678=CARTESIAN_POINT('Origin',(-67.998054881725,-13.4265585667677,180.985485069079));
#18679=CARTESIAN_POINT('',(-62.88786637536,-111.709716750739,180.985485069079));
#18680=CARTESIAN_POINT('Origin',(-34.9583934096621,-20.6140499623174,170.985485069079));
#18681=CARTESIAN_POINT('',(-52.5853897920404,-15.069651635714,170.985485069079));
#18682=CARTESIAN_POINT('',(-52.9717383111942,-18.6937070505612,170.985485069079));
#18683=CARTESIAN_POINT('',(-52.5342226896633,-12.3683081541722,170.985485069079));
#18684=CARTESIAN_POINT('Origin',(-67.998054881725,-13.4265585667677,170.985485069079));
#18685=CARTESIAN_POINT('',(-53.9352248596064,8.10403203946808,170.985485069079));
#18686=CARTESIAN_POINT('',(-51.890637311636,-21.772789521366,170.985485069079));
#18687=CARTESIAN_POINT('',(-41.2825923197859,23.4801507949034,170.985485069079));
#18688=CARTESIAN_POINT('Origin',(-39.4690592605811,9.0940082318961,170.985485069079));
#18689=CARTESIAN_POINT('',(-24.4968853993885,25.5961755929473,170.985485069079));
#18690=CARTESIAN_POINT('',(-40.5289338663117,23.5751578139663,170.985485069079));
#18691=CARTESIAN_POINT('Ctrl Pts',(-24.4968853950575,25.5961755921349,170.985485069079));
#18692=CARTESIAN_POINT('Ctrl Pts',(-24.5183775783598,25.4513415431335,170.985485069079));
#18693=CARTESIAN_POINT('Ctrl Pts',(-24.5400914677881,25.3065550532397,170.985485069079));
#18694=CARTESIAN_POINT('Ctrl Pts',(-24.5620299993144,25.1618167559765,170.985485069079));
#18695=CARTESIAN_POINT('Ctrl Pts',(-24.6746763176248,24.4186386501074,170.985485069079));
#18696=CARTESIAN_POINT('Ctrl Pts',(-24.7932455255501,23.6767312043179,170.985485069073));
#18697=CARTESIAN_POINT('Ctrl Pts',(-24.9181365313699,22.9361802250035,170.985485069089));
#18698=CARTESIAN_POINT('Ctrl Pts',(-25.1681453406982,21.4537334517548,170.985485069122));
#18699=CARTESIAN_POINT('Ctrl Pts',(-25.4435247881484,19.9767295764349,170.985485068169));
#18700=CARTESIAN_POINT('Ctrl Pts',(-25.7472506552232,18.5058117725121,170.985485072688));
#18701=CARTESIAN_POINT('Ctrl Pts',(-25.8639593378723,17.9406018322643,170.985485074424));
#18702=CARTESIAN_POINT('Ctrl Pts',(-25.9849446272495,17.3763067468434,170.985485077132));
#18703=CARTESIAN_POINT('Ctrl Pts',(-26.1102556574466,16.8129413020526,170.985485082236));
#18704=CARTESIAN_POINT('Ctrl Pts',(-26.3996867343658,15.5117352779024,170.985485094025));
#18705=CARTESIAN_POINT('Ctrl Pts',(-26.7122276139814,14.2154907367009,170.985485119168));
#18706=CARTESIAN_POINT('Ctrl Pts',(-27.0488579985707,12.9244120340896,170.985485101699));
#18707=CARTESIAN_POINT('Ctrl Pts',(-27.0879359754081,12.7745362476317,170.985485099671));
#18708=CARTESIAN_POINT('Ctrl Pts',(-27.1273385599953,12.6247301299435,170.985485097187));
#18709=CARTESIAN_POINT('Ctrl Pts',(-27.1670672687997,12.4749940432329,170.985485094385));
#18710=CARTESIAN_POINT('Ctrl Pts',(-27.4097208281513,11.560441431352,170.985485077277));
#18711=CARTESIAN_POINT('Ctrl Pts',(-27.6643178615963,10.6485868038839,170.985485072147));
#18712=CARTESIAN_POINT('Ctrl Pts',(-27.9310501337635,9.73907607216142,170.985485072818));
#18713=CARTESIAN_POINT('Ctrl Pts',(-28.0841852446823,9.2169119348693,170.985485073203));
#18714=CARTESIAN_POINT('Ctrl Pts',(-28.2411510909769,8.69623022151272,170.985485073994));
#18715=CARTESIAN_POINT('Ctrl Pts',(-28.4016770094243,8.17685932462075,170.985485087244));
#18716=CARTESIAN_POINT('Ctrl Pts',(-28.8331432557161,6.78087907742721,170.985485122858));
#18717=CARTESIAN_POINT('Ctrl Pts',(-29.2912634424619,5.3947931577226,170.985485123205));
#18718=CARTESIAN_POINT('Ctrl Pts',(-29.770586941813,4.01662412744066,170.985485101063));
#18719=CARTESIAN_POINT('Ctrl Pts',(-30.1035894227145,3.05916281622453,170.98548508568));
#18720=CARTESIAN_POINT('Ctrl Pts',(-30.4468264422819,2.10552126126155,170.985485073463));
#18721=CARTESIAN_POINT('Ctrl Pts',(-30.7984770656628,1.15502342646039,170.985485070612));
#18722=CARTESIAN_POINT('Ctrl Pts',(-30.9733231577022,0.682421301348085,
170.985485069194));
#18723=CARTESIAN_POINT('Ctrl Pts',(-31.15014353561,0.210551172825435,170.985485069155));
#18724=CARTESIAN_POINT('Ctrl Pts',(-31.3286006360414,-0.260715918856281,
170.985485069136));
#18725=CARTESIAN_POINT('Ctrl Pts',(-32.2178889544888,-2.60913645515496,
170.98548506904));
#18726=CARTESIAN_POINT('Ctrl Pts',(-33.1482064936523,-4.9422839287474,170.985485079299));
#18727=CARTESIAN_POINT('Ctrl Pts',(-34.079873038293,-7.27493507937169,170.985485077263));
#18728=CARTESIAN_POINT('Ctrl Pts',(-34.2524227913675,-7.70695486409456,
170.985485076885));
#18729=CARTESIAN_POINT('Ctrl Pts',(-34.4249718336375,-8.13897504114208,
170.985485075754));
#18730=CARTESIAN_POINT('Ctrl Pts',(-34.5973624686691,-8.57105438556268,
170.985485074165));
#18731=CARTESIAN_POINT('Ctrl Pts',(-35.5425661780249,-10.9401099842479,
170.98548506545));
#18732=CARTESIAN_POINT('Ctrl Pts',(-36.4822688726745,-13.3112613391608,
170.985485074703));
#18733=CARTESIAN_POINT('Ctrl Pts',(-37.3903504544009,-15.6940571120185,
170.985485073188));
#18734=CARTESIAN_POINT('Ctrl Pts',(-37.542139679303,-16.0923503168805,170.985485072934));
#18735=CARTESIAN_POINT('Ctrl Pts',(-37.6930696748215,-16.4909865893479,
170.985485072388));
#18736=CARTESIAN_POINT('Ctrl Pts',(-37.8430949741869,-16.8899478627579,
170.985485071651));
#18737=CARTESIAN_POINT('Ctrl Pts',(-38.7542950670207,-19.3130961644508,
170.985485067177));
#18738=CARTESIAN_POINT('Ctrl Pts',(-39.6317664375482,-21.7487445692906,
170.985485069843));
#18739=CARTESIAN_POINT('Ctrl Pts',(-40.464924739775,-24.1928394847348,170.985485069762));
#18740=CARTESIAN_POINT('Ctrl Pts',(-40.5896004612047,-24.5585794599729,
170.98548506975));
#18741=CARTESIAN_POINT('Ctrl Pts',(-40.7133135695025,-24.9245349475724,
170.98548506971));
#18742=CARTESIAN_POINT('Ctrl Pts',(-40.8360698007184,-25.2907036421335,
170.985485069638));
#18743=CARTESIAN_POINT('Ctrl Pts',(-41.6687056219754,-27.7743671490236,
170.985485069145));
#18744=CARTESIAN_POINT('Ctrl Pts',(-42.4572397555062,-30.2679730819714,
170.985485069131));
#18745=CARTESIAN_POINT('Ctrl Pts',(-43.2033006997277,-32.7711592916608,
170.985485069113));
#18746=CARTESIAN_POINT('Ctrl Pts',(-44.0593573456883,-35.6434034527833,
170.985485069092));
#18747=CARTESIAN_POINT('Ctrl Pts',(-44.859958903692,-38.5281560241757,170.985485069062));
#18748=CARTESIAN_POINT('Ctrl Pts',(-45.6122146833682,-41.423821403948,170.985485069353));
#18749=CARTESIAN_POINT('Ctrl Pts',(-45.6894902577951,-41.721279012936,170.985485069383));
#18750=CARTESIAN_POINT('Ctrl Pts',(-45.7662597309399,-42.0188508621958,
170.985485069417));
#18751=CARTESIAN_POINT('Ctrl Pts',(-45.8425306268857,-42.3165352636523,
170.985485069456));
#18752=CARTESIAN_POINT('Ctrl Pts',(-47.2512086805445,-47.8145889845178,
170.985485070179));
#18753=CARTESIAN_POINT('Ctrl Pts',(-48.490005626333,-53.3509733909632,170.98548506891));
#18754=CARTESIAN_POINT('Ctrl Pts',(-49.6060214953918,-58.9150621777573,
170.985485069344));
#18755=CARTESIAN_POINT('Ctrl Pts',(-49.6512921438859,-59.1407667708916,
170.985485069362));
#18756=CARTESIAN_POINT('Ctrl Pts',(-49.6963607743348,-59.3665169394474,
170.985485069382));
#18757=CARTESIAN_POINT('Ctrl Pts',(-49.7412295360745,-59.5923121966672,
170.985485069408));
#18758=CARTESIAN_POINT('Ctrl Pts',(-50.8623576811791,-65.2342200203911,
170.985485070049));
#18759=CARTESIAN_POINT('Ctrl Pts',(-51.8590090750871,-70.9043245719156,
170.985485069059));
#18760=CARTESIAN_POINT('Ctrl Pts',(-52.7647123253029,-76.5947288226584,
170.985485069125));
#18761=CARTESIAN_POINT('Ctrl Pts',(-52.7888259492539,-76.7462312802221,
170.985485069127));
#18762=CARTESIAN_POINT('Ctrl Pts',(-52.8128750527938,-76.8977498306085,
170.985485069129));
#18763=CARTESIAN_POINT('Ctrl Pts',(-52.8368600283206,-77.049284227944,170.985485069132));
#18764=CARTESIAN_POINT('Ctrl Pts',(-53.7497954202113,-82.8171081000875,
170.985485069235));
#18765=CARTESIAN_POINT('Ctrl Pts',(-54.5700444916928,-88.6081190949848,
170.985485069075));
#18766=CARTESIAN_POINT('Ctrl Pts',(-55.3194711561834,-94.4094288582262,
170.985485069086));
#18767=CARTESIAN_POINT('Ctrl Pts',(-55.3292569335755,-94.4851805342949,
170.985485069086));
#18768=CARTESIAN_POINT('Ctrl Pts',(-55.3390305632831,-94.5609336213681,
170.985485069086));
#18769=CARTESIAN_POINT('Ctrl Pts',(-55.3487920806066,-94.6366881163334,
170.985485069086));
#18770=CARTESIAN_POINT('Ctrl Pts',(-56.1061223474536,-100.513968254811,
170.9854850691));
#18771=CARTESIAN_POINT('Ctrl Pts',(-56.7906477111516,-106.399981462517,
170.985485069079));
#18772=CARTESIAN_POINT('Ctrl Pts',(-57.4188561822461,-112.292749775204,
170.985485069079));
#18773=CARTESIAN_POINT('Origin',(-67.998054881725,-13.4265585667677,180.985485069079));
#18774=CARTESIAN_POINT('Origin',(-67.998054881725,-13.4265585667677,171.485485069079));
#18775=CARTESIAN_POINT('Origin',(-67.998054881725,-13.4265585667677,173.485485069079));
#18776=CARTESIAN_POINT('Ctrl Pts',(-57.4188561822461,-112.292749775204,
170.985485069079));
#18777=CARTESIAN_POINT('Ctrl Pts',(-53.4413942236179,-112.716773792997,
170.985485069079));
#18778=CARTESIAN_POINT('Ctrl Pts',(-53.4413942236179,-112.716773792997,
174.985485069079));
#18779=CARTESIAN_POINT('Ctrl Pts',(-56.7826130392591,-106.324614029273,
170.985485069079));
#18780=CARTESIAN_POINT('Ctrl Pts',(-52.8079181997713,-106.774594389709,
170.985485067414));
#18781=CARTESIAN_POINT('Ctrl Pts',(-52.8079182001533,-106.774594389693,
174.98548506783));
#18782=CARTESIAN_POINT('Ctrl Pts',(-56.0885640554346,-100.362870586925,
170.985485069079));
#18783=CARTESIAN_POINT('Ctrl Pts',(-52.1171985560672,-100.841826095817,
170.985485068746));
#18784=CARTESIAN_POINT('Ctrl Pts',(-52.1171985561525,-100.841826095775,
174.985485068829));
#18785=CARTESIAN_POINT('Ctrl Pts',(-54.5503923877258,-88.455985304064,170.985485069079));
#18786=CARTESIAN_POINT('Ctrl Pts',(-50.587687217705,-89.0019798491525,170.985485069413));
#18787=CARTESIAN_POINT('Ctrl Pts',(-50.5876872176197,-89.0019798491944,
174.985485069329));
#18788=CARTESIAN_POINT('Ctrl Pts',(-53.7067133387789,-82.5129732641369,
170.985485069079));
#18789=CARTESIAN_POINT('Ctrl Pts',(-49.7493162082364,-83.0969773147974,
170.985485069079));
#18790=CARTESIAN_POINT('Ctrl Pts',(-49.7493162081637,-83.096977314809,174.985485069079));
#18791=CARTESIAN_POINT('Ctrl Pts',(-51.8227490518109,-70.6764783742679,
170.985485069079));
#18792=CARTESIAN_POINT('Ctrl Pts',(-47.879595467558,-71.3499712035021,170.985485069079));
#18793=CARTESIAN_POINT('Ctrl Pts',(-47.8795954676306,-71.3499712034905,
174.985485069079));
#18794=CARTESIAN_POINT('Ctrl Pts',(-50.7825461626129,-64.7803920175373,
170.985485069079));
#18795=CARTESIAN_POINT('Ctrl Pts',(-46.8482928517823,-65.5053796921416,
170.985485069079));
#18796=CARTESIAN_POINT('Ctrl Pts',(-46.8482928517271,-65.5053796921527,
174.985485069079));
#18797=CARTESIAN_POINT('Ctrl Pts',(-48.429587030133,-53.0497142451155,170.985485069079));
#18798=CARTESIAN_POINT('Ctrl Pts',(-44.5200735879382,-53.8980425350056,
170.985485069079));
#18799=CARTESIAN_POINT('Ctrl Pts',(-44.5200735879935,-53.8980425349946,
174.985485069079));
#18800=CARTESIAN_POINT('Ctrl Pts',(-47.116819037505,-47.2151254801378,170.985485069079));
#18801=CARTESIAN_POINT('Ctrl Pts',(-43.2231877084345,-48.1356655301653,
170.985485069079));
#18802=CARTESIAN_POINT('Ctrl Pts',(-43.2231877083669,-48.1356655301828,
174.985485069079));
#18803=CARTESIAN_POINT('Ctrl Pts',(-44.8599803826999,-38.5281517318545,
170.985485069079));
#18804=CARTESIAN_POINT('Ctrl Pts',(-40.9995722140334,-39.5765736406343,
170.985485069079));
#18805=CARTESIAN_POINT('Ctrl Pts',(-40.9995722140672,-39.5765736406255,
174.985485069079));
#18806=CARTESIAN_POINT('Ctrl Pts',(-44.0593677242217,-35.6433989890554,
170.985485069079));
#18807=CARTESIAN_POINT('Ctrl Pts',(-40.2116389363166,-36.7377081133746,
170.985485069079));
#18808=CARTESIAN_POINT('Ctrl Pts',(-40.2116389362875,-36.7377081133832,
174.985485069079));
#18809=CARTESIAN_POINT('Ctrl Pts',(-42.3472650417746,-29.8989102456991,
170.985485069079));
#18810=CARTESIAN_POINT('Ctrl Pts',(-38.5282657072424,-31.0896131337399,
170.985485069079));
#18811=CARTESIAN_POINT('Ctrl Pts',(-38.5282657072715,-31.0896131337312,
174.985485069079));
#18812=CARTESIAN_POINT('Ctrl Pts',(-41.4353095848977,-27.039279258621,170.985485069079));
#18813=CARTESIAN_POINT('Ctrl Pts',(-37.6324604140697,-28.2806667005876,
170.985485069079));
#18814=CARTESIAN_POINT('Ctrl Pts',(-37.6324604140849,-28.2806667005877,
174.985485069079));
#18815=CARTESIAN_POINT('Ctrl Pts',(-39.4946798076272,-21.3463520167058,
170.985485069079));
#18816=CARTESIAN_POINT('Ctrl Pts',(-35.7253902478902,-22.686188130551,170.985485069079));
#18817=CARTESIAN_POINT('Ctrl Pts',(-35.725390247875,-22.6861881305509,174.985485069079));
#18818=CARTESIAN_POINT('Ctrl Pts',(-38.4642123465852,-18.5114604936425,
170.985485069079));
#18819=CARTESIAN_POINT('Ctrl Pts',(-34.7124817228929,-19.8992827188875,
170.985485069079));
#18820=CARTESIAN_POINT('Ctrl Pts',(-34.712481722994,-19.899282718849,174.985485069079));
#18821=CARTESIAN_POINT('Ctrl Pts',(-36.316827378144,-12.8765246130018,170.985485069079));
#18822=CARTESIAN_POINT('Ctrl Pts',(-32.5929839678225,-14.3375254538628,
170.985485069079));
#18823=CARTESIAN_POINT('Ctrl Pts',(-32.5929839677214,-14.3375254539014,
174.985485069079));
#18824=CARTESIAN_POINT('Ctrl Pts',(-35.1986985564766,-10.0755969552936,
170.985485069079));
#18825=CARTESIAN_POINT('Ctrl Pts',(-31.4848789139723,-11.5613793000778,
170.985485069079));
#18826=CARTESIAN_POINT('Ctrl Pts',(-31.4848789142267,-11.561379299971,174.985485069079));
#18827=CARTESIAN_POINT('Ctrl Pts',(-32.9615227473215,-4.47408340352996,
170.985485069079));
#18828=CARTESIAN_POINT('Ctrl Pts',(-29.2459613632304,-5.95550471904053,
170.985485069079));
#18829=CARTESIAN_POINT('Ctrl Pts',(-29.2459613629761,-5.95550471914736,
174.985485069079));
#18830=CARTESIAN_POINT('Ctrl Pts',(-31.8444493580227,-1.67276288830323,
170.985485069079));
#18831=CARTESIAN_POINT('Ctrl Pts',(-28.1161190404298,-3.12330252930428,
170.985485069079));
#18832=CARTESIAN_POINT('Ctrl Pts',(-28.1161190407185,-3.12330252919715,
174.985485069079));
#18833=CARTESIAN_POINT('Ctrl Pts',(-29.7527124597669,3.98288655387735,170.985485069079));
#18834=CARTESIAN_POINT('Ctrl Pts',(-25.9777796362599,2.65835101834502,170.985485069079));
#18835=CARTESIAN_POINT('Ctrl Pts',(-25.9777796359711,2.6583510182379,174.985485069079));
#18836=CARTESIAN_POINT('Ctrl Pts',(-28.7818376120864,6.83882893219871,170.985485069079));
#18837=CARTESIAN_POINT('Ctrl Pts',(-24.9741240759836,5.6087285236563,170.985485069079));
#18838=CARTESIAN_POINT('Ctrl Pts',(-24.9741240760463,5.60872852367469,174.985485069079));
#18839=CARTESIAN_POINT('Ctrl Pts',(-27.0805945471387,12.6394205519279,170.985485069079));
#18840=CARTESIAN_POINT('Ctrl Pts',(-23.2116619383549,11.618053890714,170.985485069079));
#18841=CARTESIAN_POINT('Ctrl Pts',(-23.2116619382922,11.6180538906956,174.985485069079));
#18842=CARTESIAN_POINT('Ctrl Pts',(-26.3554676902183,15.562162940868,170.985485069079));
#18843=CARTESIAN_POINT('Ctrl Pts',(-22.4590134306381,14.65207208465,170.985485069079));
#18844=CARTESIAN_POINT('Ctrl Pts',(-22.4590134305428,14.6520720846303,174.985485069079));
#18845=CARTESIAN_POINT('Ctrl Pts',(-25.4433917160236,19.9776877415196,170.985485069079));
#18846=CARTESIAN_POINT('Ctrl Pts',(-21.5156656424655,19.2189893943357,170.985485069079));
#18847=CARTESIAN_POINT('Ctrl Pts',(-21.5156656425132,19.2189893943455,174.985485069079));
#18848=CARTESIAN_POINT('Ctrl Pts',(-25.1680142641662,21.4546534375747,170.985485069079));
#18849=CARTESIAN_POINT('Ctrl Pts',(-21.2313563309936,20.7441370734468,170.985485069079));
#18850=CARTESIAN_POINT('Ctrl Pts',(-21.2313563309339,20.7441370734394,174.985485069079));
#18851=CARTESIAN_POINT('Ctrl Pts',(-24.7932108072927,23.6769458352522,170.985485069079));
#18852=CARTESIAN_POINT('Ctrl Pts',(-20.8450961455913,23.0343589425206,170.985485069079));
#18853=CARTESIAN_POINT('Ctrl Pts',(-20.8450961456211,23.0343589425243,174.985485069079));
#18854=CARTESIAN_POINT('Ctrl Pts',(-24.6746446772461,24.418849042421,170.985485069079));
#18855=CARTESIAN_POINT('Ctrl Pts',(-20.7230313702667,23.7981943284674,170.985485069079));
#18856=CARTESIAN_POINT('Ctrl Pts',(-20.7230313702386,23.7981943284632,174.985485069079));
#18857=CARTESIAN_POINT('Ctrl Pts',(-24.505722723831,25.5333006223766,170.985485069079));
#18858=CARTESIAN_POINT('Ctrl Pts',(-20.5492881240966,24.9444540731779,170.985485069079));
#18859=CARTESIAN_POINT('Ctrl Pts',(-20.5492881241107,24.94445407318,174.985485069079));
#18860=CARTESIAN_POINT('Ctrl Pts',(-24.4509032451114,25.9050506043959,170.985485069079));
#18861=CARTESIAN_POINT('Ctrl Pts',(-20.4929326108229,25.3266255922602,170.985485069079));
#18862=CARTESIAN_POINT('Ctrl Pts',(-20.4929326108094,25.3266255922583,174.985485069079));
#18863=CARTESIAN_POINT('Ctrl Pts',(-24.3441364534122,26.6490642977548,170.985485069079));
#18864=CARTESIAN_POINT('Ctrl Pts',(-20.3832266462647,26.0911211678509,170.985485069079));
#18865=CARTESIAN_POINT('Ctrl Pts',(-20.3832266462781,26.0911211678529,174.985485069079));
#18866=CARTESIAN_POINT('Ctrl Pts',(-24.2925780488274,27.0213863993399,170.985485069079));
#18867=CARTESIAN_POINT('Ctrl Pts',(-20.3297617855482,26.4772473384921,170.985485069079));
#18868=CARTESIAN_POINT('Ctrl Pts',(-20.3297617855514,26.4772473384925,174.985485069079));
#18869=CARTESIAN_POINT('Ctrl Pts',(-24.2414621684861,27.3938099964894,170.985485069079));
#18870=CARTESIAN_POINT('Ctrl Pts',(-20.2786142962294,26.8499012345166,170.985485069079));
#18871=CARTESIAN_POINT('Ctrl Pts',(-20.2786142962294,26.8499012345166,174.985485069079));
#18872=CARTESIAN_POINT('Ctrl Pts',(-24.4968853994471,25.5961755935782,170.985485069079));
#18873=CARTESIAN_POINT('Ctrl Pts',(-24.2311967766072,25.620873127159,170.985485069285));
#18874=CARTESIAN_POINT('Ctrl Pts',(-23.9697295431316,25.6452190869017,171.010442378523));
#18875=CARTESIAN_POINT('Ctrl Pts',(-23.7123793162008,25.6692186217661,171.059399504179));
#18876=CARTESIAN_POINT('Ctrl Pts',(-23.7113153156031,25.6693178465452,171.059601914768));
#18877=CARTESIAN_POINT('Ctrl Pts',(-23.7102513470147,25.6694170689936,171.059804751606));
#18878=CARTESIAN_POINT('Ctrl Pts',(-23.7091874109976,25.6695162890582,171.060008014593));
#18879=CARTESIAN_POINT('Ctrl Pts',(-23.5057804574324,25.6884855228749,171.098868532867));
#18880=CARTESIAN_POINT('Ctrl Pts',(-23.3035081474716,25.7073729132474,171.153320157475));
#18881=CARTESIAN_POINT('Ctrl Pts',(-23.1063670980905,25.7258021132664,171.222655786241));
#18882=CARTESIAN_POINT('Ctrl Pts',(-23.0549689640615,25.7306069293897,171.240732802426));
#18883=CARTESIAN_POINT('Ctrl Pts',(-23.0039194998808,25.7353806115,171.259821295379));
#18884=CARTESIAN_POINT('Ctrl Pts',(-22.9532892035529,25.7401165199994,171.279908231871));
#18885=CARTESIAN_POINT('Ctrl Pts',(-22.9514181264669,25.7402915387237,171.280650558291));
#18886=CARTESIAN_POINT('Ctrl Pts',(-22.9495477609699,25.7404664927989,171.281394161589));
#18887=CARTESIAN_POINT('Ctrl Pts',(-22.9476781070859,25.7406413822181,171.282139041655));
#18888=CARTESIAN_POINT('Ctrl Pts',(-22.749261664958,25.759201467923,171.361189209017));
#18889=CARTESIAN_POINT('Ctrl Pts',(-22.5588332490509,25.7770361827933,171.454634081597));
#18890=CARTESIAN_POINT('Ctrl Pts',(-22.3764129335352,25.7941386741052,171.562330579903));
#18891=CARTESIAN_POINT('Ctrl Pts',(-22.3344346010229,25.7980742777963,171.587113562016));
#18892=CARTESIAN_POINT('Ctrl Pts',(-22.2928802296816,25.8019711166271,171.612651042871));
#18893=CARTESIAN_POINT('Ctrl Pts',(-22.2517498765304,25.8058291246237,171.63894093754));
#18894=CARTESIAN_POINT('Ctrl Pts',(-22.249557397228,25.8060347781626,171.640342336884));
#18895=CARTESIAN_POINT('Ctrl Pts',(-22.2473659252672,25.8062403399649,171.641746095296));
#18896=CARTESIAN_POINT('Ctrl Pts',(-22.2451754709029,25.8064458090578,171.643152205469));
#18897=CARTESIAN_POINT('Ctrl Pts',(-22.0863321814473,25.8213456340087,171.74511788384));
#18898=CARTESIAN_POINT('Ctrl Pts',(-21.9327437650712,25.8357658974467,171.859516657719));
#18899=CARTESIAN_POINT('Ctrl Pts',(-21.7883375934458,25.849334383468,171.983584558283));
#18900=CARTESIAN_POINT('Ctrl Pts',(-21.733215969023,25.8545136426509,172.030942812718));
#18901=CARTESIAN_POINT('Ctrl Pts',(-21.6794318011014,25.8595688351721,172.079709652122));
#18902=CARTESIAN_POINT('Ctrl Pts',(-21.6272015230238,25.8644794472182,172.1297306957));
#18903=CARTESIAN_POINT('Ctrl Pts',(-21.6251536123851,25.8646719886908,172.131691983886));
#18904=CARTESIAN_POINT('Ctrl Pts',(-21.6231079442685,25.8648643215606,172.133655207642));
#18905=CARTESIAN_POINT('Ctrl Pts',(-21.6210645192453,25.8650564457624,172.135620367119));
#18906=CARTESIAN_POINT('Ctrl Pts',(-21.4322727467778,25.8828067758117,172.317181196012));
#18907=CARTESIAN_POINT('Ctrl Pts',(-21.2625723923638,25.8987813228249,172.515322627133));
#18908=CARTESIAN_POINT('Ctrl Pts',(-21.1123142886195,25.9129371819159,172.730296947743));
#18909=CARTESIAN_POINT('Ctrl Pts',(-21.1108026321242,25.9130795955083,172.73245967521));
#18910=CARTESIAN_POINT('Ctrl Pts',(-21.1092929703707,25.9132218225119,172.734624218554));
#18911=CARTESIAN_POINT('Ctrl Pts',(-21.1077853097955,25.913363862311,172.736790566379));
#18912=CARTESIAN_POINT('Ctrl Pts',(-20.9825286565164,25.9251645488611,172.916771049295));
#18913=CARTESIAN_POINT('Ctrl Pts',(-20.871068234139,25.9356720301901,173.109226845106));
#18914=CARTESIAN_POINT('Ctrl Pts',(-20.7770687387732,25.9445374993322,173.307711809801));
#18915=CARTESIAN_POINT('Ctrl Pts',(-20.758343486239,25.9463035529463,173.347251182578));
#18916=CARTESIAN_POINT('Ctrl Pts',(-20.7403111257963,25.9480044477976,173.387029977365));
#18917=CARTESIAN_POINT('Ctrl Pts',(-20.7230006234092,25.9496374272564,173.426997467644));
#18918=CARTESIAN_POINT('Ctrl Pts',(-20.7221958278602,25.9497133473291,173.42885562621));
#18919=CARTESIAN_POINT('Ctrl Pts',(-20.7213924732957,25.9497891318426,173.430714336564));
#18920=CARTESIAN_POINT('Ctrl Pts',(-20.7205905601952,25.9498647807505,173.432573598924));
#18921=CARTESIAN_POINT('Ctrl Pts',(-20.6265972034254,25.9587316951138,173.650500342107));
#18922=CARTESIAN_POINT('Ctrl Pts',(-20.5524177598076,25.9657340826921,173.875976284431));
#18923=CARTESIAN_POINT('Ctrl Pts',(-20.4988179155159,25.9707948958704,174.109381554084));
#18924=CARTESIAN_POINT('Ctrl Pts',(-20.4930004344399,25.9713441733037,174.134714290721));
#18925=CARTESIAN_POINT('Ctrl Pts',(-20.4874254268857,25.9718705746878,174.160140452629));
#18926=CARTESIAN_POINT('Ctrl Pts',(-20.4820939068001,25.9723739982273,174.18566053939));
#18927=CARTESIAN_POINT('Ctrl Pts',(-20.481863032781,25.9723957982795,174.186765651047));
#18928=CARTESIAN_POINT('Ctrl Pts',(-20.481632638324,25.972417553073,174.187870862314));
#18929=CARTESIAN_POINT('Ctrl Pts',(-20.4814027234763,25.9724392626033,174.188976172781));
#18930=CARTESIAN_POINT('Ctrl Pts',(-20.4595046689509,25.9745069693321,174.294250578148));
#18931=CARTESIAN_POINT('Ctrl Pts',(-20.4419804524051,25.9761618272396,174.400292622434));
#18932=CARTESIAN_POINT('Ctrl Pts',(-20.4288329501748,25.9774034459845,174.50689626372));
#18933=CARTESIAN_POINT('Ctrl Pts',(-20.4157271529572,25.9786411262074,174.613161749047));
#18934=CARTESIAN_POINT('Ctrl Pts',(-20.4069702858337,25.9794681908885,174.71998596903));
#18935=CARTESIAN_POINT('Ctrl Pts',(-20.4026160570217,25.9798794514795,174.82717079242));
#18936=CARTESIAN_POINT('Ctrl Pts',(-20.4004755131676,25.9800816276554,174.879862973944));
#18937=CARTESIAN_POINT('Ctrl Pts',(-20.3993997459139,25.9801832417458,174.932642329276));
#18938=CARTESIAN_POINT('Ctrl Pts',(-20.3993997459139,25.9801832417458,174.985485069079));
#18939=CARTESIAN_POINT('Ctrl Pts',(-24.2415334023097,27.3932909961974,180.985485069079));
#18940=CARTESIAN_POINT('Ctrl Pts',(-20.278685530053,26.8493822342246,180.985485069079));
#18941=CARTESIAN_POINT('Ctrl Pts',(-20.278685530053,26.8493822342246,176.985485069079));
#18942=CARTESIAN_POINT('Ctrl Pts',(-24.2926179909382,27.0210953863739,180.985485069079));
#18943=CARTESIAN_POINT('Ctrl Pts',(-20.3298036372618,26.4769424124262,180.985485069079));
#18944=CARTESIAN_POINT('Ctrl Pts',(-20.3298036372611,26.4769424124265,176.985485069079));
#18945=CARTESIAN_POINT('Ctrl Pts',(-24.3441461251675,26.6489998256275,180.985485069079));
#18946=CARTESIAN_POINT('Ctrl Pts',(-20.3832365919444,26.0910548674088,180.985485069079));
#18947=CARTESIAN_POINT('Ctrl Pts',(-20.3832365919587,26.0910548674102,176.985485069079));
#18948=CARTESIAN_POINT('Ctrl Pts',(-24.4508478987634,25.9054333651556,180.985485069079));
#18949=CARTESIAN_POINT('Ctrl Pts',(-20.4928757331822,25.3270189434495,180.985485069079));
#18950=CARTESIAN_POINT('Ctrl Pts',(-20.4928757331679,25.3270189434481,176.985485069079));
#18951=CARTESIAN_POINT('Ctrl Pts',(-24.5056334618508,25.5339044052764,180.985485069079));
#18952=CARTESIAN_POINT('Ctrl Pts',(-20.5491963566518,24.9450748104871,180.985485069079));
#18953=CARTESIAN_POINT('Ctrl Pts',(-20.5491963566663,24.9450748104893,176.985485069079));
#18954=CARTESIAN_POINT('Ctrl Pts',(-24.6744493717257,24.4201078416409,180.985485069079));
#18955=CARTESIAN_POINT('Ctrl Pts',(-20.7228304061464,23.7994896118014,180.985485069079));
#18956=CARTESIAN_POINT('Ctrl Pts',(-20.7228304061173,23.799489611797,176.985485069079));
#18957=CARTESIAN_POINT('Ctrl Pts',(-24.7929390693147,23.6786305769485,180.985485069079));
#18958=CARTESIAN_POINT('Ctrl Pts',(-20.844816338285,23.0360937770448,180.985485069079));
#18959=CARTESIAN_POINT('Ctrl Pts',(-20.8448163383128,23.0360937770495,176.985485069079));
#18960=CARTESIAN_POINT('Ctrl Pts',(-25.1674956400503,21.4575816922395,180.985485069079));
#18961=CARTESIAN_POINT('Ctrl Pts',(-21.2308213810126,20.7471576413164,180.985485069079));
#18962=CARTESIAN_POINT('Ctrl Pts',(-21.2308213809569,20.747157641307,176.985485069079));
#18963=CARTESIAN_POINT('Ctrl Pts',(-25.4426848277649,19.9813991557405,180.985485069079));
#18964=CARTESIAN_POINT('Ctrl Pts',(-21.514935511514,19.2228232467,180.985485069079));
#18965=CARTESIAN_POINT('Ctrl Pts',(-21.5149355115658,19.2228232467107,176.985485069079));
#18966=CARTESIAN_POINT('Ctrl Pts',(-26.0503136106968,17.0391806793695,180.985485069079));
#18967=CARTESIAN_POINT('Ctrl Pts',(-22.1433957211981,16.1797362624707,180.985485069079));
#18968=CARTESIAN_POINT('Ctrl Pts',(-22.1433957211464,16.17973626246,176.985485069079));
#18969=CARTESIAN_POINT('Ctrl Pts',(-26.3828251631526,15.5731574926212,180.985485069079));
#18970=CARTESIAN_POINT('Ctrl Pts',(-22.4878342294287,14.6609731726812,180.985485069079));
#18971=CARTESIAN_POINT('Ctrl Pts',(-22.4878342294486,14.6609731726861,176.985485069079));
#18972=CARTESIAN_POINT('Ctrl Pts',(-27.109507055406,12.6520390211126,180.985485069079));
#18973=CARTESIAN_POINT('Ctrl Pts',(-23.241113420143,11.6329387856295,180.985485069079));
#18974=CARTESIAN_POINT('Ctrl Pts',(-23.2411134201231,11.6329387856246,176.985485069079));
#18975=CARTESIAN_POINT('Ctrl Pts',(-27.5040176966898,11.1961293872236,180.985485069079));
#18976=CARTESIAN_POINT('Ctrl Pts',(-23.6503198129769,10.1228332499071,180.985485069079));
#18977=CARTESIAN_POINT('Ctrl Pts',(-23.6503198129348,10.1228332498947,176.985485069079));
#18978=CARTESIAN_POINT('Ctrl Pts',(-28.7782751940985,6.85013767399355,180.985485069079));
#18979=CARTESIAN_POINT('Ctrl Pts',(-24.97043768125,5.62042982854441,180.985485069079));
#18980=CARTESIAN_POINT('Ctrl Pts',(-24.9704376813344,5.62042982856915,176.985485069079));
#18981=CARTESIAN_POINT('Ctrl Pts',(-29.7477097626479,3.99730639154945,180.985485069079));
#18982=CARTESIAN_POINT('Ctrl Pts',(-25.9726213257473,2.67321154894945,180.985485069079));
#18983=CARTESIAN_POINT('Ctrl Pts',(-25.972621325458,2.67321154884444,176.985485069079));
#18984=CARTESIAN_POINT('Ctrl Pts',(-31.8366868970815,-1.65266278222268,
180.985485069079));
#18985=CARTESIAN_POINT('Ctrl Pts',(-28.1082275246236,-3.10287330721842,
180.985485069079));
#18986=CARTESIAN_POINT('Ctrl Pts',(-28.1082275249129,-3.10287330711342,
176.985485069079));
#18987=CARTESIAN_POINT('Ctrl Pts',(-32.9524088799731,-4.4512181944314,180.985485069079));
#18988=CARTESIAN_POINT('Ctrl Pts',(-29.2367745540547,-5.93245683765708,
180.985485069079));
#18989=CARTESIAN_POINT('Ctrl Pts',(-29.2367745537956,-5.93245683776055,
176.985485069079));
#18990=CARTESIAN_POINT('Ctrl Pts',(-35.1872819016544,-10.0470567632054,
180.985485069079));
#18991=CARTESIAN_POINT('Ctrl Pts',(-31.4735186150714,-11.5329802516063,
180.985485069079));
#18992=CARTESIAN_POINT('Ctrl Pts',(-31.4735186153305,-11.5329802515028,
176.985485069079));
#18993=CARTESIAN_POINT('Ctrl Pts',(-36.3044540496635,-12.8450741320516,
180.985485069079));
#18994=CARTESIAN_POINT('Ctrl Pts',(-32.5807344389687,-14.3063866454124,
180.985485069079));
#18995=CARTESIAN_POINT('Ctrl Pts',(-32.5807344388679,-14.3063866454508,
176.985485069079));
#18996=CARTESIAN_POINT('Ctrl Pts',(-38.4502987871715,-18.4739441657436,
180.985485069079));
#18997=CARTESIAN_POINT('Ctrl Pts',(-34.6987852921578,-19.8623491849324,
180.985485069079));
#18998=CARTESIAN_POINT('Ctrl Pts',(-34.6987852922586,-19.862349184894,176.985485069079));
#18999=CARTESIAN_POINT('Ctrl Pts',(-39.4801549046855,-21.3055854274631,
180.985485069079));
#19000=CARTESIAN_POINT('Ctrl Pts',(-35.7111108093928,-22.6461097640756,
180.985485069079));
#19001=CARTESIAN_POINT('Ctrl Pts',(-35.7111108093873,-22.6461097640774,
176.985485069079));
#19002=CARTESIAN_POINT('Ctrl Pts',(-41.4205088263372,-26.9940453161076,
180.985485069079));
#19003=CARTESIAN_POINT('Ctrl Pts',(-37.6179212387892,-28.2362315051643,
180.985485069079));
#19004=CARTESIAN_POINT('Ctrl Pts',(-37.6179212387947,-28.2362315051624,
176.985485069079));
#19005=CARTESIAN_POINT('Ctrl Pts',(-42.3326945401042,-29.8522172923435,
180.985485069079));
#19006=CARTESIAN_POINT('Ctrl Pts',(-38.5139474648075,-31.0437297254249,
180.985485069079));
#19007=CARTESIAN_POINT('Ctrl Pts',(-38.5139474648464,-31.0437297254133,
176.985485069079));
#19008=CARTESIAN_POINT('Ctrl Pts',(-44.0456869733603,-35.5953385529714,
180.985485069079));
#19009=CARTESIAN_POINT('Ctrl Pts',(-40.1981801154455,-36.6904285408454,
180.985485069079));
#19010=CARTESIAN_POINT('Ctrl Pts',(-40.1981801154065,-36.690428540857,176.985485069079));
#19011=CARTESIAN_POINT('Ctrl Pts',(-44.8469569069594,-38.4801764731839,
180.985485069079));
#19012=CARTESIAN_POINT('Ctrl Pts',(-40.986749817546,-39.5293406298925,180.985485069079));
#19013=CARTESIAN_POINT('Ctrl Pts',(-40.986749817569,-39.5293406298865,176.985485069079));
#19014=CARTESIAN_POINT('Ctrl Pts',(-47.1060660254085,-47.1694786137269,
180.985485069079));
#19015=CARTESIAN_POINT('Ctrl Pts',(-43.2125745008618,-48.0906195108081,
180.985485069079));
#19016=CARTESIAN_POINT('Ctrl Pts',(-43.2125745008157,-48.0906195108201,
176.985485069079));
#19017=CARTESIAN_POINT('Ctrl Pts',(-48.4207181977957,-53.0083673031996,
180.985485069079));
#19018=CARTESIAN_POINT('Ctrl Pts',(-44.5113064894929,-53.8571726050397,
180.985485069079));
#19019=CARTESIAN_POINT('Ctrl Pts',(-44.5113064895194,-53.8571726050551,
176.985485069079));
#19020=CARTESIAN_POINT('Ctrl Pts',(-50.7773623574713,-64.7516965919457,
180.985485069079));
#19021=CARTESIAN_POINT('Ctrl Pts',(-46.8431551177289,-65.4769439569077,
180.985485069079));
#19022=CARTESIAN_POINT('Ctrl Pts',(-46.8431551177024,-65.4769439568923,
176.985485069079));
#19023=CARTESIAN_POINT('Ctrl Pts',(-51.8193876826615,-70.6561291763739,
180.985485069079));
#19024=CARTESIAN_POINT('Ctrl Pts',(-47.8762608373712,-71.3297841813875,
180.985485069079));
#19025=CARTESIAN_POINT('Ctrl Pts',(-47.8762608373576,-71.3297841813897,
176.985485069079));
#19026=CARTESIAN_POINT('Ctrl Pts',(-53.2348917042471,-79.5482475998618,
180.985485069079));
#19027=CARTESIAN_POINT('Ctrl Pts',(-49.2810610786228,-80.1546620454955,
180.985485069079));
#19028=CARTESIAN_POINT('Ctrl Pts',(-49.2810610786295,-80.1546620454944,
176.985485069079));
#19029=CARTESIAN_POINT('Ctrl Pts',(-53.6818624435884,-82.518291930448,180.985485069079));
#19030=CARTESIAN_POINT('Ctrl Pts',(-49.7249287002307,-83.1040011999898,
180.985485069079));
#19031=CARTESIAN_POINT('Ctrl Pts',(-49.7249287002415,-83.1040011999882,
176.985485069079));
#19032=CARTESIAN_POINT('Ctrl Pts',(-54.5319871398436,-88.4613735803899,
180.985485069079));
#19033=CARTESIAN_POINT('Ctrl Pts',(-50.5695327094811,-89.0084886370079,
180.985485069079));
#19034=CARTESIAN_POINT('Ctrl Pts',(-50.5695327094702,-89.0084886370094,
176.985485069079));
#19035=CARTESIAN_POINT('Ctrl Pts',(-54.9352946649178,-91.4354154550141,
180.985485069079));
#19036=CARTESIAN_POINT('Ctrl Pts',(-50.9704223157392,-91.9646344207502,
180.985485069079));
#19037=CARTESIAN_POINT('Ctrl Pts',(-50.970422315736,-91.9646344207298,176.985485069079));
#19038=CARTESIAN_POINT('Ctrl Pts',(-56.0886961413402,-100.364039043625,
180.985485069079));
#19039=CARTESIAN_POINT('Ctrl Pts',(-52.1173300454227,-100.842989112103,
180.985485069079));
#19040=CARTESIAN_POINT('Ctrl Pts',(-52.1173300454289,-100.842989112144,
176.985485069079));
#19041=CARTESIAN_POINT('Ctrl Pts',(-56.7826622117359,-106.325075281961,
180.985485069079));
#19042=CARTESIAN_POINT('Ctrl Pts',(-52.807967153609,-106.775053587525,180.985485069079));
#19043=CARTESIAN_POINT('Ctrl Pts',(-52.8079671537057,-106.775053587484,
176.985485069079));
#19044=CARTESIAN_POINT('Ctrl Pts',(-57.4188561822461,-112.292749775204,
180.985485069079));
#19045=CARTESIAN_POINT('Ctrl Pts',(-53.4413942236179,-112.716773792997,
180.985485069079));
#19046=CARTESIAN_POINT('Ctrl Pts',(-53.4413942236179,-112.716773792997,
176.985485069079));
#19047=CARTESIAN_POINT('Ctrl Pts',(-20.3993997459139,25.9801832417458,176.985485069079));
#19048=CARTESIAN_POINT('Ctrl Pts',(-20.3993997459139,25.9801832417458,177.253460354772));
#19049=CARTESIAN_POINT('Ctrl Pts',(-20.4266849103993,25.9776057723927,177.516770554086));
#19050=CARTESIAN_POINT('Ctrl Pts',(-20.4800815464371,25.9725641538593,177.775616151056));
#19051=CARTESIAN_POINT('Ctrl Pts',(-20.4803012881147,25.9725434062281,177.776681371076));
#19052=CARTESIAN_POINT('Ctrl Pts',(-20.4805214718867,25.9725226168914,177.77774651468));
#19053=CARTESIAN_POINT('Ctrl Pts',(-20.480742097672,25.9725017858569,177.778811581889));
#19054=CARTESIAN_POINT('Ctrl Pts',(-20.5234236436048,25.9684718817652,177.984856015713));
#19055=CARTESIAN_POINT('Ctrl Pts',(-20.5835648824924,25.9627948754604,178.189817520743));
#19056=CARTESIAN_POINT('Ctrl Pts',(-20.6593131446062,25.9556471231507,178.387733685858));
#19057=CARTESIAN_POINT('Ctrl Pts',(-20.6783192713366,25.9538536683249,178.437393171253));
#19058=CARTESIAN_POINT('Ctrl Pts',(-20.6983081455396,25.9519676032949,178.486608932719));
#19059=CARTESIAN_POINT('Ctrl Pts',(-20.7192508383654,25.9499916825274,178.535286354135));
#19060=CARTESIAN_POINT('Ctrl Pts',(-20.7200499813087,25.9499162842417,178.537143814307));
#19061=CARTESIAN_POINT('Ctrl Pts',(-20.7208505133994,25.9498407552781,178.539000491351));
#19062=CARTESIAN_POINT('Ctrl Pts',(-20.721652433009,25.949765095793,178.540856379937));
#19063=CARTESIAN_POINT('Ctrl Pts',(-20.8260553070923,25.9399148968435,178.782476736931));
#19064=CARTESIAN_POINT('Ctrl Pts',(-20.9533828010123,25.9279083222768,179.011452496788));
#19065=CARTESIAN_POINT('Ctrl Pts',(-21.1034139583469,25.9137749684792,179.227886442344));
#19066=CARTESIAN_POINT('Ctrl Pts',(-21.1049105333212,25.9136339869393,179.230045391406));
#19067=CARTESIAN_POINT('Ctrl Pts',(-21.1064093715489,25.913492793354,179.232203098791));
#19068=CARTESIAN_POINT('Ctrl Pts',(-21.1079104727703,25.9133513877557,179.234359564478));
#19069=CARTESIAN_POINT('Ctrl Pts',(-21.2244365213831,25.9023744893363,179.401759618492));
#19070=CARTESIAN_POINT('Ctrl Pts',(-21.3546271641416,25.8901176743735,179.560987606355));
#19071=CARTESIAN_POINT('Ctrl Pts',(-21.4950259385074,25.8769104720021,179.708596225131));
#19072=CARTESIAN_POINT('Ctrl Pts',(-21.535526013038,25.8731006618183,179.751176084456));
#19073=CARTESIAN_POINT('Ctrl Pts',(-21.5768751842987,25.8692118004005,179.792789103293));
#19074=CARTESIAN_POINT('Ctrl Pts',(-21.61898973787,25.8652518683145,179.833352682713));
#19075=CARTESIAN_POINT('Ctrl Pts',(-21.621024213633,25.8650605713597,179.835312233799));
#19076=CARTESIAN_POINT('Ctrl Pts',(-21.623060483137,25.8648691080782,179.83726934325));
#19077=CARTESIAN_POINT('Ctrl Pts',(-21.625098537302,25.8646774793371,179.839224002025));
#19078=CARTESIAN_POINT('Ctrl Pts',(-21.7635610963668,25.8516584897863,179.972020794527));
#19079=CARTESIAN_POINT('Ctrl Pts',(-21.9114405909342,25.83776470468,180.095037456217));
#19080=CARTESIAN_POINT('Ctrl Pts',(-22.0682312152839,25.8230479395925,180.207628051587));
#19081=CARTESIAN_POINT('Ctrl Pts',(-22.124650811608,25.817752253394,180.248142693117));
#19082=CARTESIAN_POINT('Ctrl Pts',(-22.1822245235746,25.8123499802544,180.287306902747));
#19083=CARTESIAN_POINT('Ctrl Pts',(-22.2409296003261,25.8068434610663,180.325089138399));
#19084=CARTESIAN_POINT('Ctrl Pts',(-22.2431448782432,25.8066356686396,180.326514877993));
#19085=CARTESIAN_POINT('Ctrl Pts',(-22.2453617235553,25.8064277318171,180.327938621455));
#19086=CARTESIAN_POINT('Ctrl Pts',(-22.2475801350017,25.806219650729,180.329360367391));
#19087=CARTESIAN_POINT('Ctrl Pts',(-22.3925906417591,25.7926180512291,180.422295381327));
#19088=CARTESIAN_POINT('Ctrl Pts',(-22.5418509440023,25.7786290931416,180.505212509635));
#19089=CARTESIAN_POINT('Ctrl Pts',(-22.695315785544,25.76425946275,180.578485420675));
#19090=CARTESIAN_POINT('Ctrl Pts',(-22.7771613042894,25.7565958842928,180.61756316222));
#19091=CARTESIAN_POINT('Ctrl Pts',(-22.8602030711131,25.7488239991733,180.653896980504));
#19092=CARTESIAN_POINT('Ctrl Pts',(-22.9444365893079,25.7409446072073,180.687538032982));
#19093=CARTESIAN_POINT('Ctrl Pts',(-22.9463001496801,25.7407702855959,180.688282298847));
#19094=CARTESIAN_POINT('Ctrl Pts',(-22.9481643583708,25.7405959068607,180.689025272588));
#19095=CARTESIAN_POINT('Ctrl Pts',(-22.9500292139766,25.740421471109,180.689766953873));
#19096=CARTESIAN_POINT('Ctrl Pts',(-23.04271460306,25.7317518210453,180.726629335191));
#19097=CARTESIAN_POINT('Ctrl Pts',(-23.1371806620555,25.7229245611075,180.760230126284));
#19098=CARTESIAN_POINT('Ctrl Pts',(-23.2329365689234,25.7139823855379,180.790422755679));
#19099=CARTESIAN_POINT('Ctrl Pts',(-23.3296368764114,25.7049520170156,180.820913162401));
#19100=CARTESIAN_POINT('Ctrl Pts',(-23.4276518178533,25.695804527105,180.847927609303));
#19101=CARTESIAN_POINT('Ctrl Pts',(-23.5264561919686,25.6865857564093,180.871364287284));
#19102=CARTESIAN_POINT('Ctrl Pts',(-23.586216777123,25.6810098986994,180.885539667704));
#19103=CARTESIAN_POINT('Ctrl Pts',(-23.646265830258,25.6754079958158,180.898407166228));
#19104=CARTESIAN_POINT('Ctrl Pts',(-23.7064855675305,25.6697903447738,180.909953373108));
#19105=CARTESIAN_POINT('Ctrl Pts',(-23.7907662810468,25.6619281444462,180.926112901499));
#19106=CARTESIAN_POINT('Ctrl Pts',(-23.8753692960766,25.6540391323433,180.939687708742));
#19107=CARTESIAN_POINT('Ctrl Pts',(-23.9602961099603,25.6461240023457,180.950688406402));
#19108=CARTESIAN_POINT('Ctrl Pts',(-24.0490096964407,25.6378559473296,180.962179610401));
#19109=CARTESIAN_POINT('Ctrl Pts',(-24.1380773688624,25.6295593207584,180.970862622925));
#19110=CARTESIAN_POINT('Ctrl Pts',(-24.2275069672944,25.6212344136867,180.976688931065));
#19111=CARTESIAN_POINT('Ctrl Pts',(-24.311208662952,25.613442711048,180.982142068274));
#19112=CARTESIAN_POINT('Ctrl Pts',(-24.3952280469572,25.6056261751778,180.985092314052));
#19113=CARTESIAN_POINT('Ctrl Pts',(-24.4795664985897,25.5977855805591,180.985448489195));
#19114=CARTESIAN_POINT('Ctrl Pts',(-24.4853379760646,25.5972490303337,180.985472863093));
#19115=CARTESIAN_POINT('Ctrl Pts',(-24.491110943542,25.596712367858,180.985485069075));
#19116=CARTESIAN_POINT('Ctrl Pts',(-24.4968853994148,25.596175593583,180.985485069079));
#19117=CARTESIAN_POINT('Ctrl Pts',(-55.9273079477605,-112.451758781876,
176.985485069079));
#19118=CARTESIAN_POINT('Ctrl Pts',(-55.9273079477605,-112.451758781876,
174.985485069079));
#19119=CARTESIAN_POINT('Ctrl Pts',(-55.9161963178522,-112.347528635931,
176.985485069079));
#19120=CARTESIAN_POINT('Ctrl Pts',(-55.9161963178522,-112.347528635931,
174.985485069079));
#19121=CARTESIAN_POINT('Ctrl Pts',(-55.9050783560045,-112.243408267559,
176.985485069079));
#19122=CARTESIAN_POINT('Ctrl Pts',(-55.9050783560045,-112.243408267559,
174.985485069079));
#19123=CARTESIAN_POINT('Ctrl Pts',(-55.893954080246,-112.139397514846,176.985485069079));
#19124=CARTESIAN_POINT('Ctrl Pts',(-55.893954080246,-112.139397514846,174.985485069079));
#19125=CARTESIAN_POINT('',(-55.8941531222797,-112.141258553928,174.985485069079));
#19126=CARTESIAN_POINT('',(-55.9103881299845,-112.293170927494,176.98548507057));
#19127=CARTESIAN_POINT('Ctrl Pts',(-55.8941531222797,-112.141258553928,
174.985485069079));
#19128=CARTESIAN_POINT('Ctrl Pts',(-55.8985635545636,-112.182496407459,
175.225173349436));
#19129=CARTESIAN_POINT('Ctrl Pts',(-55.9022915288212,-112.217379919497,
175.466099548914));
#19130=CARTESIAN_POINT('Ctrl Pts',(-55.905634973815,-112.248674438416,175.762105987673));
#19131=CARTESIAN_POINT('Ctrl Pts',(-55.9061908793933,-112.253878190418,
175.815650974815));
#19132=CARTESIAN_POINT('Ctrl Pts',(-55.9069724331886,-112.261194689414,
175.898612699006));
#19133=CARTESIAN_POINT('Ctrl Pts',(-55.9072335279748,-112.26363902673,175.927964564546));
#19134=CARTESIAN_POINT('Ctrl Pts',(-55.90752307931,-112.266349861729,175.962609843277));
#19135=CARTESIAN_POINT('Ctrl Pts',(-55.9075666685364,-112.266757955063,
175.967886313802));
#19136=CARTESIAN_POINT('Ctrl Pts',(-55.90763270527,-112.26737621146,175.975974940967));
#19137=CARTESIAN_POINT('Ctrl Pts',(-55.907655516467,-112.267589777688,175.978786794323));
#19138=CARTESIAN_POINT('Ctrl Pts',(-55.9076972825353,-112.267980807186,
175.983968189128));
#19139=CARTESIAN_POINT('Ctrl Pts',(-55.9077162836962,-112.268158703655,
175.986339383711));
#19140=CARTESIAN_POINT('Ctrl Pts',(-55.9077553600245,-112.268524552788,
175.99123478032));
#19141=CARTESIAN_POINT('Ctrl Pts',(-55.9077767006682,-112.26872435356,175.993921954021));
#19142=CARTESIAN_POINT('Ctrl Pts',(-55.9078351002393,-112.269271118478,
176.001313380653));
#19143=CARTESIAN_POINT('Ctrl Pts',(-55.9078719345754,-112.269615981164,
176.006017771104));
#19144=CARTESIAN_POINT('Ctrl Pts',(-55.9080645843082,-112.271419680157,
176.030849218023));
#19145=CARTESIAN_POINT('Ctrl Pts',(-55.908214601632,-112.272824262972,176.050978879581));
#19146=CARTESIAN_POINT('Ctrl Pts',(-55.9087759640173,-112.278080294568,
176.129579022445));
#19147=CARTESIAN_POINT('Ctrl Pts',(-55.9091407847523,-112.281496343087,
176.188039682372));
#19148=CARTESIAN_POINT('Ctrl Pts',(-55.9107627717114,-112.296684608531,
176.493833485863));
#19149=CARTESIAN_POINT('Ctrl Pts',(-55.9110811044381,-112.299666462952,
176.738023108658));
#19150=CARTESIAN_POINT('Ctrl Pts',(-55.9103874835559,-112.293170814203,
176.985485065785));
#19151=CARTESIAN_POINT('Ctrl Pts',(-55.9273079477605,-112.451758781876,
174.985485069079));
#19152=CARTESIAN_POINT('Ctrl Pts',(-55.9162739233362,-112.348256596724,
174.985485069079));
#19153=CARTESIAN_POINT('Ctrl Pts',(-55.9052223395644,-112.244756517776,
174.985485069079));
#19154=CARTESIAN_POINT('Ctrl Pts',(-55.8941531222797,-112.141258553928,
174.985485069079));
#19155=CARTESIAN_POINT('',(-55.9103874835467,-112.293170814116,176.985485069079));
#19156=CARTESIAN_POINT('Origin',(-34.9583934096621,-20.6140499623174,173.485485069079));
#19157=CARTESIAN_POINT('',(-60.9459236613779,-101.771602184887,173.485485069079));
#19158=CARTESIAN_POINT('Origin',(-57.8714679378161,-101.961142909682,173.485484935551));
#19159=CARTESIAN_POINT('Origin',(-57.7124589446281,-100.469594673199,173.485484935556));
#19160=CARTESIAN_POINT('Origin',(-57.5534499237749,-98.9780464405567,173.485484935551));
#19161=CARTESIAN_POINT('',(-37.4541011624573,-44.0244753865006,173.485485069079));
#19162=CARTESIAN_POINT('',(-69.5889371886705,15.3762068992854,173.485485069079));
#19163=CARTESIAN_POINT('',(-62.0059837058594,-111.715257081458,173.485485069079));
#19164=CARTESIAN_POINT('Origin',(-58.5743664423751,-112.487668859306,173.485458785641));
#19165=CARTESIAN_POINT('Ctrl Pts',(-60.5242814633668,-111.628781113343,
173.485485069079));
#19166=CARTESIAN_POINT('Ctrl Pts',(-60.7715770916306,-111.628999793736,
173.485485069079));
#19167=CARTESIAN_POINT('Ctrl Pts',(-61.0198212492056,-111.638374754475,
173.485485069079));
#19168=CARTESIAN_POINT('Ctrl Pts',(-61.5077217781315,-111.668933227103,
173.485485069079));
#19169=CARTESIAN_POINT('Ctrl Pts',(-61.7598509417045,-111.690516273231,
173.485485069079));
#19170=CARTESIAN_POINT('Ctrl Pts',(-62.0059837058594,-111.715257081458,
173.485485069079));
#19171=CARTESIAN_POINT('',(-61.8999777014113,-110.7208915918,173.485485069079));
#19172=CARTESIAN_POINT('Ctrl Pts',(-61.8999777014113,-110.7208915918,173.485485069079));
#19173=CARTESIAN_POINT('Ctrl Pts',(-61.6722691809327,-110.812341651549,
173.485485069079));
#19174=CARTESIAN_POINT('Ctrl Pts',(-61.4408313059547,-110.903719063423,
173.485485070806));
#19175=CARTESIAN_POINT('Ctrl Pts',(-60.9623872716977,-111.087021812589,
173.485485070806));
#19176=CARTESIAN_POINT('Ctrl Pts',(-60.720877573809,-111.177330293225,173.485485069079));
#19177=CARTESIAN_POINT('Ctrl Pts',(-60.4851225885515,-111.26146009287,173.485485069079));
#19178=CARTESIAN_POINT('',(-61.8469746991872,-110.223708846972,173.485485069079));
#19179=CARTESIAN_POINT('Origin',(-58.8255219851367,-110.9104323152,173.485484935551));
#19180=CARTESIAN_POINT('Ctrl Pts',(-60.3652724566946,-110.137232878857,
173.485485069079));
#19181=CARTESIAN_POINT('Ctrl Pts',(-60.612568084958,-110.13745155925,173.485485069079));
#19182=CARTESIAN_POINT('Ctrl Pts',(-60.8608122425326,-110.146826519989,
173.485485069079));
#19183=CARTESIAN_POINT('Ctrl Pts',(-61.3487127714596,-110.177384992617,
173.485485069079));
#19184=CARTESIAN_POINT('Ctrl Pts',(-61.6008419350333,-110.198968038745,
173.485485069079));
#19185=CARTESIAN_POINT('Ctrl Pts',(-61.8469746991872,-110.223708846972,
173.485485069079));
#19186=CARTESIAN_POINT('',(-61.740968694739,-109.229343357315,173.485485069079));
#19187=CARTESIAN_POINT('Ctrl Pts',(-61.740968694739,-109.229343357315,173.485485069079));
#19188=CARTESIAN_POINT('Ctrl Pts',(-61.5132601742589,-109.320793417064,
173.485485069079));
#19189=CARTESIAN_POINT('Ctrl Pts',(-61.281822299282,-109.412170828938,173.485485070806));
#19190=CARTESIAN_POINT('Ctrl Pts',(-60.8033813639377,-109.595472390839,
173.485485070806));
#19191=CARTESIAN_POINT('Ctrl Pts',(-60.5618656159965,-109.685783111862,
173.485485069079));
#19192=CARTESIAN_POINT('Ctrl Pts',(-60.3261135818793,-109.769911858384,
173.485485069079));
#19193=CARTESIAN_POINT('',(-61.687965692515,-108.732160612486,173.485485069079));
#19194=CARTESIAN_POINT('Origin',(-58.6665129885927,-109.418884079281,173.485484935562));
#19195=CARTESIAN_POINT('Ctrl Pts',(-60.2062634500224,-108.645684644372,
173.485485069079));
#19196=CARTESIAN_POINT('Ctrl Pts',(-60.4535623858286,-108.645903327689,
173.485485069079));
#19197=CARTESIAN_POINT('Ctrl Pts',(-60.7017999171308,-108.655278077643,
173.485485069079));
#19198=CARTESIAN_POINT('Ctrl Pts',(-61.1897037647873,-108.685836758131,
173.485485069079));
#19199=CARTESIAN_POINT('Ctrl Pts',(-61.4418329283609,-108.70741980426,173.485485069079));
#19200=CARTESIAN_POINT('Ctrl Pts',(-61.687965692515,-108.732160612486,173.485485069079));
#19201=CARTESIAN_POINT('',(-61.5819596880668,-107.737795122829,173.485485069079));
#19202=CARTESIAN_POINT('Ctrl Pts',(-61.5819596880668,-107.737795122829,
173.485485069079));
#19203=CARTESIAN_POINT('Ctrl Pts',(-61.3542511675849,-107.829245182579,
173.485485069079));
#19204=CARTESIAN_POINT('Ctrl Pts',(-61.122813292609,-107.920622594452,173.485485070806));
#19205=CARTESIAN_POINT('Ctrl Pts',(-60.6443692583563,-108.103925343616,
173.485485070806));
#19206=CARTESIAN_POINT('Ctrl Pts',(-60.4028595604654,-108.194233824254,
173.485485069079));
#19207=CARTESIAN_POINT('Ctrl Pts',(-60.1671045752071,-108.278363623899,
173.485485069079));
#19208=CARTESIAN_POINT('',(-61.5289566858427,-107.240612378001,173.485485069079));
#19209=CARTESIAN_POINT('Origin',(-58.5075039863327,-107.927335844292,173.485484935562));
#19210=CARTESIAN_POINT('Ctrl Pts',(-60.0472544433501,-107.154136409886,
173.485485069079));
#19211=CARTESIAN_POINT('Ctrl Pts',(-60.2945500716139,-107.154355090279,
173.485485069079));
#19212=CARTESIAN_POINT('Ctrl Pts',(-60.542794229189,-107.163730051018,173.485485069079));
#19213=CARTESIAN_POINT('Ctrl Pts',(-61.0306947581148,-107.194288523646,
173.485485069079));
#19214=CARTESIAN_POINT('Ctrl Pts',(-61.282823921688,-107.215871569774,173.485485069079));
#19215=CARTESIAN_POINT('Ctrl Pts',(-61.5289566858427,-107.240612378001,
173.485485069079));
#19216=CARTESIAN_POINT('',(-61.4229506813946,-106.246246888344,173.485485069079));
#19217=CARTESIAN_POINT('Ctrl Pts',(-61.4229506813946,-106.246246888344,
173.485485069079));
#19218=CARTESIAN_POINT('Ctrl Pts',(-61.1952421609126,-106.337696948094,
173.485485069079));
#19219=CARTESIAN_POINT('Ctrl Pts',(-60.9638042859369,-106.429074359967,
173.485485070806));
#19220=CARTESIAN_POINT('Ctrl Pts',(-60.4853633505951,-106.612375921868,
173.485485070806));
#19221=CARTESIAN_POINT('Ctrl Pts',(-60.2438476026526,-106.702686642891,
173.485485069079));
#19222=CARTESIAN_POINT('Ctrl Pts',(-60.0080955685348,-106.786815389413,
173.485485069079));
#19223=CARTESIAN_POINT('',(-61.3699476791705,-105.749064143515,173.485485069079));
#19224=CARTESIAN_POINT('Origin',(-58.3484949741263,-106.435787610392,173.485484935551));
#19225=CARTESIAN_POINT('Ctrl Pts',(-59.8882454366779,-105.662588175401,
173.485485069079));
#19226=CARTESIAN_POINT('Ctrl Pts',(-60.1355410649418,-105.662806855793,
173.485485069079));
#19227=CARTESIAN_POINT('Ctrl Pts',(-60.3837852225172,-105.672181816532,
173.485485069079));
#19228=CARTESIAN_POINT('Ctrl Pts',(-60.8716857514425,-105.70274028916,173.485485069079));
#19229=CARTESIAN_POINT('Ctrl Pts',(-61.1238149150156,-105.724323335288,
173.485485069079));
#19230=CARTESIAN_POINT('Ctrl Pts',(-61.3699476791705,-105.749064143515,
173.485485069079));
#19231=CARTESIAN_POINT('',(-61.2639416747223,-104.754698653858,173.485485069079));
#19232=CARTESIAN_POINT('Ctrl Pts',(-61.2639416747223,-104.754698653858,
173.485485069079));
#19233=CARTESIAN_POINT('Ctrl Pts',(-61.0362331542402,-104.846148713608,
173.485485069079));
#19234=CARTESIAN_POINT('Ctrl Pts',(-60.8047952792646,-104.937526125481,
173.485485070806));
#19235=CARTESIAN_POINT('Ctrl Pts',(-60.3263543439242,-105.120827687381,
173.485485070806));
#19236=CARTESIAN_POINT('Ctrl Pts',(-60.0848385959808,-105.211138408405,
173.485485069079));
#19237=CARTESIAN_POINT('Ctrl Pts',(-59.8490865618626,-105.295267154927,
173.485485069079));
#19238=CARTESIAN_POINT('',(-61.2109386724983,-104.25751590903,173.485485069079));
#19239=CARTESIAN_POINT('Origin',(-58.189485943239,-104.944239379307,173.485484935551));
#19240=CARTESIAN_POINT('Ctrl Pts',(-59.7292364300057,-104.171039940915,
173.485485069079));
#19241=CARTESIAN_POINT('Ctrl Pts',(-59.9765353658119,-104.171258624233,
173.485485069079));
#19242=CARTESIAN_POINT('Ctrl Pts',(-60.2247728971142,-104.180633374186,
173.485485069079));
#19243=CARTESIAN_POINT('Ctrl Pts',(-60.7126767447704,-104.211192054675,
173.485485069079));
#19244=CARTESIAN_POINT('Ctrl Pts',(-60.9648059083435,-104.232775100803,
173.485485069079));
#19245=CARTESIAN_POINT('Ctrl Pts',(-61.2109386724983,-104.25751590903,173.485485069079));
#19246=CARTESIAN_POINT('',(-61.1049326680501,-103.263150419372,173.485485069079));
#19247=CARTESIAN_POINT('Ctrl Pts',(-61.1049326680501,-103.263150419373,
173.485485069079));
#19248=CARTESIAN_POINT('Ctrl Pts',(-60.8772241475705,-103.354600479122,
173.485485069079));
#19249=CARTESIAN_POINT('Ctrl Pts',(-60.6457862725931,-103.445977890995,
173.485485070806));
#19250=CARTESIAN_POINT('Ctrl Pts',(-60.167345337252,-103.629279452896,173.485485070806));
#19251=CARTESIAN_POINT('Ctrl Pts',(-59.9258295893085,-103.719590173919,
173.485485069079));
#19252=CARTESIAN_POINT('Ctrl Pts',(-59.6900775551904,-103.803718920442,
173.485485069079));
#19253=CARTESIAN_POINT('',(-61.0519296658261,-102.765967674544,173.485485069079));
#19254=CARTESIAN_POINT('Origin',(-58.0304769626648,-103.452691141352,173.485484935545));
#19255=CARTESIAN_POINT('Ctrl Pts',(-59.5702274233335,-102.679491706429,
173.485485069079));
#19256=CARTESIAN_POINT('Ctrl Pts',(-59.8175230515967,-102.679710386822,
173.485485069079));
#19257=CARTESIAN_POINT('Ctrl Pts',(-60.0657672091708,-102.689085347561,
173.485485069079));
#19258=CARTESIAN_POINT('Ctrl Pts',(-60.5536677380983,-102.719643820189,
173.485485069079));
#19259=CARTESIAN_POINT('Ctrl Pts',(-60.8057969016718,-102.741226866317,
173.485485069079));
#19260=CARTESIAN_POINT('Ctrl Pts',(-61.0519296658261,-102.765967674544,
173.485485069079));
#19261=CARTESIAN_POINT('',(-60.6425873069478,-101.892414120442,173.485485069077));
#19262=CARTESIAN_POINT('Ctrl Pts',(-60.642587306948,-101.892414120443,173.485485069079));
#19263=CARTESIAN_POINT('Ctrl Pts',(-60.4342503547387,-101.974634832253,
173.485485069079));
#19264=CARTESIAN_POINT('Ctrl Pts',(-60.2480095641541,-102.046444777389,
173.485485069079));
#19265=CARTESIAN_POINT('Ctrl Pts',(-59.8845339623614,-102.183752672436,
173.485485069079));
#19266=CARTESIAN_POINT('Ctrl Pts',(-59.7067146857557,-102.249490890159,
173.485485069079));
#19267=CARTESIAN_POINT('Ctrl Pts',(-59.5310685485181,-102.312170685956,
173.485485069079));
#19268=CARTESIAN_POINT('',(-60.9552496185426,-101.859082229163,173.485485069079));
#19269=CARTESIAN_POINT('',(-43.8144614293464,-103.686404765925,173.485485069079));
#19270=CARTESIAN_POINT('',(-54.5948893516535,-42.1971528497386,173.485485069079));
#19271=CARTESIAN_POINT('Ctrl Pts',(-57.259519543175,-112.30973612544,173.494068527883));
#19272=CARTESIAN_POINT('Ctrl Pts',(-55.9273079477605,-112.451758781876,
173.638013937363));
#19273=CARTESIAN_POINT('Ctrl Pts',(-55.9273079477605,-112.451758781876,
174.985485069079));
#19274=CARTESIAN_POINT('Ctrl Pts',(-57.2437226572379,-112.161556988779,
173.494068527878));
#19275=CARTESIAN_POINT('Ctrl Pts',(-55.9115340572459,-112.303795348611,
173.638013937322));
#19276=CARTESIAN_POINT('Ctrl Pts',(-55.9115340572464,-112.303795348611,
174.985485069038));
#19277=CARTESIAN_POINT('Ctrl Pts',(-57.2278898065789,-112.013381908907,
173.494068527883));
#19278=CARTESIAN_POINT('Ctrl Pts',(-55.8957243236821,-112.155836616448,
173.638013937363));
#19279=CARTESIAN_POINT('Ctrl Pts',(-55.8957243236832,-112.155836616448,
174.985485069079));
#19280=CARTESIAN_POINT('Ctrl Pts',(-57.2120207737176,-111.865210910606,
173.494068527883));
#19281=CARTESIAN_POINT('Ctrl Pts',(-55.879878531177,-112.007882616058,173.638013937363));
#19282=CARTESIAN_POINT('Ctrl Pts',(-55.879878531177,-112.007882616058,174.985485069079));
#19283=CARTESIAN_POINT('Ctrl Pts',(-57.2413645753253,-112.263285154288,
173.495537439996));
#19284=CARTESIAN_POINT('Ctrl Pts',(-57.2033140047626,-112.275892356383,
173.500095525992));
#19285=CARTESIAN_POINT('Ctrl Pts',(-57.1653918170167,-112.288244330645,
173.506200883917));
#19286=CARTESIAN_POINT('Ctrl Pts',(-57.0899544352199,-112.312424168425,
173.521506336905));
#19287=CARTESIAN_POINT('Ctrl Pts',(-57.0524790264818,-112.324239249128,
173.530698662253));
#19288=CARTESIAN_POINT('Ctrl Pts',(-57.0153382075498,-112.335767487168,
173.541420416595));
#19289=CARTESIAN_POINT('Ctrl Pts',(-55.8941531223023,-112.141258553931,
174.985485069071));
#19290=CARTESIAN_POINT('Ctrl Pts',(-55.8916773175805,-112.118109604864,
174.850935587984));
#19291=CARTESIAN_POINT('Ctrl Pts',(-55.9075132742012,-112.095933400872,
174.716548833312));
#19292=CARTESIAN_POINT('Ctrl Pts',(-55.9811754973074,-112.050187383497,
174.433829597845));
#19293=CARTESIAN_POINT('Ctrl Pts',(-56.0450398693184,-112.027296731103,
174.288799639065));
#19294=CARTESIAN_POINT('Ctrl Pts',(-56.1432872646253,-112.003471991653,
174.137658259513));
#19295=CARTESIAN_POINT('Ctrl Pts',(-56.1559725791695,-112.000546571712,
174.119092857142));
#19296=CARTESIAN_POINT('Ctrl Pts',(-56.1964158282439,-111.991665771564,
174.062734827425));
#19297=CARTESIAN_POINT('Ctrl Pts',(-56.2255745057671,-111.985870655016,
174.025962079021));
#19298=CARTESIAN_POINT('Ctrl Pts',(-56.3847089020071,-111.957140194668,
173.843960050512));
#19299=CARTESIAN_POINT('Ctrl Pts',(-56.5410272906302,-111.938298267507,
173.724180636921));
#19300=CARTESIAN_POINT('Ctrl Pts',(-56.8689932673701,-111.910937177978,
173.563255743881));
#19301=CARTESIAN_POINT('Ctrl Pts',(-57.0332189978765,-111.901459989199,
173.515132800414));
#19302=CARTESIAN_POINT('Ctrl Pts',(-57.2022249863543,-111.895960177099,
173.495524270213));
#19303=CARTESIAN_POINT('Origin',(-57.4101169644616,-112.210813934705,176.985487255437));
#19304=CARTESIAN_POINT('Ctrl Pts',(-57.0153371209007,-112.335767603012,
178.42954834513));
#19305=CARTESIAN_POINT('Ctrl Pts',(-56.8473564372785,-112.320853466685,
178.38305319844));
#19306=CARTESIAN_POINT('Ctrl Pts',(-56.6884637490847,-112.310226558581,
178.308320841682));
#19307=CARTESIAN_POINT('Ctrl Pts',(-56.4556453066853,-112.297678205632,
178.144602855094));
#19308=CARTESIAN_POINT('Ctrl Pts',(-56.3728898125372,-112.293947382744,
178.071756401203));
#19309=CARTESIAN_POINT('Ctrl Pts',(-56.2709933701936,-112.290154253653,
177.959937124381));
#19310=CARTESIAN_POINT('Ctrl Pts',(-56.2444363725251,-112.28925807319,177.928257007469));
#19311=CARTESIAN_POINT('Ctrl Pts',(-56.2046433208664,-112.288053998207,
177.876578050907));
#19312=CARTESIAN_POINT('Ctrl Pts',(-56.1905182651179,-112.287657594759,
177.857294323186));
#19313=CARTESIAN_POINT('Ctrl Pts',(-56.1744975949982,-112.287243742126,
177.834282953652));
#19314=CARTESIAN_POINT('Ctrl Pts',(-56.1721473696133,-112.287183975266,
177.830877075062));
#19315=CARTESIAN_POINT('Ctrl Pts',(-56.1684117420286,-112.287090485813,
177.825415042612));
#19316=CARTESIAN_POINT('Ctrl Pts',(-56.1670172505921,-112.287055927343,
177.823365146775));
#19317=CARTESIAN_POINT('Ctrl Pts',(-56.1645609823913,-112.286995657481,
177.819735019072));
#19318=CARTESIAN_POINT('Ctrl Pts',(-56.1634971100675,-112.286969754496,
177.818156215516));
#19319=CARTESIAN_POINT('Ctrl Pts',(-56.1613001770806,-112.286916680793,
177.814882425266));
#19320=CARTESIAN_POINT('Ctrl Pts',(-56.160167562911,-112.286889550508,177.813187143314));
#19321=CARTESIAN_POINT('Ctrl Pts',(-56.1572702675728,-112.286820743249,
177.808831200865));
#19322=CARTESIAN_POINT('Ctrl Pts',(-56.1555106437809,-112.286779523379,
177.806167182541));
#19323=CARTESIAN_POINT('Ctrl Pts',(-56.1483293226769,-112.286613629846,
177.795218581503));
#19324=CARTESIAN_POINT('Ctrl Pts',(-56.1429816031708,-112.286495587941,
177.786885698674));
#19325=CARTESIAN_POINT('Ctrl Pts',(-56.1089735505856,-112.285780346088,
177.732713914608));
#19326=CARTESIAN_POINT('Ctrl Pts',(-56.0827423503488,-112.285394420431,
177.685398052236));
#19327=CARTESIAN_POINT('Ctrl Pts',(-56.0139383163625,-112.284873827523,
177.543566166655));
#19328=CARTESIAN_POINT('Ctrl Pts',(-55.9786013530088,-112.285290965373,
177.445922321661));
#19329=CARTESIAN_POINT('Ctrl Pts',(-55.9245999086427,-112.287723313926,
177.227616441256));
#19330=CARTESIAN_POINT('Ctrl Pts',(-55.9100488748278,-112.289987551767,
177.106767079342));
#19331=CARTESIAN_POINT('Ctrl Pts',(-55.9103887977622,-112.293171089531,
176.985485076695));
#19332=CARTESIAN_POINT('Origin',(-69.5889371886705,15.3762068992854,178.485485069079));
#19333=CARTESIAN_POINT('Origin',(-53.4413942236179,-112.716773792997,178.485485069079));
#19334=CARTESIAN_POINT('',(-37.1738630900728,31.4290895869696,178.485485069079));
#19335=CARTESIAN_POINT('Origin',(-44.1060283439209,41.4682670878081,178.485485069079));
#19336=CARTESIAN_POINT('',(-41.1020539958444,25.42062214227,178.485485069079));
#19337=CARTESIAN_POINT('Origin',(-31.7758655563387,23.6116972707429,178.485485069079));
#19338=CARTESIAN_POINT('Origin',(-36.6843857876575,24.5637629925993,178.485485069079));
#19339=CARTESIAN_POINT('',(-26.3222158483506,41.9802195673193,178.485485069079));
#19340=CARTESIAN_POINT('Origin',(-60.1632027754914,33.6789365837495,178.485485069079));
#19341=CARTESIAN_POINT('',(-31.0667656272414,60.393115748013,179.845797336032));
#19342=CARTESIAN_POINT('',(-31.066765828848,60.3931158153939,172.125173944189));
#19343=CARTESIAN_POINT('',(-31.0667661651747,60.3931159007681,178.485485069079));
#19344=CARTESIAN_POINT('',(-28.9197092925293,57.8469757052857,178.485485069079));
#19345=CARTESIAN_POINT('Ctrl Pts',(-31.0667654102549,60.3931159213539,179.845797430829));
#19346=CARTESIAN_POINT('Ctrl Pts',(-30.9091769682086,60.2214795244379,179.79892929946));
#19347=CARTESIAN_POINT('Ctrl Pts',(-30.7556527061396,60.0512411160334,179.742114967035));
#19348=CARTESIAN_POINT('Ctrl Pts',(-30.6059165456662,59.8823450585327,179.676490357673));
#19349=CARTESIAN_POINT('Ctrl Pts',(-30.4442591103229,59.7000023070635,179.605641031689));
#19350=CARTESIAN_POINT('Ctrl Pts',(-30.2870169389526,59.5192241310761,179.524523032668));
#19351=CARTESIAN_POINT('Ctrl Pts',(-30.1338194315574,59.3399324111494,179.434622622711));
#19352=CARTESIAN_POINT('Ctrl Pts',(-30.0717866024173,59.267333497384,179.398220093288));
#19353=CARTESIAN_POINT('Ctrl Pts',(-30.010416692512,59.1949782192853,179.360378177063));
#19354=CARTESIAN_POINT('Ctrl Pts',(-29.949684172152,59.1228610766146,179.321197665583));
#19355=CARTESIAN_POINT('Ctrl Pts',(-29.9426383506173,59.1144944797101,179.316652178422));
#19356=CARTESIAN_POINT('Ctrl Pts',(-29.9356009897824,59.106130933026,179.312088584704));
#19357=CARTESIAN_POINT('Ctrl Pts',(-29.9285720599821,59.0977704247621,179.307506991655));
#19358=CARTESIAN_POINT('Ctrl Pts',(-29.6522634383716,58.7691171902053,179.127403662113));
#19359=CARTESIAN_POINT('Ctrl Pts',(-29.3887247237273,58.4448506261122,178.919335958335));
#19360=CARTESIAN_POINT('Ctrl Pts',(-29.1356651950541,58.1236205383787,178.68935857041));
#19361=CARTESIAN_POINT('Ctrl Pts',(-29.0628302196002,58.0311648791201,178.623167040329));
#19362=CARTESIAN_POINT('Ctrl Pts',(-28.9908632147143,57.9389607063399,178.55516084433));
#19363=CARTESIAN_POINT('Ctrl Pts',(-28.9197092925293,57.8469757052856,178.485485069079));
#19364=CARTESIAN_POINT('',(-27.6932740952942,56.17235187585,177.985895857994));
#19365=CARTESIAN_POINT('Ctrl Pts',(-28.9197092925293,57.8469757052856,178.485485069079));
#19366=CARTESIAN_POINT('Ctrl Pts',(-28.8695639852542,57.7821498179569,178.4363815229));
#19367=CARTESIAN_POINT('Ctrl Pts',(-28.8180944967583,57.7151863974902,178.393590440407));
#19368=CARTESIAN_POINT('Ctrl Pts',(-28.765769451896,57.6466415487446,178.35528260832));
#19369=CARTESIAN_POINT('Ctrl Pts',(-28.7186055717574,57.5848577310937,178.320753330693));
#19370=CARTESIAN_POINT('Ctrl Pts',(-28.6707461547263,57.5217885156425,178.289868104488));
#19371=CARTESIAN_POINT('Ctrl Pts',(-28.6225281965413,57.4578315766418,178.261313090149));
#19372=CARTESIAN_POINT('Ctrl Pts',(-28.6223170910684,57.4575515635438,178.261188072002));
#19373=CARTESIAN_POINT('Ctrl Pts',(-28.6221059794197,57.4572715343512,178.261063099026));
#19374=CARTESIAN_POINT('Ctrl Pts',(-28.6218948616221,57.4569914890959,178.260938171111));
#19375=CARTESIAN_POINT('Ctrl Pts',(-28.5576206106114,57.3717324572002,178.222904200128));
#19376=CARTESIAN_POINT('Ctrl Pts',(-28.4924136963644,57.2845038762807,178.18938357879));
#19377=CARTESIAN_POINT('Ctrl Pts',(-28.4269389977876,57.1961490995419,178.159893050851));
#19378=CARTESIAN_POINT('Ctrl Pts',(-28.3890105999134,57.1449666550392,178.142809681222));
#19379=CARTESIAN_POINT('Ctrl Pts',(-28.3509920646441,57.0934057548245,178.12707974697));
#19380=CARTESIAN_POINT('Ctrl Pts',(-28.313012572032,57.0416287203634,178.112616869885));
#19381=CARTESIAN_POINT('Ctrl Pts',(-28.3124798542368,57.0409024719134,178.112414006933));
#19382=CARTESIAN_POINT('Ctrl Pts',(-28.3119471450267,57.0401761821527,178.112211393752));
#19383=CARTESIAN_POINT('Ctrl Pts',(-28.3114144448134,57.0394498516033,178.11200903013));
#19384=CARTESIAN_POINT('Ctrl Pts',(-28.1791184150512,56.8590657526497,178.061752050421));
#19385=CARTESIAN_POINT('Ctrl Pts',(-28.0471800611791,56.6759576351996,178.026148692935));
#19386=CARTESIAN_POINT('Ctrl Pts',(-27.9156412222414,56.4900036591952,178.005762137669));
#19387=CARTESIAN_POINT('Ctrl Pts',(-27.8413887382427,56.3850343228436,177.994254111744));
#19388=CARTESIAN_POINT('Ctrl Pts',(-27.7672636383413,56.2791580302122,177.987595826179));
#19389=CARTESIAN_POINT('Ctrl Pts',(-27.6932740952942,56.1723518758501,177.985895857994));
#19390=CARTESIAN_POINT('Ctrl Pts',(-27.6932740952942,56.17235187585,177.985895857994));
#19391=CARTESIAN_POINT('Ctrl Pts',(-27.681334674434,56.1551169589298,177.985621541128));
#19392=CARTESIAN_POINT('Ctrl Pts',(-27.6694076934204,56.137870682049,177.985485069079));
#19393=CARTESIAN_POINT('Ctrl Pts',(-27.6574947146374,56.1206152968612,177.985485069079));
#19394=CARTESIAN_POINT('',(-27.6932740952942,56.1723518758501,173.985074280165));
#19395=CARTESIAN_POINT('Ctrl Pts',(-27.6574947146374,56.1206152968612,173.985485069079));
#19396=CARTESIAN_POINT('Ctrl Pts',(-27.6694076934205,56.137870682049,173.985485069079));
#19397=CARTESIAN_POINT('Ctrl Pts',(-27.681334674434,56.1551169589298,173.985348597031));
#19398=CARTESIAN_POINT('Ctrl Pts',(-27.6932740952942,56.1723518758501,173.985074280165));
#19399=CARTESIAN_POINT('',(-28.9197092925293,57.8469757052857,173.485485069079));
#19400=CARTESIAN_POINT('Ctrl Pts',(-27.6932740952942,56.1723518758501,173.985074280165));
#19401=CARTESIAN_POINT('Ctrl Pts',(-27.8243471320476,56.3615597884776,173.98206277363));
#19402=CARTESIAN_POINT('Ctrl Pts',(-27.9558453121505,56.547849976542,173.963493852483));
#19403=CARTESIAN_POINT('Ctrl Pts',(-28.0877242229479,56.7313482308063,173.929959739527));
#19404=CARTESIAN_POINT('Ctrl Pts',(-28.1621686748946,56.8349313351047,173.91103003617));
#19405=CARTESIAN_POINT('Ctrl Pts',(-28.236734533152,56.9376246600296,173.887330718302));
#19406=CARTESIAN_POINT('Ctrl Pts',(-28.3114144448134,57.0394498516033,173.858961108029));
#19407=CARTESIAN_POINT('Ctrl Pts',(-28.3119471450267,57.0401761821527,173.858758744407));
#19408=CARTESIAN_POINT('Ctrl Pts',(-28.3124798542368,57.0409024719135,173.858556131226));
#19409=CARTESIAN_POINT('Ctrl Pts',(-28.313012572032,57.0416287203635,173.858353268274));
#19410=CARTESIAN_POINT('Ctrl Pts',(-28.3785754740065,57.1310099206225,173.833386420974));
#19411=CARTESIAN_POINT('Ctrl Pts',(-28.4442544486703,57.2197472411231,173.80464629479));
#19412=CARTESIAN_POINT('Ctrl Pts',(-28.5093860560218,57.3070049527639,173.77167881297));
#19413=CARTESIAN_POINT('Ctrl Pts',(-28.5471157068459,57.3575518857476,173.752581302127));
#19414=CARTESIAN_POINT('Ctrl Pts',(-28.5846618629718,57.4076023578408,173.732064410334));
#19415=CARTESIAN_POINT('Ctrl Pts',(-28.6218948616218,57.4569914890955,173.710031967047));
#19416=CARTESIAN_POINT('Ctrl Pts',(-28.6221059794194,57.4572715343509,173.709907039132));
#19417=CARTESIAN_POINT('Ctrl Pts',(-28.6223170910682,57.4575515635435,173.709782066156));
#19418=CARTESIAN_POINT('Ctrl Pts',(-28.622528196541,57.4578315766415,173.709657048009));
#19419=CARTESIAN_POINT('Ctrl Pts',(-28.6793546949681,57.5332069975494,173.676003995527));
#19420=CARTESIAN_POINT('Ctrl Pts',(-28.7356833945105,57.6073497472281,173.639115263873));
#19421=CARTESIAN_POINT('Ctrl Pts',(-28.7909620326999,57.6796078112931,173.596837451893));
#19422=CARTESIAN_POINT('Ctrl Pts',(-28.8346253447626,57.7366827773859,173.563443190417));
#19423=CARTESIAN_POINT('Ctrl Pts',(-28.8776335649023,57.7925818541628,173.526686679897));
#19424=CARTESIAN_POINT('Ctrl Pts',(-28.9197092925293,57.8469757052856,173.485485069079));
#19425=CARTESIAN_POINT('Ctrl Pts',(-28.9197092925293,57.8469757052857,173.485485069079));
#19426=CARTESIAN_POINT('Ctrl Pts',(-29.0790134324243,58.0529178519195,173.329490304359));
#19427=CARTESIAN_POINT('Ctrl Pts',(-29.2423834600949,58.2599171593523,173.181896823521));
#19428=CARTESIAN_POINT('Ctrl Pts',(-29.410398257058,58.4683499340291,173.044312541129));
#19429=CARTESIAN_POINT('Ctrl Pts',(-29.5682295040916,58.6641493835094,172.915067383829));
#19430=CARTESIAN_POINT('Ctrl Pts',(-29.7301598671435,58.8612136717954,172.79465486008));
#19431=CARTESIAN_POINT('Ctrl Pts',(-29.8967040919158,59.0598163446466,172.684407875314));
#19432=CARTESIAN_POINT('Ctrl Pts',(-29.9074498185088,59.0726305387503,172.677294545761));
#19433=CARTESIAN_POINT('Ctrl Pts',(-29.9182147646746,59.0854511235265,172.670223535932));
#19434=CARTESIAN_POINT('Ctrl Pts',(-29.9289990735725,59.0982781667031,172.663195203856));
#19435=CARTESIAN_POINT('Ctrl Pts',(-30.0800102141939,59.2778934243173,172.564778471406));
#19436=CARTESIAN_POINT('Ctrl Pts',(-30.2348076625985,59.4587693147239,172.474706081542));
#19437=CARTESIAN_POINT('Ctrl Pts',(-30.3939297630228,59.6412243163263,172.394408698027));
#19438=CARTESIAN_POINT('Ctrl Pts',(-30.5498223183852,59.8199762078775,172.315741031677));
#19439=CARTESIAN_POINT('Ctrl Pts',(-30.7098658175238,60.0002439081216,172.246455610862));
#19440=CARTESIAN_POINT('Ctrl Pts',(-30.8745987125149,60.1822886744227,172.187897745043));
#19441=CARTESIAN_POINT('Ctrl Pts',(-30.9379500098726,60.25229759476,172.165378157985));
#19442=CARTESIAN_POINT('Ctrl Pts',(-31.0019951796934,60.3225689131167,172.14444511125));
#19443=CARTESIAN_POINT('Ctrl Pts',(-31.0667661288183,60.3931158611695,172.125175120043));
#19444=CARTESIAN_POINT('Origin',(-13.1705752052125,56.1246475259002,178.485485069079));
#19445=CARTESIAN_POINT('',(-34.8117175582729,61.2863342745896,179.985485069079));
#19446=CARTESIAN_POINT('',(-31.0975708454296,60.4004632081127,179.985485069769));
#19447=CARTESIAN_POINT('',(-13.1705752052126,56.1246475259002,179.985485069079));
#19448=CARTESIAN_POINT('Ctrl Pts',(-31.0975708439929,60.4004632071099,179.985485070495));
#19449=CARTESIAN_POINT('Ctrl Pts',(-31.0877379564735,60.3981179388064,179.962800941576));
#19450=CARTESIAN_POINT('Ctrl Pts',(-31.0798430692015,60.3962349080896,179.939231997035));
#19451=CARTESIAN_POINT('Ctrl Pts',(-31.0694893305528,60.3937654101902,179.892276273643));
#19452=CARTESIAN_POINT('Ctrl Pts',(-31.0667653038197,60.393115695324,179.869118012909));
#19453=CARTESIAN_POINT('Ctrl Pts',(-31.0667651743783,60.3931156644506,179.845797336034));
#19454=CARTESIAN_POINT('',(-31.0975708454298,60.4004632081127,171.98548506839));
#19455=CARTESIAN_POINT('Ctrl Pts',(-31.0667651743779,60.3931156644505,172.125172868157));
#19456=CARTESIAN_POINT('Ctrl Pts',(-31.0667652986773,60.3931156940975,172.101852061251));
#19457=CARTESIAN_POINT('Ctrl Pts',(-31.0694893609766,60.3937654174737,172.078693606888));
#19458=CARTESIAN_POINT('Ctrl Pts',(-31.0798431515216,60.3962349277511,172.031737895439));
#19459=CARTESIAN_POINT('Ctrl Pts',(-31.0877380076616,60.3981179510155,172.008169078495));
#19460=CARTESIAN_POINT('Ctrl Pts',(-31.0975708439932,60.4004632071099,171.985485067664));
#19461=CARTESIAN_POINT('',(-34.8117175582729,61.2863342745896,171.985485069079));
#19462=CARTESIAN_POINT('',(-13.1705752052126,56.1246475259002,171.985485069079));
#19463=CARTESIAN_POINT('',(-34.8117175582729,61.2863342745896,178.485485069079));
#19464=CARTESIAN_POINT('Origin',(-13.5112392801691,-107.683134251892,178.485485069079));
#19465=CARTESIAN_POINT('',(-34.5615750673481,59.3020387486575,171.985485069079));
#19466=CARTESIAN_POINT('',(-34.5615750673481,59.3020387486575,179.985485069079));
#19467=CARTESIAN_POINT('',(-34.5615750673481,59.3020387486575,165.645237852233));
#19468=CARTESIAN_POINT('',(-13.511239280169,-107.683134251892,179.985485069079));
#19469=CARTESIAN_POINT('',(-13.511239280169,-107.683134251892,171.985485069079));
#19470=CARTESIAN_POINT('Origin',(-44.1060283439209,41.4682670878081,178.485485069079));
#19471=CARTESIAN_POINT('',(-33.3398524910169,36.8879333106141,171.985485068901));
#19472=CARTESIAN_POINT('',(-32.4060870603391,41.4312001114371,171.985485069079));
#19473=CARTESIAN_POINT('Origin',(-44.1060283439209,41.4682670878081,171.985485069079));
#19474=CARTESIAN_POINT('',(-33.7101944105682,36.1001541204655,173.485485069079));
#19475=CARTESIAN_POINT('Ctrl Pts',(-33.3398524911435,36.8879333109887,171.985485069079));
#19476=CARTESIAN_POINT('Ctrl Pts',(-33.4532592756956,36.621368155505,172.485877932252));
#19477=CARTESIAN_POINT('Ctrl Pts',(-33.5767107475439,36.3586572484842,172.985815014066));
#19478=CARTESIAN_POINT('Ctrl Pts',(-33.7101944105682,36.1001541204655,173.485485069079));
#19479=CARTESIAN_POINT('',(-34.1412494001895,35.3369392868692,173.985485069079));
#19480=CARTESIAN_POINT('Ctrl Pts',(-33.7101944105682,36.1001541204655,173.485485069079));
#19481=CARTESIAN_POINT('Ctrl Pts',(-33.7173223371263,36.0863502491167,173.512167058454));
#19482=CARTESIAN_POINT('Ctrl Pts',(-33.7250068081281,36.0715415783123,173.53788693616));
#19483=CARTESIAN_POINT('Ctrl Pts',(-33.7332256693475,36.0557977306796,173.56269943543));
#19484=CARTESIAN_POINT('Ctrl Pts',(-33.7415673687971,36.0398185771658,173.587882779689));
#19485=CARTESIAN_POINT('Ctrl Pts',(-33.7504597671664,36.0228754836816,173.612131975538));
#19486=CARTESIAN_POINT('Ctrl Pts',(-33.7599017013052,36.0050016280506,173.635474291225));
#19487=CARTESIAN_POINT('Ctrl Pts',(-33.7672835911654,35.9910274960872,173.65372377284));
#19488=CARTESIAN_POINT('Ctrl Pts',(-33.7750018538206,35.9764835561052,173.671418424909));
#19489=CARTESIAN_POINT('Ctrl Pts',(-33.7830638223894,35.9613727471357,173.688555375548));
#19490=CARTESIAN_POINT('Ctrl Pts',(-33.7891998689,35.9498717562971,173.701598483478));
#19491=CARTESIAN_POINT('Ctrl Pts',(-33.7955340084333,35.9380444037457,173.714314450847));
#19492=CARTESIAN_POINT('Ctrl Pts',(-33.80205321792,35.9259228315441,173.726665343328));
#19493=CARTESIAN_POINT('Ctrl Pts',(-33.8040994034126,35.9221182314254,173.730541920246));
#19494=CARTESIAN_POINT('Ctrl Pts',(-33.8061638904978,35.9182845158034,173.734382709747));
#19495=CARTESIAN_POINT('Ctrl Pts',(-33.8082463328237,35.9144225718301,173.738186738285));
#19496=CARTESIAN_POINT('Ctrl Pts',(-33.8216183462776,35.889623821763,173.762613595228));
#19497=CARTESIAN_POINT('Ctrl Pts',(-33.8357333107594,35.8636566094212,173.785523526798));
#19498=CARTESIAN_POINT('Ctrl Pts',(-33.8504811981783,35.8367881814026,173.80666357432));
#19499=CARTESIAN_POINT('Ctrl Pts',(-33.8619180624397,35.8159519385266,173.823057505676));
#19500=CARTESIAN_POINT('Ctrl Pts',(-33.8737350879047,35.7945745828219,173.838387610758));
#19501=CARTESIAN_POINT('Ctrl Pts',(-33.8858739421569,35.7727914017629,173.852553342878));
#19502=CARTESIAN_POINT('Ctrl Pts',(-33.8864939107968,35.7716788676759,173.853276830407));
#19503=CARTESIAN_POINT('Ctrl Pts',(-33.887114918358,35.7705649165669,173.853997532403));
#19504=CARTESIAN_POINT('Ctrl Pts',(-33.8877369560626,35.7694495689522,173.854715427453));
#19505=CARTESIAN_POINT('Ctrl Pts',(-33.9011175249542,35.7454574773375,173.870157970747));
#19506=CARTESIAN_POINT('Ctrl Pts',(-33.9150376519582,35.7207195066863,173.884371926662));
#19507=CARTESIAN_POINT('Ctrl Pts',(-33.9293809697622,35.6954582180761,173.89723673113));
#19508=CARTESIAN_POINT('Ctrl Pts',(-33.9342982268056,35.6867980007511,173.901647115899));
#19509=CARTESIAN_POINT('Ctrl Pts',(-33.9392650649815,35.6780764980385,173.905899303386));
#19510=CARTESIAN_POINT('Ctrl Pts',(-33.9442763474657,35.6693032844709,173.909989611581));
#19511=CARTESIAN_POINT('Ctrl Pts',(-33.9595076554056,35.642637951217,173.922421707334));
#19512=CARTESIAN_POINT('Ctrl Pts',(-33.9751531092322,35.6154891438031,173.933361803908));
#19513=CARTESIAN_POINT('Ctrl Pts',(-33.9910791468951,35.588102646381,173.942754134747));
#19514=CARTESIAN_POINT('Ctrl Pts',(-33.9982885995841,35.5757052339386,173.947005886893));
#19515=CARTESIAN_POINT('Ctrl Pts',(-34.0055541831447,35.5632613568449,173.950940413097));
#19516=CARTESIAN_POINT('Ctrl Pts',(-34.0128674167925,35.5507867018521,173.954557379261));
#19517=CARTESIAN_POINT('Ctrl Pts',(-34.0279475134156,35.5250636070225,173.962015666779));
#19518=CARTESIAN_POINT('Ctrl Pts',(-34.0432386359242,35.4991945765188,173.968132509407));
#19519=CARTESIAN_POINT('Ctrl Pts',(-34.0587493304729,35.4731802876461,173.972914111171));
#19520=CARTESIAN_POINT('Ctrl Pts',(-34.0739448242849,35.4476946484089,173.977598543567));
#19521=CARTESIAN_POINT('Ctrl Pts',(-34.0893515965258,35.4220686096455,173.98100154487));
#19522=CARTESIAN_POINT('Ctrl Pts',(-34.1049834076364,35.3963015527894,173.983080513186));
#19523=CARTESIAN_POINT('Ctrl Pts',(-34.1169386417112,35.3765948665997,173.984670511471));
#19524=CARTESIAN_POINT('Ctrl Pts',(-34.1290254559346,35.35680593016,173.985485066055));
#19525=CARTESIAN_POINT('Ctrl Pts',(-34.1412494001895,35.3369392868692,173.985485069079));
#19526=CARTESIAN_POINT('',(-37.4579682234273,31.8405312878237,173.985485069079));
#19527=CARTESIAN_POINT('Origin',(-44.1060283439209,41.4682670878081,173.985485069079));
#19528=CARTESIAN_POINT('',(-37.4579682234273,31.8405312878237,177.985485069079));
#19529=CARTESIAN_POINT('',(-37.4579682234273,31.8405312878237,178.485485069079));
#19530=CARTESIAN_POINT('',(-34.1412494001895,35.3369392868692,177.985485069079));
#19531=CARTESIAN_POINT('Origin',(-44.1060283439209,41.4682670878081,177.985485069079));
#19532=CARTESIAN_POINT('',(-33.7101944105682,36.1001541204655,178.485485069079));
#19533=CARTESIAN_POINT('Ctrl Pts',(-34.1412494001895,35.3369392868692,177.985485069079));
#19534=CARTESIAN_POINT('Ctrl Pts',(-34.1216095524896,35.3688584318198,177.98548506929));
#19535=CARTESIAN_POINT('Ctrl Pts',(-34.1022530974808,35.4006888588025,177.987571320185));
#19536=CARTESIAN_POINT('Ctrl Pts',(-34.0832209590391,35.4323178174378,177.991637372604));
#19537=CARTESIAN_POINT('Ctrl Pts',(-34.0638728223472,35.4644719243962,177.995770935327));
#19538=CARTESIAN_POINT('Ctrl Pts',(-34.0448594190002,35.496418670158,178.001950696189));
#19539=CARTESIAN_POINT('Ctrl Pts',(-34.026224496512,35.5280487026682,178.010118542669));
#19540=CARTESIAN_POINT('Ctrl Pts',(-34.0212915827807,35.5364215961852,178.012280681099));
#19541=CARTESIAN_POINT('Ctrl Pts',(-34.0163852148609,35.544772305989,178.014582413863));
#19542=CARTESIAN_POINT('Ctrl Pts',(-34.0115062740386,35.5530987904069,178.017023265722));
#19543=CARTESIAN_POINT('Ctrl Pts',(-34.007479623835,35.5599707409795,178.01903773095));
#19544=CARTESIAN_POINT('Ctrl Pts',(-34.0034718839124,35.5668257850579,178.021146733784));
#19545=CARTESIAN_POINT('Ctrl Pts',(-33.999477173576,35.5736737697792,178.023353970292));
#19546=CARTESIAN_POINT('Ctrl Pts',(-33.9833988783172,35.6012361988427,178.032237868573));
#19547=CARTESIAN_POINT('Ctrl Pts',(-33.9675632094865,35.6286311820355,178.042702346422));
#19548=CARTESIAN_POINT('Ctrl Pts',(-33.9521138058932,35.6555970548587,178.054698671223));
#19549=CARTESIAN_POINT('Ctrl Pts',(-33.9494502518773,35.6602461054461,178.056766897282));
#19550=CARTESIAN_POINT('Ctrl Pts',(-33.9467981555019,35.6648824218227,178.058880533764));
#19551=CARTESIAN_POINT('Ctrl Pts',(-33.9441582204118,35.6695046945796,178.061039180225));
#19552=CARTESIAN_POINT('Ctrl Pts',(-33.9297962098085,35.6946511955657,178.072782841451));
#19553=CARTESIAN_POINT('Ctrl Pts',(-33.9157941348307,35.7193826009939,178.085866381542));
#19554=CARTESIAN_POINT('Ctrl Pts',(-33.9022674318341,35.7434803909662,178.100186584167));
#19555=CARTESIAN_POINT('Ctrl Pts',(-33.8973136760764,35.7523054953435,178.105430935745));
#19556=CARTESIAN_POINT('Ctrl Pts',(-33.892423522062,35.7610458255236,178.110840715817));
#19557=CARTESIAN_POINT('Ctrl Pts',(-33.8876020576637,35.769691455901,178.116409398955));
#19558=CARTESIAN_POINT('Ctrl Pts',(-33.8869772780581,35.7708117822357,178.117131005373));
#19559=CARTESIAN_POINT('Ctrl Pts',(-33.8863535630653,35.7719306524527,178.117855401103));
#19560=CARTESIAN_POINT('Ctrl Pts',(-33.8857309216736,35.7730480455806,178.118582564087));
#19561=CARTESIAN_POINT('Ctrl Pts',(-33.8698601234795,35.8015298026145,178.137117562145));
#19562=CARTESIAN_POINT('Ctrl Pts',(-33.8545548409672,35.829289317426,178.157619748358));
#19563=CARTESIAN_POINT('Ctrl Pts',(-33.8399353901162,35.8560417099049,178.179865523891));
#19564=CARTESIAN_POINT('Ctrl Pts',(-33.8374692589998,35.8605545269871,178.183618127173));
#19565=CARTESIAN_POINT('Ctrl Pts',(-33.835022606309,35.8650387401053,178.187420245313));
#19566=CARTESIAN_POINT('Ctrl Pts',(-33.8325959619353,35.8694930537462,178.191270687453));
#19567=CARTESIAN_POINT('Ctrl Pts',(-33.8199869512839,35.8926379730227,178.211277848981));
#19568=CARTESIAN_POINT('Ctrl Pts',(-33.8079193627232,35.9149734889198,178.232590487925));
#19569=CARTESIAN_POINT('Ctrl Pts',(-33.7964576639897,35.9363350562286,178.255037515312));
#19570=CARTESIAN_POINT('Ctrl Pts',(-33.7900321528711,35.9483105051952,178.26762148104));
#19571=CARTESIAN_POINT('Ctrl Pts',(-33.7837965875609,35.9599807277839,178.280562417347));
#19572=CARTESIAN_POINT('Ctrl Pts',(-33.7777632759112,35.9713148162947,178.293822172451));
#19573=CARTESIAN_POINT('Ctrl Pts',(-33.7675348173914,35.9905298446117,178.31630184248));
#19574=CARTESIAN_POINT('Ctrl Pts',(-33.7578783351679,36.0087958173318,178.339710187513));
#19575=CARTESIAN_POINT('Ctrl Pts',(-33.7487823904955,36.0260993702412,178.364051408715));
#19576=CARTESIAN_POINT('Ctrl Pts',(-33.7398557276015,36.0430808921452,178.387939623072));
#19577=CARTESIAN_POINT('Ctrl Pts',(-33.7314687603436,36.0591360073105,178.412726903841));
#19578=CARTESIAN_POINT('Ctrl Pts',(-33.7236293478618,36.0742203564055,178.438450236595));
#19579=CARTESIAN_POINT('Ctrl Pts',(-33.7189541482838,36.0832162272936,178.453790890593));
#19580=CARTESIAN_POINT('Ctrl Pts',(-33.7144740589414,36.091866196189,178.469465048149));
#19581=CARTESIAN_POINT('Ctrl Pts',(-33.7101944105682,36.1001541204655,178.485485069079));
#19582=CARTESIAN_POINT('',(-33.3398524910169,36.8879333106141,179.985485069258));
#19583=CARTESIAN_POINT('Ctrl Pts',(-33.7101944105682,36.1001541204655,178.485485069079));
#19584=CARTESIAN_POINT('Ctrl Pts',(-33.5767107475439,36.3586572484842,178.985155124093));
#19585=CARTESIAN_POINT('Ctrl Pts',(-33.4532592756956,36.621368155505,179.485092205907));
#19586=CARTESIAN_POINT('Ctrl Pts',(-33.3398524911435,36.8879333109887,179.985485069079));
#19587=CARTESIAN_POINT('',(-32.4060870603391,41.431200111437,179.985485069079));
#19588=CARTESIAN_POINT('Origin',(-44.1060283439209,41.4682670878081,179.985485069079));
#19589=CARTESIAN_POINT('',(-32.4060870603391,41.431200111437,178.485485069079));
#19590=CARTESIAN_POINT('Origin',(-53.4413942236179,-112.716773792997,179.985485069079));
#19591=CARTESIAN_POINT('Ctrl Pts',(-33.3398524907636,36.8879333098646,179.985485069079));
#19592=CARTESIAN_POINT('Ctrl Pts',(-33.3574892950243,36.8464776027502,179.985485069079));
#19593=CARTESIAN_POINT('Ctrl Pts',(-33.3710414244414,36.8032694853988,179.985485069083));
#19594=CARTESIAN_POINT('Ctrl Pts',(-33.3899087453465,36.7118220614565,179.985485069083));
#19595=CARTESIAN_POINT('Ctrl Pts',(-33.3945539764798,36.6634335677105,179.985485069079));
#19596=CARTESIAN_POINT('Ctrl Pts',(-33.3922298082537,36.5460366143256,179.985485069079));
#19597=CARTESIAN_POINT('Ctrl Pts',(-33.3793951963956,36.4773565513148,179.985485069079));
#19598=CARTESIAN_POINT('Ctrl Pts',(-33.3300887502201,36.3532182089249,179.985485069079));
#19599=CARTESIAN_POINT('Ctrl Pts',(-33.2955167311449,36.2981567358835,179.985485069079));
#19600=CARTESIAN_POINT('Ctrl Pts',(-33.2141725090471,36.2148346472178,179.985485069079));
#19601=CARTESIAN_POINT('Ctrl Pts',(-33.1719475707044,36.184379905615,179.985485069079));
#19602=CARTESIAN_POINT('Ctrl Pts',(-33.0822769881238,36.1419052727305,179.985485069079));
#19603=CARTESIAN_POINT('Ctrl Pts',(-33.0367157125635,36.1289877482769,179.985485069079));
#19604=CARTESIAN_POINT('Ctrl Pts',(-32.9897426468184,36.123524749977,179.985485069079));
#19605=CARTESIAN_POINT('',(-29.2214842185525,55.7467898368407,179.985485069079));
#19606=CARTESIAN_POINT('',(-8.69585033055052,-107.076100989514,179.985485069079));
#19607=CARTESIAN_POINT('',(-30.7570310015667,59.9437472274033,179.985510844164));
#19608=CARTESIAN_POINT('Origin',(-39.1429618482127,54.4960773822167,179.985485069079));
#19609=CARTESIAN_POINT('Ctrl Pts',(-30.757020815632,59.9437588539596,179.985485069079));
#19610=CARTESIAN_POINT('Ctrl Pts',(-30.8085788556864,60.0230926458723,179.985485069079));
#19611=CARTESIAN_POINT('Ctrl Pts',(-30.8639970094185,60.1012773870114,179.98548506805));
#19612=CARTESIAN_POINT('Ctrl Pts',(-30.9777147231709,60.2527014471581,179.98548506805));
#19613=CARTESIAN_POINT('Ctrl Pts',(-31.0371822006902,60.3274835122335,179.985485069079));
#19614=CARTESIAN_POINT('Ctrl Pts',(-31.097570844777,60.4004632086527,179.985485069079));
#19615=CARTESIAN_POINT('',(-33.4443560589197,58.4349622311539,179.985485069079));
#19616=CARTESIAN_POINT('',(36.9742820842401,3.78287784314388,179.985485069079));
#19617=CARTESIAN_POINT('',(-34.3114325764233,57.3177432227255,179.985485069079));
#19618=CARTESIAN_POINT('',(-123.860032366778,-58.0646894049869,179.985485069079));
#19619=CARTESIAN_POINT('',(-33.1942135679949,56.4506667052219,179.985485069079));
#19620=CARTESIAN_POINT('',(36.1072055667355,2.66565883471801,179.985485069079));
#19621=CARTESIAN_POINT('',(-34.0612900854985,55.3334476967935,179.985485069079));
#19622=CARTESIAN_POINT('',(-122.742813358349,-58.9317659224909,179.985485069079));
#19623=CARTESIAN_POINT('',(-32.94407107707,54.4663711792899,179.985485069079));
#19624=CARTESIAN_POINT('',(35.240129049233,1.54843982628677,179.985485069079));
#19625=CARTESIAN_POINT('',(-33.8111475945737,53.3491521708615,179.985485069079));
#19626=CARTESIAN_POINT('',(-121.625594349921,-59.7988424399945,179.985485069079));
#19627=CARTESIAN_POINT('',(-32.6939285861452,52.4820756533578,179.985485069079));
#19628=CARTESIAN_POINT('',(34.3730525317294,0.43122081785836,179.985485069079));
#19629=CARTESIAN_POINT('',(-33.5610051036489,51.3648566449294,179.985485069079));
#19630=CARTESIAN_POINT('',(-120.508375341492,-60.6659189574982,179.985485069079));
#19631=CARTESIAN_POINT('',(-32.4437860952204,50.4977801274258,179.985485069079));
#19632=CARTESIAN_POINT('',(33.5059760142258,-0.685998190570039,179.985485069079));
#19633=CARTESIAN_POINT('',(-33.3108626127241,49.3805611189974,179.985485069079));
#19634=CARTESIAN_POINT('',(-119.391156333064,-61.5329954750018,179.985485069079));
#19635=CARTESIAN_POINT('',(-32.1936436042956,48.5134846014937,179.985485069079));
#19636=CARTESIAN_POINT('',(32.6388994967221,-1.80321719899848,179.985485069079));
#19637=CARTESIAN_POINT('',(-33.0607201217992,47.3962655930653,179.985485069079));
#19638=CARTESIAN_POINT('',(-118.273937324635,-62.4000719925054,179.985485069079));
#19639=CARTESIAN_POINT('',(-31.9435011133708,46.5291890755617,179.985485069079));
#19640=CARTESIAN_POINT('',(31.7718229792185,-2.92043620742687,179.985485069079));
#19641=CARTESIAN_POINT('',(-32.8105776308745,45.4119700671332,179.985485069079));
#19642=CARTESIAN_POINT('',(-117.156718316207,-63.267148510009,179.985485069079));
#19643=CARTESIAN_POINT('',(-31.693358622446,44.5448935496296,179.985485069079));
#19644=CARTESIAN_POINT('',(30.9047464617149,-4.03765521585528,179.985485069079));
#19645=CARTESIAN_POINT('',(-32.5604351399496,43.4276745412012,179.985485069079));
#19646=CARTESIAN_POINT('',(-116.039499307778,-64.1342250275126,179.985485069079));
#19647=CARTESIAN_POINT('',(-31.4432161315212,42.5605980236976,179.985485069079));
#19648=CARTESIAN_POINT('',(30.0376699442113,-5.15487422428371,179.985485069079));
#19649=CARTESIAN_POINT('',(-32.3102926490249,41.4433790152692,179.985485069079));
#19650=CARTESIAN_POINT('',(-114.92228029935,-65.0013015450162,179.985485069079));
#19651=CARTESIAN_POINT('',(-72.3928015643781,36.3474552058043,179.985485069079));
#19652=CARTESIAN_POINT('Origin',(-8.69585033055052,-107.076100989514,179.985485069079));
#19653=CARTESIAN_POINT('',(-28.5054632460221,55.8370522333852,178.735485069079));
#19654=CARTESIAN_POINT('',(-28.5054632460221,55.8370522333853,178.735485069079));
#19655=CARTESIAN_POINT('',(-29.2214842185525,55.7467898368407,179.985485069079));
#19656=CARTESIAN_POINT('Origin',(-8.69585033055052,-107.076100989514,171.985485069079));
#19657=CARTESIAN_POINT('',(-29.2214842185525,55.7467898368408,171.985485069079));
#19658=CARTESIAN_POINT('',(-28.5054632460221,55.8370522333853,173.235485069079));
#19659=CARTESIAN_POINT('',(-29.2214842185525,55.7467898368408,171.985485069079));
#19660=CARTESIAN_POINT('',(-7.97982935802012,-106.98583859297,173.235485069079));
#19661=CARTESIAN_POINT('',(-8.69585033055052,-107.076100989514,171.985485069079));
#19662=CARTESIAN_POINT('Origin',(-53.4413942236179,-112.716773792997,171.985485069079));
#19663=CARTESIAN_POINT('Ctrl Pts',(-32.9897426468162,36.1235247499768,171.985485069079));
#19664=CARTESIAN_POINT('Ctrl Pts',(-33.0365950120472,36.128973710728,171.985485069079));
#19665=CARTESIAN_POINT('Ctrl Pts',(-33.082044287583,36.1418391062218,171.985485069079));
#19666=CARTESIAN_POINT('Ctrl Pts',(-33.1715122949256,36.1841256819134,171.985485069079));
#19667=CARTESIAN_POINT('Ctrl Pts',(-33.2136614374764,36.2144401514148,171.98548506908));
#19668=CARTESIAN_POINT('Ctrl Pts',(-33.2950202919873,36.2974900115958,171.98548506908));
#19669=CARTESIAN_POINT('Ctrl Pts',(-33.3296649319802,36.3524534103143,171.985485069079));
#19670=CARTESIAN_POINT('Ctrl Pts',(-33.3791527024948,36.4764276694108,171.985485069079));
#19671=CARTESIAN_POINT('Ctrl Pts',(-33.3920941031955,36.54504181561,171.985485069079));
#19672=CARTESIAN_POINT('Ctrl Pts',(-33.3946169229336,36.6625737676883,171.985485069079));
#19673=CARTESIAN_POINT('Ctrl Pts',(-33.3900102035898,36.7111525376301,171.985485069076));
#19674=CARTESIAN_POINT('Ctrl Pts',(-33.3711403825,36.8029537917995,171.985485069076));
#19675=CARTESIAN_POINT('Ctrl Pts',(-33.3575537145651,36.8463261831631,171.985485069079));
#19676=CARTESIAN_POINT('Ctrl Pts',(-33.3398524907635,36.8879333098647,171.985485069079));
#19677=CARTESIAN_POINT('',(-32.3102926490249,41.4433790152692,171.985485069079));
#19678=CARTESIAN_POINT('',(-72.3928015643781,36.3474552058043,171.985485069079));
#19679=CARTESIAN_POINT('',(-31.4432161315212,42.5605980236976,171.985485069079));
#19680=CARTESIAN_POINT('',(-114.92228029935,-65.0013015450162,171.985485069079));
#19681=CARTESIAN_POINT('',(-32.5604351399496,43.4276745412012,171.985485069079));
#19682=CARTESIAN_POINT('',(30.0376699442113,-5.15487422428371,171.985485069079));
#19683=CARTESIAN_POINT('',(-31.693358622446,44.5448935496296,171.985485069079));
#19684=CARTESIAN_POINT('',(-116.039499307778,-64.1342250275126,171.985485069079));
#19685=CARTESIAN_POINT('',(-32.8105776308745,45.4119700671332,171.985485069079));
#19686=CARTESIAN_POINT('',(30.9047464617149,-4.03765521585528,171.985485069079));
#19687=CARTESIAN_POINT('',(-31.9435011133708,46.5291890755617,171.985485069079));
#19688=CARTESIAN_POINT('',(-117.156718316207,-63.267148510009,171.985485069079));
#19689=CARTESIAN_POINT('',(-33.0607201217992,47.3962655930653,171.985485069079));
#19690=CARTESIAN_POINT('',(31.7718229792185,-2.92043620742687,171.985485069079));
#19691=CARTESIAN_POINT('',(-32.1936436042956,48.5134846014937,171.985485069079));
#19692=CARTESIAN_POINT('',(-118.273937324635,-62.4000719925054,171.985485069079));
#19693=CARTESIAN_POINT('',(-33.3108626127241,49.3805611189974,171.985485069079));
#19694=CARTESIAN_POINT('',(32.6388994967221,-1.80321719899848,171.985485069079));
#19695=CARTESIAN_POINT('',(-32.4437860952204,50.4977801274258,171.985485069079));
#19696=CARTESIAN_POINT('',(-119.391156333064,-61.5329954750018,171.985485069079));
#19697=CARTESIAN_POINT('',(-33.5610051036489,51.3648566449294,171.985485069079));
#19698=CARTESIAN_POINT('',(33.5059760142258,-0.685998190570039,171.985485069079));
#19699=CARTESIAN_POINT('',(-32.6939285861452,52.4820756533578,171.985485069079));
#19700=CARTESIAN_POINT('',(-120.508375341492,-60.6659189574982,171.985485069079));
#19701=CARTESIAN_POINT('',(-33.8111475945737,53.3491521708615,171.985485069079));
#19702=CARTESIAN_POINT('',(34.3730525317294,0.43122081785836,171.985485069079));
#19703=CARTESIAN_POINT('',(-32.94407107707,54.4663711792899,171.985485069079));
#19704=CARTESIAN_POINT('',(-121.625594349921,-59.7988424399945,171.985485069079));
#19705=CARTESIAN_POINT('',(-34.0612900854985,55.3334476967935,171.985485069079));
#19706=CARTESIAN_POINT('',(35.240129049233,1.54843982628677,171.985485069079));
#19707=CARTESIAN_POINT('',(-33.1942135679949,56.4506667052219,171.985485069079));
#19708=CARTESIAN_POINT('',(-122.742813358349,-58.9317659224909,171.985485069079));
#19709=CARTESIAN_POINT('',(-34.3114325764233,57.3177432227255,171.985485069079));
#19710=CARTESIAN_POINT('',(36.1072055667355,2.66565883471801,171.985485069079));
#19711=CARTESIAN_POINT('',(-33.4443560589197,58.4349622311539,171.985485069079));
#19712=CARTESIAN_POINT('',(-123.860032366778,-58.0646894049869,171.985485069079));
#19713=CARTESIAN_POINT('',(36.9742820842401,3.78287784314388,171.985485069079));
#19714=CARTESIAN_POINT('',(-30.7570310015667,59.9437472274033,171.985459293995));
#19715=CARTESIAN_POINT('Ctrl Pts',(-31.0975708447772,60.4004632086527,171.985485069079));
#19716=CARTESIAN_POINT('Ctrl Pts',(-31.0371822006902,60.3274835122321,171.985485069079));
#19717=CARTESIAN_POINT('Ctrl Pts',(-30.9777147231722,60.2527014471572,171.985485070109));
#19718=CARTESIAN_POINT('Ctrl Pts',(-30.8639970094202,60.1012773870101,171.985485070109));
#19719=CARTESIAN_POINT('Ctrl Pts',(-30.8085788556878,60.0230926458712,171.985485069079));
#19720=CARTESIAN_POINT('Ctrl Pts',(-30.757020815632,59.9437588539596,171.985485069079));
#19721=CARTESIAN_POINT('Origin',(-39.1429618482127,54.4960773822167,171.985485069079));
#19722=CARTESIAN_POINT('Origin',(-39.1429618482127,54.4960773822167,171.985485069079));
#19723=CARTESIAN_POINT('',(-28.9015818590613,57.6692029676422,173.235485069079));
#19724=CARTESIAN_POINT('Ctrl Pts',(-30.7570310015667,59.9437472274033,171.985459293995));
#19725=CARTESIAN_POINT('Ctrl Pts',(-30.4721900266403,59.6217336312295,172.09525140435));
#19726=CARTESIAN_POINT('Ctrl Pts',(-30.2017002008111,59.3043637535052,172.235659045439));
#19727=CARTESIAN_POINT('Ctrl Pts',(-29.9430583375974,58.990922442063,172.399845773266));
#19728=CARTESIAN_POINT('Ctrl Pts',(-29.6729880538802,58.6636313266262,172.571287301006));
#19729=CARTESIAN_POINT('Ctrl Pts',(-29.4156601420299,58.3403948799334,172.768784715011));
#19730=CARTESIAN_POINT('Ctrl Pts',(-29.1687750801219,58.0200685378704,172.987248162164));
#19731=CARTESIAN_POINT('Ctrl Pts',(-29.0783477005634,57.9027415862418,173.067265466178));
#19732=CARTESIAN_POINT('Ctrl Pts',(-28.9893211789838,57.7858051107646,173.150095083597));
#19733=CARTESIAN_POINT('Ctrl Pts',(-28.9015818590613,57.6692029676421,173.235485069079));
#19734=CARTESIAN_POINT('Origin',(-39.1429618482127,54.4960773822167,173.235485069079));
#19735=CARTESIAN_POINT('Origin',(-39.1429618482127,54.4960773822167,179.985485069079));
#19736=CARTESIAN_POINT('',(-28.9015818590613,57.6692029676422,178.735485069079));
#19737=CARTESIAN_POINT('Origin',(-39.1429618482127,54.4960773822167,178.735485069079));
#19738=CARTESIAN_POINT('Ctrl Pts',(-28.9015818590613,57.6692029676422,178.735485069079));
#19739=CARTESIAN_POINT('Ctrl Pts',(-29.1411279737203,57.9875504356935,178.968617024867));
#19740=CARTESIAN_POINT('Ctrl Pts',(-29.390270556352,58.3083899273538,179.182659656602));
#19741=CARTESIAN_POINT('Ctrl Pts',(-29.6513150897315,58.632864293538,179.372505039673));
#19742=CARTESIAN_POINT('Ctrl Pts',(-29.7469287040763,58.7517105551756,179.442040314007));
#19743=CARTESIAN_POINT('Ctrl Pts',(-29.8441388328647,58.8710444806848,179.508329929376));
#19744=CARTESIAN_POINT('Ctrl Pts',(-29.9430583375964,58.9909224420661,179.571124364888));
#19745=CARTESIAN_POINT('Ctrl Pts',(-30.2017002008109,59.3043637535053,179.735311092719));
#19746=CARTESIAN_POINT('Ctrl Pts',(-30.4721900266405,59.6217336312296,179.875718733809));
#19747=CARTESIAN_POINT('Ctrl Pts',(-30.7570310015667,59.9437472274033,179.985510844164));
#19748=CARTESIAN_POINT('Origin',(-34.5615750673481,59.3020387486575,165.645237852233));
#19749=CARTESIAN_POINT('',(-33.4443560589197,58.4349622311539,165.645237852233));
#19750=CARTESIAN_POINT('Origin',(-33.4443560589197,58.4349622311539,165.645237852233));
#19751=CARTESIAN_POINT('',(-34.3114325764233,57.3177432227255,165.645237852233));
#19752=CARTESIAN_POINT('Origin',(-34.3114325764233,57.3177432227255,165.645237852233));
#19753=CARTESIAN_POINT('',(-33.1942135679949,56.4506667052219,165.645237852233));
#19754=CARTESIAN_POINT('Origin',(-33.1942135679949,56.4506667052219,165.645237852233));
#19755=CARTESIAN_POINT('',(-34.0612900854985,55.3334476967935,165.645237852233));
#19756=CARTESIAN_POINT('Origin',(-34.0612900854985,55.3334476967935,165.645237852233));
#19757=CARTESIAN_POINT('',(-32.94407107707,54.4663711792899,165.645237852233));
#19758=CARTESIAN_POINT('Origin',(-32.94407107707,54.4663711792899,165.645237852233));
#19759=CARTESIAN_POINT('',(-33.8111475945737,53.3491521708615,165.645237852233));
#19760=CARTESIAN_POINT('Origin',(-33.8111475945737,53.3491521708615,165.645237852233));
#19761=CARTESIAN_POINT('',(-32.6939285861452,52.4820756533578,165.645237852233));
#19762=CARTESIAN_POINT('Origin',(-32.6939285861452,52.4820756533578,165.645237852233));
#19763=CARTESIAN_POINT('',(-33.5610051036489,51.3648566449294,165.645237852233));
#19764=CARTESIAN_POINT('Origin',(-33.5610051036489,51.3648566449294,165.645237852233));
#19765=CARTESIAN_POINT('',(-32.4437860952204,50.4977801274258,165.645237852233));
#19766=CARTESIAN_POINT('Origin',(-32.4437860952204,50.4977801274258,165.645237852233));
#19767=CARTESIAN_POINT('',(-33.3108626127241,49.3805611189974,165.645237852233));
#19768=CARTESIAN_POINT('Origin',(-33.3108626127241,49.3805611189974,165.645237852233));
#19769=CARTESIAN_POINT('',(-32.1936436042956,48.5134846014937,165.645237852233));
#19770=CARTESIAN_POINT('Origin',(-32.1936436042956,48.5134846014937,165.645237852233));
#19771=CARTESIAN_POINT('',(-33.0607201217992,47.3962655930653,165.645237852233));
#19772=CARTESIAN_POINT('Origin',(-33.0607201217992,47.3962655930653,165.645237852233));
#19773=CARTESIAN_POINT('',(-31.9435011133708,46.5291890755617,165.645237852233));
#19774=CARTESIAN_POINT('Origin',(-31.9435011133708,46.5291890755617,165.645237852233));
#19775=CARTESIAN_POINT('',(-32.8105776308745,45.4119700671332,165.645237852233));
#19776=CARTESIAN_POINT('Origin',(-32.8105776308745,45.4119700671332,165.645237852233));
#19777=CARTESIAN_POINT('',(-31.693358622446,44.5448935496296,165.645237852233));
#19778=CARTESIAN_POINT('Origin',(-31.693358622446,44.5448935496296,165.645237852233));
#19779=CARTESIAN_POINT('',(-32.5604351399496,43.4276745412012,165.645237852233));
#19780=CARTESIAN_POINT('Origin',(-32.5604351399496,43.4276745412012,165.645237852233));
#19781=CARTESIAN_POINT('',(-31.4432161315212,42.5605980236976,165.645237852233));
#19782=CARTESIAN_POINT('Origin',(-31.4432161315212,42.5605980236976,165.645237852233));
#19783=CARTESIAN_POINT('',(-32.3102926490249,41.4433790152692,165.645237852233));
#19784=CARTESIAN_POINT('Origin',(-37.2830935213589,40.8111577534073,165.645237852233));
#19785=CARTESIAN_POINT('Origin',(-7.55021677450188,-106.931681155043,172.985485069079));
#19786=CARTESIAN_POINT('',(-28.0900682566218,55.8894173856563,173.485279674622));
#19787=CARTESIAN_POINT('Origin',(-28.0758506625039,55.8912096713119,172.985485069079));
#19788=CARTESIAN_POINT('Origin',(-26.8530188945057,47.5592063900784,158.714565891));
#19789=CARTESIAN_POINT('Origin',(-39.1429618482127,54.4960773822167,172.985485069079));
#19790=CARTESIAN_POINT('Ctrl Pts',(-28.9015818590613,57.6692029676421,173.235485069079));
#19791=CARTESIAN_POINT('Ctrl Pts',(-28.8783957075631,57.6244523537673,173.250906112447));
#19792=CARTESIAN_POINT('Ctrl Pts',(-28.8552578884252,57.5793410334276,173.264929290539));
#19793=CARTESIAN_POINT('Ctrl Pts',(-28.832206350973,57.5339462931836,173.277868929688));
#19794=CARTESIAN_POINT('Ctrl Pts',(-28.8065664597265,57.4834543810741,173.292261502906));
#19795=CARTESIAN_POINT('Ctrl Pts',(-28.7810331273392,57.4326117098059,173.305313364622));
#19796=CARTESIAN_POINT('Ctrl Pts',(-28.7556446263524,57.3814869308062,173.317399481028));
#19797=CARTESIAN_POINT('Ctrl Pts',(-28.7329260654482,57.3357386053725,173.328214580818));
#19798=CARTESIAN_POINT('Ctrl Pts',(-28.7103230594705,57.2897634704848,173.33825497767));
#19799=CARTESIAN_POINT('Ctrl Pts',(-28.6878575715527,57.2435917682567,173.347760399718));
#19800=CARTESIAN_POINT('Ctrl Pts',(-28.6871251437978,57.2420864621477,173.348070298838));
#19801=CARTESIAN_POINT('Ctrl Pts',(-28.6863928067171,57.2405808318857,173.34837957377));
#19802=CARTESIAN_POINT('Ctrl Pts',(-28.6856605607426,57.2390748787108,173.348688226559));
#19803=CARTESIAN_POINT('Ctrl Pts',(-28.6546983128659,57.1753972387935,173.361739283828));
#19804=CARTESIAN_POINT('Ctrl Pts',(-28.6239686550817,57.111288866525,173.373652144523));
#19805=CARTESIAN_POINT('Ctrl Pts',(-28.5935146468786,57.0468622475461,173.384569672603));
#19806=CARTESIAN_POINT('Ctrl Pts',(-28.5594104597168,56.9747135353897,173.396795761809));
#19807=CARTESIAN_POINT('Ctrl Pts',(-28.5256504453393,56.9021633205751,173.407773929404));
#19808=CARTESIAN_POINT('Ctrl Pts',(-28.4923003004926,56.8293357844001,173.417654178831));
#19809=CARTESIAN_POINT('Ctrl Pts',(-28.4872778889987,56.818368220198,173.419142108749));
#19810=CARTESIAN_POINT('Ctrl Pts',(-28.4822648091068,56.8073943548846,173.420605050385));
#19811=CARTESIAN_POINT('Ctrl Pts',(-28.4772613313079,56.7964146162697,173.422043425076));
#19812=CARTESIAN_POINT('Ctrl Pts',(-28.4770521713326,56.7959556311497,173.422103553336));
#19813=CARTESIAN_POINT('Ctrl Pts',(-28.4768430287364,56.7954966370769,173.422163638491));
#19814=CARTESIAN_POINT('Ctrl Pts',(-28.4766339035806,56.7950376341736,173.422223680559));
#19815=CARTESIAN_POINT('Ctrl Pts',(-28.4066282600523,56.641384222626,173.442323049322));
#19816=CARTESIAN_POINT('Ctrl Pts',(-28.3384533787665,56.4865756844121,173.457833018597));
#19817=CARTESIAN_POINT('Ctrl Pts',(-28.2720423773652,56.3306091186088,173.468472689585));
#19818=CARTESIAN_POINT('Ctrl Pts',(-28.2098532731482,56.184557699259,173.478435972685));
#19819=CARTESIAN_POINT('Ctrl Pts',(-28.1492110828377,56.0374907574936,173.484128243792));
#19820=CARTESIAN_POINT('Ctrl Pts',(-28.0900682566218,55.8894173856563,173.485279674622));
#19821=CARTESIAN_POINT('Origin',(-7.55021677450188,-106.931681155043,178.985485069079));
#19822=CARTESIAN_POINT('',(-28.0900682566218,55.8894173856563,178.485690463537));
#19823=CARTESIAN_POINT('Origin',(-26.8543432602028,47.5681742429628,193.240450635157));
#19824=CARTESIAN_POINT('Origin',(-28.0758506625039,55.8912096713119,178.985485069079));
#19825=CARTESIAN_POINT('Origin',(-39.1429618482127,54.4960773822167,178.985485069079));
#19826=CARTESIAN_POINT('Ctrl Pts',(-28.0900682566218,55.8894173856563,178.485690463537));
#19827=CARTESIAN_POINT('Ctrl Pts',(-28.1532261741964,56.0475431705021,178.486920062765));
#19828=CARTESIAN_POINT('Ctrl Pts',(-28.2180938553462,56.2045210764306,178.493327449093));
#19829=CARTESIAN_POINT('Ctrl Pts',(-28.2847294808783,56.3603405304585,178.504585631502));
#19830=CARTESIAN_POINT('Ctrl Pts',(-28.34712892925,56.5062541899956,178.515128105837));
#19831=CARTESIAN_POINT('Ctrl Pts',(-28.4110786768076,56.6511523167797,178.529924851071));
#19832=CARTESIAN_POINT('Ctrl Pts',(-28.4766339035804,56.7950376341737,178.5487464576));
#19833=CARTESIAN_POINT('Ctrl Pts',(-28.4768430287362,56.7954966370769,178.548806499668));
#19834=CARTESIAN_POINT('Ctrl Pts',(-28.4770521713324,56.7959556311498,178.548866584823));
#19835=CARTESIAN_POINT('Ctrl Pts',(-28.4772613313078,56.7964146162698,178.548926713083));
#19836=CARTESIAN_POINT('Ctrl Pts',(-28.5112094816522,56.8709111629163,178.558685956994));
#19837=CARTESIAN_POINT('Ctrl Pts',(-28.54559760442,56.9451372173971,178.569572016831));
#19838=CARTESIAN_POINT('Ctrl Pts',(-28.5803527484962,57.0189613364396,178.581737771227));
#19839=CARTESIAN_POINT('Ctrl Pts',(-28.610726409608,57.0834786570626,178.592369823289));
#19840=CARTESIAN_POINT('Ctrl Pts',(-28.6413817046753,57.1476909918109,178.603979625781));
#19841=CARTESIAN_POINT('Ctrl Pts',(-28.6722760253921,57.2114911539207,178.616704729058));
#19842=CARTESIAN_POINT('Ctrl Pts',(-28.6767326149162,57.2206945002802,178.618540359706));
#19843=CARTESIAN_POINT('Ctrl Pts',(-28.6811941725409,57.2298892065096,178.620399261204));
#19844=CARTESIAN_POINT('Ctrl Pts',(-28.6856605607423,57.2390748787112,178.6222819116));
#19845=CARTESIAN_POINT('Ctrl Pts',(-28.6863928067167,57.2405808318861,178.622590564388));
#19846=CARTESIAN_POINT('Ctrl Pts',(-28.6871251437975,57.2420864621481,178.62289983932));
#19847=CARTESIAN_POINT('Ctrl Pts',(-28.6878575715524,57.2435917682571,178.62320973844));
#19848=CARTESIAN_POINT('Ctrl Pts',(-28.7136979020017,57.2966995417155,178.634143097541));
#19849=CARTESIAN_POINT('Ctrl Pts',(-28.7397203004661,57.3495477961519,178.645783407186));
#19850=CARTESIAN_POINT('Ctrl Pts',(-28.7658909284461,57.4020887705021,178.658498134593));
#19851=CARTESIAN_POINT('Ctrl Pts',(-28.7890925824529,57.4486691394938,178.669770416874));
#19852=CARTESIAN_POINT('Ctrl Pts',(-28.8124109552486,57.495008155114,178.681886920562));
#19853=CARTESIAN_POINT('Ctrl Pts',(-28.8358161917034,57.5410513416207,178.695136076362));
#19854=CARTESIAN_POINT('Ctrl Pts',(-28.8576730368229,57.584048505876,178.707508724118));
#19855=CARTESIAN_POINT('Ctrl Pts',(-28.8796057823956,57.6267878682054,178.720868843039));
#19856=CARTESIAN_POINT('Ctrl Pts',(-28.9015818590613,57.6692029676421,178.735485069079));
#19857=CARTESIAN_POINT('Ctrl Pts',(-27.6574947146374,56.1206152968612,177.985485069079));
#19858=CARTESIAN_POINT('Ctrl Pts',(-27.6574947146374,56.1206152968612,178.485485069079));
#19859=CARTESIAN_POINT('Ctrl Pts',(-28.0689593736356,55.8365434144167,178.485485069079));
#19860=CARTESIAN_POINT('Ctrl Pts',(-27.6694079641717,56.1378710742194,177.985485068867));
#19861=CARTESIAN_POINT('Ctrl Pts',(-27.6681144406602,56.1359974667813,178.481269766953));
#19862=CARTESIAN_POINT('Ctrl Pts',(-28.0759896722413,55.8541773044658,178.485485069079));
#19863=CARTESIAN_POINT('Ctrl Pts',(-27.6813344276784,56.1551166027306,177.985621535458));
#19864=CARTESIAN_POINT('Ctrl Pts',(-27.6788158552697,56.1514749213828,178.477207837903));
#19865=CARTESIAN_POINT('Ctrl Pts',(-28.083025968225,55.871801963558,178.485553302133));
#19866=CARTESIAN_POINT('Ctrl Pts',(-27.6932740952942,56.17235187585,177.985895857994));
#19867=CARTESIAN_POINT('Ctrl Pts',(-27.6895961064823,56.1670425872045,178.473302706478));
#19868=CARTESIAN_POINT('Ctrl Pts',(-28.0900682566218,55.8894173856562,178.485690463537));
#19869=CARTESIAN_POINT('Origin',(-28.1042858507397,55.8876251000007,177.985895857994));
#19870=CARTESIAN_POINT('Ctrl Pts',(-28.9015818590613,57.6692029676421,178.735485069079));
#19871=CARTESIAN_POINT('Ctrl Pts',(-28.8684594052104,57.7807218601806,178.623519943881));
#19872=CARTESIAN_POINT('Ctrl Pts',(-28.9197092925293,57.8469757052856,178.485485069079));
#19873=CARTESIAN_POINT('Ctrl Pts',(-28.8312423460306,57.5334435982818,178.688702479453));
#19874=CARTESIAN_POINT('Ctrl Pts',(-28.7721100878092,57.6556162573135,178.558964673111));
#19875=CARTESIAN_POINT('Ctrl Pts',(-28.8243214284443,57.72366201422,178.392078873294));
#19876=CARTESIAN_POINT('Ctrl Pts',(-28.7591862218731,57.3901866577354,178.653390254656));
#19877=CARTESIAN_POINT('Ctrl Pts',(-28.672354550029,57.5244839151744,178.515152190406));
#19878=CARTESIAN_POINT('Ctrl Pts',(-28.7239047060481,57.5923063305154,178.321295444065));
#19879=CARTESIAN_POINT('Ctrl Pts',(-28.6165295181076,57.0969960951184,178.593029960819));
#19880=CARTESIAN_POINT('Ctrl Pts',(-28.471590439667,57.2570348653644,178.447866227612));
#19881=CARTESIAN_POINT('Ctrl Pts',(-28.5198863309438,57.3216783903814,178.200574848726));
#19882=CARTESIAN_POINT('Ctrl Pts',(-28.5454048906478,56.9459811395567,178.568491345164));
#19883=CARTESIAN_POINT('Ctrl Pts',(-28.3690672047113,57.1185646996549,178.425946256232));
#19884=CARTESIAN_POINT('Ctrl Pts',(-28.4153684876184,57.1811899787714,178.151497622782));
#19885=CARTESIAN_POINT('Ctrl Pts',(-28.3390919900902,56.4931505677619,178.509256722049));
#19886=CARTESIAN_POINT('Ctrl Pts',(-28.0597531656501,56.6952271283425,178.389517436387));
#19887=CARTESIAN_POINT('Ctrl Pts',(-28.1035068265426,56.7559702344856,178.033028371953));
#19888=CARTESIAN_POINT('Ctrl Pts',(-28.2104907674039,56.1909140904525,178.48803492694));
#19889=CARTESIAN_POINT('Ctrl Pts',(-27.8614033472109,56.415147805598,178.410967591661));
#19890=CARTESIAN_POINT('Ctrl Pts',(-27.897368693661,56.4669686322174,177.990585092576));
#19891=CARTESIAN_POINT('Ctrl Pts',(-28.0900682566218,55.8894173856563,178.485690463537));
#19892=CARTESIAN_POINT('Ctrl Pts',(-27.6895961064823,56.1670425872046,178.473302706478));
#19893=CARTESIAN_POINT('Ctrl Pts',(-27.6932740952942,56.1723518758501,177.985895857994));
#19894=CARTESIAN_POINT('Origin',(-29.3151965518073,57.5410511594434,178.485485069079));
#19895=CARTESIAN_POINT('Ctrl Pts',(-28.9197092925293,57.8469757052856,178.485485069079));
#19896=CARTESIAN_POINT('Ctrl Pts',(-28.8684594052104,57.7807218601806,178.623519943881));
#19897=CARTESIAN_POINT('Ctrl Pts',(-28.9015818590613,57.6692029676421,178.735485069079));
#19898=CARTESIAN_POINT('Ctrl Pts',(-29.2441517252768,58.2664021627722,178.803187555911));
#19899=CARTESIAN_POINT('Ctrl Pts',(-29.1960592199985,58.2060626206576,178.939525960898));
#19900=CARTESIAN_POINT('Ctrl Pts',(-29.2280229684941,58.1030305019131,179.053185293937));
#19901=CARTESIAN_POINT('Ctrl Pts',(-29.5857084336898,58.6906563012156,179.086383412666));
#19902=CARTESIAN_POINT('Ctrl Pts',(-29.5424509131589,58.6380170915417,179.222334391769));
#19903=CARTESIAN_POINT('Ctrl Pts',(-29.5732144254148,58.5426646457117,179.336383412017));
#19904=CARTESIAN_POINT('Ctrl Pts',(-30.3136646322233,59.5550714589887,179.555994501918));
#19905=CARTESIAN_POINT('Ctrl Pts',(-30.2815269581094,59.5181763377526,179.690677583542));
#19906=CARTESIAN_POINT('Ctrl Pts',(-30.3129364447101,59.439080359551,179.805994502568));
#19907=CARTESIAN_POINT('Ctrl Pts',(-30.7003778315039,59.9956453799363,179.742653148955));
#19908=CARTESIAN_POINT('Ctrl Pts',(-30.6749317799783,59.967435021151,179.877207841684));
#19909=CARTESIAN_POINT('Ctrl Pts',(-30.707799046115,59.8962927399543,179.992649949041));
#19910=CARTESIAN_POINT('Ctrl Pts',(-31.1165943278663,60.4472861348584,179.860245913625));
#19911=CARTESIAN_POINT('Ctrl Pts',(-31.0989366204049,60.4281255768369,179.994612574165));
#19912=CARTESIAN_POINT('Ctrl Pts',(-31.1350022734637,60.3643955167689,180.110245913625));
#19913=CARTESIAN_POINT('Ctrl Pts',(-28.0689593736356,55.8365434144167,173.485485069079));
#19914=CARTESIAN_POINT('Ctrl Pts',(-27.6574947146374,56.1206152968612,173.485485069079));
#19915=CARTESIAN_POINT('Ctrl Pts',(-27.6574947146374,56.1206152968612,173.985485069079));
#19916=CARTESIAN_POINT('Ctrl Pts',(-28.0759896722412,55.8541773044657,173.485485069079));
#19917=CARTESIAN_POINT('Ctrl Pts',(-27.6681144406602,56.1359974667812,173.489700371206));
#19918=CARTESIAN_POINT('Ctrl Pts',(-27.6694079641718,56.1378710742195,173.985485069291));
#19919=CARTESIAN_POINT('Ctrl Pts',(-28.0830259682254,55.8718019635579,173.485416836026));
#19920=CARTESIAN_POINT('Ctrl Pts',(-27.6788158552703,56.1514749213822,173.493762300257));
#19921=CARTESIAN_POINT('Ctrl Pts',(-27.6813344276784,56.1551166027305,173.9853486027));
#19922=CARTESIAN_POINT('Ctrl Pts',(-28.0900682566218,55.8894173856563,173.485279674622));
#19923=CARTESIAN_POINT('Ctrl Pts',(-27.6895961064823,56.1670425872046,173.497667431681));
#19924=CARTESIAN_POINT('Ctrl Pts',(-27.6932740952942,56.1723518758501,173.985074280165));
#19925=CARTESIAN_POINT('Origin',(-28.1042858507397,55.8876251000007,173.985074280165));
#19926=CARTESIAN_POINT('Ctrl Pts',(-28.9197092925293,57.8469757052856,173.485485069079));
#19927=CARTESIAN_POINT('Ctrl Pts',(-28.8684594052104,57.7807218601806,173.347450194278));
#19928=CARTESIAN_POINT('Ctrl Pts',(-28.9015818590613,57.6692029676421,173.235485069079));
#19929=CARTESIAN_POINT('Ctrl Pts',(-28.8243214284456,57.7236620142217,173.578891264868));
#19930=CARTESIAN_POINT('Ctrl Pts',(-28.7721100878089,57.6556162573148,173.412005465051));
#19931=CARTESIAN_POINT('Ctrl Pts',(-28.8312423460299,57.5334435982831,173.282267658708));
#19932=CARTESIAN_POINT('Ctrl Pts',(-28.7239047060486,57.592306330516,173.649674694096));
#19933=CARTESIAN_POINT('Ctrl Pts',(-28.6723545500293,57.5244839151751,173.455817947753));
#19934=CARTESIAN_POINT('Ctrl Pts',(-28.7591862218723,57.3901866577358,173.317579883503));
#19935=CARTESIAN_POINT('Ctrl Pts',(-28.5198863309434,57.3216783903809,173.77039528943));
#19936=CARTESIAN_POINT('Ctrl Pts',(-28.4715904396667,57.2570348653639,173.523103910547));
#19937=CARTESIAN_POINT('Ctrl Pts',(-28.6165295181085,57.096996095118,173.377940177339));
#19938=CARTESIAN_POINT('Ctrl Pts',(-28.4153684876182,57.1811899787712,173.819472515376));
#19939=CARTESIAN_POINT('Ctrl Pts',(-28.3690672047116,57.1185646996537,173.545023881929));
#19940=CARTESIAN_POINT('Ctrl Pts',(-28.5454048906478,56.9459811395561,173.402478792994));
#19941=CARTESIAN_POINT('Ctrl Pts',(-28.103506826543,56.7559702344862,173.937941766205));
#19942=CARTESIAN_POINT('Ctrl Pts',(-28.0597531656494,56.695227128345,173.581452701767));
#19943=CARTESIAN_POINT('Ctrl Pts',(-28.3390919900903,56.4931505677632,173.46171341611));
#19944=CARTESIAN_POINT('Ctrl Pts',(-27.8973686936607,56.4669686322171,173.980385045582));
#19945=CARTESIAN_POINT('Ctrl Pts',(-27.8614033472118,56.4151478055982,173.560002546493));
#19946=CARTESIAN_POINT('Ctrl Pts',(-28.2104907674024,56.1909140904522,173.482935211219));
#19947=CARTESIAN_POINT('Ctrl Pts',(-27.6932740952942,56.1723518758501,173.985074280165));
#19948=CARTESIAN_POINT('Ctrl Pts',(-27.6895961064823,56.1670425872046,173.497667431681));
#19949=CARTESIAN_POINT('Ctrl Pts',(-28.0900682566218,55.8894173856563,173.485279674622));
#19950=CARTESIAN_POINT('Origin',(-29.3151965518073,57.5410511594434,173.485485069079));
#19951=CARTESIAN_POINT('Ctrl Pts',(-28.9015818590613,57.6692029676421,173.235485069079));
#19952=CARTESIAN_POINT('Ctrl Pts',(-28.8684594052104,57.7807218601806,173.347450194278));
#19953=CARTESIAN_POINT('Ctrl Pts',(-28.9197092925293,57.8469757052856,173.485485069079));
#19954=CARTESIAN_POINT('Ctrl Pts',(-29.2280229684935,58.1030305019142,172.917784844223));
#19955=CARTESIAN_POINT('Ctrl Pts',(-29.1960592200032,58.2060626206536,173.03144417726));
#19956=CARTESIAN_POINT('Ctrl Pts',(-29.244151725278,58.2664021627738,173.167782582254));
#19957=CARTESIAN_POINT('Ctrl Pts',(-29.5732144254162,58.5426646457073,172.634586726136));
#19958=CARTESIAN_POINT('Ctrl Pts',(-29.5424509131556,58.6380170915374,172.748635746381));
#19959=CARTESIAN_POINT('Ctrl Pts',(-29.5857084336879,58.6906563012133,172.884586725484));
#19960=CARTESIAN_POINT('Ctrl Pts',(-30.3129364447087,59.4390803595552,172.164975635597));
#19961=CARTESIAN_POINT('Ctrl Pts',(-30.2815269581124,59.5181763377567,172.280292554625));
#19962=CARTESIAN_POINT('Ctrl Pts',(-30.3136646322252,59.555071458991,172.414975636249));
#19963=CARTESIAN_POINT('Ctrl Pts',(-30.7077990461131,59.8962927399557,171.978320189122));
#19964=CARTESIAN_POINT('Ctrl Pts',(-30.6749317799805,59.9674350211545,172.093762296512));
#19965=CARTESIAN_POINT('Ctrl Pts',(-30.7003778315034,59.9956453799358,172.228316989206));
#19966=CARTESIAN_POINT('Ctrl Pts',(-31.1350022734636,60.3643955167688,171.860724224534));
#19967=CARTESIAN_POINT('Ctrl Pts',(-31.0989366204048,60.4281255768368,171.976357563994));
#19968=CARTESIAN_POINT('Ctrl Pts',(-31.1165943278662,60.4472861348583,172.110724224534));
#19969=CARTESIAN_POINT('Origin',(-51.4899841053611,-42.5281564925371,175.985485069079));
#19970=CARTESIAN_POINT('Origin',(-51.4899841053611,-42.5281564925371,175.985485069079));
#19971=CARTESIAN_POINT('',(-59.8287670060529,-101.979172801565,172.515418850865));
#19972=CARTESIAN_POINT('Origin',(-57.8503443722502,-102.190085871961,175.985485069079));
#19973=CARTESIAN_POINT('Ctrl Pts',(-59.8287670060529,-101.979172801565,
172.515418850865));
#19974=CARTESIAN_POINT('Ctrl Pts',(-60.2848547374583,-101.898008987142,
172.780385782992));
#19975=CARTESIAN_POINT('Ctrl Pts',(-60.6562094364539,-101.828107748012,
173.157058062683));
#19976=CARTESIAN_POINT('Ctrl Pts',(-60.8101044574071,-101.799139614069,
173.313156769748));
#19977=CARTESIAN_POINT('Ctrl Pts',(-60.9459236613779,-101.771602184887,
173.485485069079));
#19978=CARTESIAN_POINT('Origin',(-57.8503443722502,-102.190085871961,175.985485069079));
#19979=CARTESIAN_POINT('Ctrl Pts',(-60.6425873069478,-101.892414120442,
173.485485069077));
#19980=CARTESIAN_POINT('Ctrl Pts',(-60.507560609551,-101.906808868484,173.25618146547));
#19981=CARTESIAN_POINT('Ctrl Pts',(-60.3677502586115,-101.921713585952,
173.078920934662));
#19982=CARTESIAN_POINT('Ctrl Pts',(-60.1377190475615,-101.946236449864,
172.805174418299));
#19983=CARTESIAN_POINT('Ctrl Pts',(-59.9888386836434,-101.962108091312,
172.654046519857));
#19984=CARTESIAN_POINT('Ctrl Pts',(-59.8287670060529,-101.979172801565,
172.515418850865));
#19985=CARTESIAN_POINT('Origin',(-51.4899841053611,-42.5281564925371,175.985485069079));
#19986=CARTESIAN_POINT('Origin',(-62.88786637536,-111.709716750739,178.985485069079));
#19987=CARTESIAN_POINT('Origin',(-52.5853897920404,-15.069651635714,178.985485069079));
#19988=CARTESIAN_POINT('Origin',(-67.998054881725,-13.4265585667677,178.985485069079));
#19989=CARTESIAN_POINT('Origin',(-52.5342226896633,-12.3683081541722,178.985485069079));
#19990=CARTESIAN_POINT('Origin',(-52.4446243855275,-13.6775759072102,178.985485069079));
#19991=CARTESIAN_POINT('Origin',(-53.9352248596064,8.10403203946808,178.985485069079));
#19992=CARTESIAN_POINT('Origin',(-39.4690592605811,9.0940082318961,178.985485069079));
#19993=CARTESIAN_POINT('Origin',(-52.9717383111942,-18.6937070505612,180.485485069079));
#19994=CARTESIAN_POINT('Origin',(-52.5853897920404,-15.069651635714,180.485485069079));
#19995=CARTESIAN_POINT('Origin',(-67.998054881725,-13.4265585667677,180.485485069079));
#19996=CARTESIAN_POINT('Origin',(-52.5342226896633,-12.3683081541722,180.485485069079));
#19997=CARTESIAN_POINT('Origin',(-51.890637311636,-21.772789521366,180.485485069079));
#19998=CARTESIAN_POINT('Origin',(-53.9352248596064,8.10403203946808,180.485485069079));
#19999=CARTESIAN_POINT('Origin',(-39.4690592605811,9.0940082318961,180.485485069079));
#20000=CARTESIAN_POINT('Origin',(-41.2825923197859,23.4801507949034,180.485485069079));
#20001=CARTESIAN_POINT('Origin',(-40.5289338663118,23.5751578139663,180.485485069079));
#20002=CARTESIAN_POINT('Origin',(-24.4968854027218,25.596175593274,180.485485069079));
#20003=CARTESIAN_POINT('Ctrl Pts',(-20.9569943874949,26.5463753651884,176.985485069079));
#20004=CARTESIAN_POINT('Ctrl Pts',(-20.3076118873532,26.6282372421243,176.985485069079));
#20005=CARTESIAN_POINT('Ctrl Pts',(-20.3993997459139,25.9801832417458,176.985485069079));
#20006=CARTESIAN_POINT('Ctrl Pts',(-20.9569943910055,26.5463753647458,177.220977963401));
#20007=CARTESIAN_POINT('Ctrl Pts',(-20.3076118917219,26.6282372415765,177.266627063424));
#20008=CARTESIAN_POINT('Ctrl Pts',(-20.3993997460441,25.9801832408266,177.254619805483));
#20009=CARTESIAN_POINT('Ctrl Pts',(-20.9811883709224,26.543325444851,177.45231830065));
#20010=CARTESIAN_POINT('Ctrl Pts',(-20.3376037120335,26.6244564394995,177.542172659695));
#20011=CARTESIAN_POINT('Ctrl Pts',(-20.4269246477449,25.9775831262692,177.519008762253));
#20012=CARTESIAN_POINT('Ctrl Pts',(-21.0757990735786,26.5313987149253,177.906973211595));
#20013=CARTESIAN_POINT('Ctrl Pts',(-20.4549506534422,26.6096635541441,178.083132559644));
#20014=CARTESIAN_POINT('Ctrl Pts',(-20.5345596128582,25.9674199466701,178.038614374861));
#20015=CARTESIAN_POINT('Ctrl Pts',(-21.1475020349058,26.522359760234,178.13275546379));
#20016=CARTESIAN_POINT('Ctrl Pts',(-20.5433816467323,26.5985158452194,178.350325889774));
#20017=CARTESIAN_POINT('Ctrl Pts',(-20.6161329571035,25.9597188096215,178.296651234969));
#20018=CARTESIAN_POINT('Ctrl Pts',(-21.3330091361947,26.4989745296601,178.56011431014));
#20019=CARTESIAN_POINT('Ctrl Pts',(-20.7717245231082,26.5697306894192,178.853810146054));
#20020=CARTESIAN_POINT('Ctrl Pts',(-20.8271720934702,25.9398095413006,178.785061344071));
#20021=CARTESIAN_POINT('Ctrl Pts',(-21.4462792894842,26.4846955687286,178.762334660914));
#20022=CARTESIAN_POINT('Ctrl Pts',(-20.9100975499512,26.5522872324514,179.090130315615));
#20023=CARTESIAN_POINT('Ctrl Pts',(-20.9560304163274,25.9276586659783,179.01617031644));
#20024=CARTESIAN_POINT('Ctrl Pts',(-21.7133004202462,26.4510345893506,179.144165737296));
#20025=CARTESIAN_POINT('Ctrl Pts',(-21.2350328903241,26.5113255236894,179.532928715243));
#20026=CARTESIAN_POINT('Ctrl Pts',(-21.2597905826465,25.8990431476073,179.452548690349));
#20027=CARTESIAN_POINT('Ctrl Pts',(-21.8670860845458,26.4316481982441,179.322751431888));
#20028=CARTESIAN_POINT('Ctrl Pts',(-21.4205619530434,26.4879375246306,179.737877540268));
#20029=CARTESIAN_POINT('Ctrl Pts',(-21.4347317392525,25.8825753022298,179.656646627006));
#20030=CARTESIAN_POINT('Ctrl Pts',(-22.2017889982529,26.3894551783737,179.642261663974));
#20031=CARTESIAN_POINT('Ctrl Pts',(-21.8221797156734,26.4373091448254,180.100434649856));
#20032=CARTESIAN_POINT('Ctrl Pts',(-21.8154653408504,25.8467781859745,180.0218011771));
#20033=CARTESIAN_POINT('Ctrl Pts',(-22.3846701288836,26.3664009805684,179.785713045127));
#20034=CARTESIAN_POINT('Ctrl Pts',(-22.0396265413609,26.4098975572291,180.261103787136));
#20035=CARTESIAN_POINT('Ctrl Pts',(-22.0234918530467,25.827238523971,180.185745614722));
#20036=CARTESIAN_POINT('Ctrl Pts',(-22.7786882937544,26.3167306144649,180.037038838909));
#20037=CARTESIAN_POINT('Ctrl Pts',(-22.5053049632146,26.3511936197905,180.538045339618));
#20038=CARTESIAN_POINT('Ctrl Pts',(-22.4716684057107,25.785200536956,180.472975090153));
#20039=CARTESIAN_POINT('Ctrl Pts',(-22.9847021376152,26.2907602812183,180.141806276838));
#20040=CARTESIAN_POINT('Ctrl Pts',(-22.7466972207022,26.3207634445538,180.651430961495));
#20041=CARTESIAN_POINT('Ctrl Pts',(-22.7059910527553,25.7632488339365,180.592709306442));
#20042=CARTESIAN_POINT('Ctrl Pts',(-23.6283960230643,26.2096155173486,180.39658255964));
#20043=CARTESIAN_POINT('Ctrl Pts',(-23.4895764797135,26.2271152626769,180.917343237008));
#20044=CARTESIAN_POINT('Ctrl Pts',(-23.4381054919345,25.6947662436456,180.883882201301));
#20045=CARTESIAN_POINT('Ctrl Pts',(-24.0961299454542,26.1506524612375,180.485485065088));
#20046=CARTESIAN_POINT('Ctrl Pts',(-24.0256564111632,26.1595364330049,181.003088599679));
#20047=CARTESIAN_POINT('Ctrl Pts',(-23.9700486532876,25.6451485909903,180.985485069078));
#20048=CARTESIAN_POINT('Ctrl Pts',(-24.559421025453,26.0922494747571,180.485485069079));
#20049=CARTESIAN_POINT('Ctrl Pts',(-24.5594210254521,26.0922494747572,180.98548506908));
#20050=CARTESIAN_POINT('Ctrl Pts',(-24.4968854027209,25.5961755932739,180.985485069079));
#20051=CARTESIAN_POINT('Origin',(-20.8944587647637,26.0503014837053,176.985485069079));
#20052=CARTESIAN_POINT('Origin',(-20.8944587647637,26.0503014837054,176.985485069079));
#20053=CARTESIAN_POINT('Origin',(-20.8944587647637,26.0503014837053,174.985485069079));
#20054=CARTESIAN_POINT('Ctrl Pts',(-24.5594210254598,26.0922494747562,171.485485069079));
#20055=CARTESIAN_POINT('Ctrl Pts',(-24.5594210254598,26.0922494747562,170.985485069079));
#20056=CARTESIAN_POINT('Ctrl Pts',(-24.4968854027286,25.5961755932732,170.985485069079));
#20057=CARTESIAN_POINT('Ctrl Pts',(-24.3258682437323,26.1216913970003,171.485485071833));
#20058=CARTESIAN_POINT('Ctrl Pts',(-24.2925991176692,26.1258853398606,170.976685296256));
#20059=CARTESIAN_POINT('Ctrl Pts',(-24.2312974837435,25.6208637654299,170.985485069079));
#20060=CARTESIAN_POINT('Ctrl Pts',(-24.0959501711783,26.1506751237818,171.507305910281));
#20061=CARTESIAN_POINT('Ctrl Pts',(-24.0306335816867,26.1589090053693,170.99304475765));
#20062=CARTESIAN_POINT('Ctrl Pts',(-23.9698304921285,25.6452096731348,171.010423173625));
#20063=CARTESIAN_POINT('Ctrl Pts',(-23.6431960794649,26.2077498058528,171.593014493502));
#20064=CARTESIAN_POINT('Ctrl Pts',(-23.5111338715838,26.2243977139913,171.073389718607));
#20065=CARTESIAN_POINT('Ctrl Pts',(-23.4549281292755,25.6932274759485,171.108375839534));
#20066=CARTESIAN_POINT('Ctrl Pts',(-23.4183852446137,26.2360897085949,171.657722381639));
#20067=CARTESIAN_POINT('Ctrl Pts',(-23.2514992137756,26.2571275464109,171.139086040182));
#20068=CARTESIAN_POINT('Ctrl Pts',(-23.1992466423954,25.717109596163,171.182327711039));
#20069=CARTESIAN_POINT('Ctrl Pts',(-22.9858808239905,26.2906116947088,171.828488317232));
#20070=CARTESIAN_POINT('Ctrl Pts',(-22.7480513169311,26.3205927456837,171.318813609326));
#20071=CARTESIAN_POINT('Ctrl Pts',(-22.7073317369307,25.7631231310235,171.37748878222));
#20072=CARTESIAN_POINT('Ctrl Pts',(-22.780301002694,26.3165273145905,171.933235555643));
#20073=CARTESIAN_POINT('Ctrl Pts',(-22.5072292845117,26.3509510377182,171.432160965498));
#20074=CARTESIAN_POINT('Ctrl Pts',(-22.473502682735,25.7850288237937,171.497199911615));
#20075=CARTESIAN_POINT('Ctrl Pts',(-22.3903890997892,26.3656800407642,172.181282504714));
#20076=CARTESIAN_POINT('Ctrl Pts',(-22.046448768076,26.4090375397752,171.705429397239));
#20077=CARTESIAN_POINT('Ctrl Pts',(-22.029997004347,25.8266280231631,171.780682137627));
#20078=CARTESIAN_POINT('Ctrl Pts',(-22.2042811099175,26.3891410200181,172.326561495445));
#20079=CARTESIAN_POINT('Ctrl Pts',(-21.8251478033509,26.4369349844039,171.86812412086));
#20080=CARTESIAN_POINT('Ctrl Pts',(-21.8183001416767,25.8465117976671,171.946715270196));
#20081=CARTESIAN_POINT('Ctrl Pts',(-21.8682914406808,26.4314962497153,172.646838591123));
#20082=CARTESIAN_POINT('Ctrl Pts',(-21.4220077743163,26.4877552628029,172.231518296184));
#20083=CARTESIAN_POINT('Ctrl Pts',(-21.4361029074071,25.8824462409076,172.312746237574));
#20084=CARTESIAN_POINT('Ctrl Pts',(-21.7172904392047,26.4505316031431,172.821893236395));
#20085=CARTESIAN_POINT('Ctrl Pts',(-21.23986603748,26.510716251808,172.432383047633));
#20086=CARTESIAN_POINT('Ctrl Pts',(-21.2643295137859,25.8986157996259,172.512808689673));
#20087=CARTESIAN_POINT('Ctrl Pts',(-21.4500317056124,26.484222534997,173.202497941726));
#20088=CARTESIAN_POINT('Ctrl Pts',(-20.9146824604562,26.5517092535569,172.873679335507));
#20089=CARTESIAN_POINT('Ctrl Pts',(-20.9602991882961,25.9272562971409,172.947785494157));
#20090=CARTESIAN_POINT('Ctrl Pts',(-21.3340158032727,26.4988476280937,173.409042585785));
#20091=CARTESIAN_POINT('Ctrl Pts',(-20.7729608251139,26.569574839814,173.115030751227));
#20092=CARTESIAN_POINT('Ctrl Pts',(-20.8283172958717,25.9397015531057,173.183836516651));
#20093=CARTESIAN_POINT('Ctrl Pts',(-21.1488654481888,26.522187886846,173.83457432462));
#20094=CARTESIAN_POINT('Ctrl Pts',(-20.5450665743191,26.598303441388,173.616334746953));
#20095=CARTESIAN_POINT('Ctrl Pts',(-20.6176840378571,25.9595724331803,173.670158504074));
#20096=CARTESIAN_POINT('Ctrl Pts',(-21.0779351096429,26.5311294438541,174.055717854822));
#20097=CARTESIAN_POINT('Ctrl Pts',(-20.4575919717946,26.6093305866297,173.878021756473));
#20098=CARTESIAN_POINT('Ctrl Pts',(-20.5369896936467,25.9671905184219,173.922893967463));
#20099=CARTESIAN_POINT('Ctrl Pts',(-20.9814287704556,26.5432951398197,174.515559365905));
#20100=CARTESIAN_POINT('Ctrl Pts',(-20.3378990677518,26.6244192066291,174.425122401938));
#20101=CARTESIAN_POINT('Ctrl Pts',(-20.427198146352,25.9775572759958,174.448427122202));
#20102=CARTESIAN_POINT('Ctrl Pts',(-20.9569943894572,26.546375364941,174.750471985775));
#20103=CARTESIAN_POINT('Ctrl Pts',(-20.3076118897997,26.6282372418308,174.704913517301));
#20104=CARTESIAN_POINT('Ctrl Pts',(-20.3993997459849,25.9801832412446,174.716898688454));
#20105=CARTESIAN_POINT('Ctrl Pts',(-20.9569943874949,26.5463753651883,174.985485069079));
#20106=CARTESIAN_POINT('Ctrl Pts',(-20.3076118873532,26.6282372421243,174.985485069079));
#20107=CARTESIAN_POINT('Ctrl Pts',(-20.3993997459139,25.9801832417458,174.985485069079));
#20108=CARTESIAN_POINT('Origin',(-24.4968854027286,25.5961755932732,171.485485069079));
#20109=CARTESIAN_POINT('Origin',(-55.3387939853426,21.7082104505275,171.485485069079));
#20110=CARTESIAN_POINT('Origin',(-41.2825923197859,23.4801507949034,171.485485069079));
#20111=CARTESIAN_POINT('Origin',(-39.4690592605811,9.0940082318961,171.485485069079));
#20112=CARTESIAN_POINT('Origin',(-53.9352248596064,8.10403203946808,171.485485069079));
#20113=CARTESIAN_POINT('Origin',(-52.4446243855275,-13.6775759072102,171.485485069079));
#20114=CARTESIAN_POINT('Origin',(-52.5342226896633,-12.3683081541722,171.485485069079));
#20115=CARTESIAN_POINT('Origin',(-67.998054881725,-13.4265585667677,171.485485069079));
#20116=CARTESIAN_POINT('Origin',(-52.5853897920404,-15.069651635714,171.485485069079));
#20117=CARTESIAN_POINT('Origin',(-62.88786637536,-111.709716750739,171.485485069079));
#20118=CARTESIAN_POINT('Ctrl Pts',(-56.2237961054143,-113.614380048479,
178.813912075476));
#20119=CARTESIAN_POINT('Ctrl Pts',(-55.0488864554725,-113.645352038053,
177.6423391512));
#20120=CARTESIAN_POINT('Ctrl Pts',(-55.0389484614927,-113.552130266048,
175.985484901707));
#20121=CARTESIAN_POINT('Ctrl Pts',(-55.0290104675128,-113.458908494044,
174.328630652215));
#20122=CARTESIAN_POINT('Ctrl Pts',(-56.1840440891124,-113.241492964766,
173.157057825983));
#20123=CARTESIAN_POINT('Ctrl Pts',(-57.3390777107121,-113.024077435489,
171.985484999752));
#20124=CARTESIAN_POINT('Ctrl Pts',(-58.9766583348819,-112.755219171892,
171.985485069079));
#20125=CARTESIAN_POINT('Ctrl Pts',(-60.6142389590518,-112.486360908295,
171.985485138407));
#20126=CARTESIAN_POINT('Ctrl Pts',(-61.7692724831595,-112.268945389411,
173.157058062683));
#20127=CARTESIAN_POINT('Ctrl Pts',(-62.9243060072673,-112.051529870527,
174.328630986959));
#20128=CARTESIAN_POINT('Ctrl Pts',(-62.9143678754131,-111.95830811322,175.985485236451));
#20129=CARTESIAN_POINT('Ctrl Pts',(-62.9044297435589,-111.865086355914,
177.642339485944));
#20130=CARTESIAN_POINT('Ctrl Pts',(-61.7295199961253,-111.896058355881,
178.813912312176));
#20131=CARTESIAN_POINT('Ctrl Pts',(-60.5546102486917,-111.927030355848,
179.985485138407));
#20132=CARTESIAN_POINT('Ctrl Pts',(-58.8971534986878,-112.009445090134,
179.985485069079));
#20133=CARTESIAN_POINT('Ctrl Pts',(-57.2396967486839,-112.09185982442,179.985484999752));
#20134=CARTESIAN_POINT('Ctrl Pts',(-56.0647870987421,-112.122831813994,
178.813912075476));
#20135=CARTESIAN_POINT('Ctrl Pts',(-54.8898774488003,-112.153803803567,
177.6423391512));
#20136=CARTESIAN_POINT('Ctrl Pts',(-54.8799394548205,-112.060582031563,
175.985484901707));
#20137=CARTESIAN_POINT('Ctrl Pts',(-54.8700014608406,-111.967360259558,
174.328630652215));
#20138=CARTESIAN_POINT('Ctrl Pts',(-56.0250350824402,-111.749944730281,
173.157057825983));
#20139=CARTESIAN_POINT('Ctrl Pts',(-57.1800687040398,-111.532529201003,
171.985484999752));
#20140=CARTESIAN_POINT('Ctrl Pts',(-58.8176493282097,-111.263670937406,
171.985485069079));
#20141=CARTESIAN_POINT('Ctrl Pts',(-60.4552299523796,-110.994812673809,
171.985485138407));
#20142=CARTESIAN_POINT('Ctrl Pts',(-61.6102634764873,-110.777397154925,
173.157058062683));
#20143=CARTESIAN_POINT('Ctrl Pts',(-62.7652970005951,-110.559981636041,
174.328630986959));
#20144=CARTESIAN_POINT('Ctrl Pts',(-62.7553588687409,-110.466759878735,
175.985485236451));
#20145=CARTESIAN_POINT('Ctrl Pts',(-62.7454207368867,-110.373538121429,
177.642339485944));
#20146=CARTESIAN_POINT('Ctrl Pts',(-61.5705109894531,-110.404510121395,
178.813912312176));
#20147=CARTESIAN_POINT('Ctrl Pts',(-60.3956012420194,-110.435482121362,
179.985485138407));
#20148=CARTESIAN_POINT('Ctrl Pts',(-58.7381444920155,-110.517896855648,
179.985485069079));
#20149=CARTESIAN_POINT('Ctrl Pts',(-57.0806877420116,-110.600311589935,
179.985484999752));
#20150=CARTESIAN_POINT('Ctrl Pts',(-55.9057780920699,-110.631283579508,
178.813912075476));
#20151=CARTESIAN_POINT('Ctrl Pts',(-54.7308684421281,-110.662255569082,
177.6423391512));
#20152=CARTESIAN_POINT('Ctrl Pts',(-54.7209304481482,-110.569033797077,
175.985484901707));
#20153=CARTESIAN_POINT('Ctrl Pts',(-54.7109924541684,-110.475812025073,
174.328630652215));
#20154=CARTESIAN_POINT('Ctrl Pts',(-55.866026075768,-110.258396495795,173.157057825983));
#20155=CARTESIAN_POINT('Ctrl Pts',(-57.0210596973676,-110.040980966518,
171.985484999752));
#20156=CARTESIAN_POINT('Ctrl Pts',(-58.6586403215375,-109.772122702921,
171.985485069079));
#20157=CARTESIAN_POINT('Ctrl Pts',(-60.2962209457073,-109.503264439324,
171.985485138407));
#20158=CARTESIAN_POINT('Ctrl Pts',(-61.4512544698151,-109.28584892044,173.157058062683));
#20159=CARTESIAN_POINT('Ctrl Pts',(-62.6062879939228,-109.068433401555,
174.328630986959));
#20160=CARTESIAN_POINT('Ctrl Pts',(-62.5963498620687,-108.975211644249,
175.985485236451));
#20161=CARTESIAN_POINT('Ctrl Pts',(-62.5864117302145,-108.881989886943,
177.642339485944));
#20162=CARTESIAN_POINT('Ctrl Pts',(-61.4115019827808,-108.91296188691,178.813912312176));
#20163=CARTESIAN_POINT('Ctrl Pts',(-60.2365922353472,-108.943933886877,
179.985485138407));
#20164=CARTESIAN_POINT('Ctrl Pts',(-58.5791354853433,-109.026348621163,
179.985485069079));
#20165=CARTESIAN_POINT('Ctrl Pts',(-56.9216787353394,-109.108763355449,
179.985484999752));
#20166=CARTESIAN_POINT('Ctrl Pts',(-55.7467690853976,-109.139735345023,
178.813912075476));
#20167=CARTESIAN_POINT('Ctrl Pts',(-54.5718594354559,-109.170707334596,
177.6423391512));
#20168=CARTESIAN_POINT('Ctrl Pts',(-54.561921441476,-109.077485562592,175.985484901707));
#20169=CARTESIAN_POINT('Ctrl Pts',(-54.5519834474962,-108.984263790587,
174.328630652215));
#20170=CARTESIAN_POINT('Ctrl Pts',(-55.7070170690958,-108.76684826131,173.157057825983));
#20171=CARTESIAN_POINT('Ctrl Pts',(-56.8620506906954,-108.549432732032,
171.985484999752));
#20172=CARTESIAN_POINT('Ctrl Pts',(-58.4996313148652,-108.280574468435,
171.985485069079));
#20173=CARTESIAN_POINT('Ctrl Pts',(-60.1372119390351,-108.011716204838,
171.985485138407));
#20174=CARTESIAN_POINT('Ctrl Pts',(-61.2922454631428,-107.794300685954,
173.157058062683));
#20175=CARTESIAN_POINT('Ctrl Pts',(-62.4472789872506,-107.57688516707,174.328630986959));
#20176=CARTESIAN_POINT('Ctrl Pts',(-62.4373408553964,-107.483663409764,
175.985485236451));
#20177=CARTESIAN_POINT('Ctrl Pts',(-62.4274027235423,-107.390441652457,
177.642339485944));
#20178=CARTESIAN_POINT('Ctrl Pts',(-61.2524929761086,-107.421413652424,
178.813912312176));
#20179=CARTESIAN_POINT('Ctrl Pts',(-60.077583228675,-107.452385652391,179.985485138407));
#20180=CARTESIAN_POINT('Ctrl Pts',(-58.4201264786711,-107.534800386677,
179.985485069079));
#20181=CARTESIAN_POINT('Ctrl Pts',(-56.7626697286672,-107.617215120964,
179.985484999752));
#20182=CARTESIAN_POINT('Ctrl Pts',(-55.5877600787254,-107.648187110537,
178.813912075476));
#20183=CARTESIAN_POINT('Ctrl Pts',(-54.4128504287836,-107.67915910011,177.6423391512));
#20184=CARTESIAN_POINT('Ctrl Pts',(-54.4029124348038,-107.585937328106,
175.985484901707));
#20185=CARTESIAN_POINT('Ctrl Pts',(-54.3929744408239,-107.492715556102,
174.328630652215));
#20186=CARTESIAN_POINT('Ctrl Pts',(-55.5480080624235,-107.275300026824,
173.157057825983));
#20187=CARTESIAN_POINT('Ctrl Pts',(-56.7030416840231,-107.057884497547,
171.985484999752));
#20188=CARTESIAN_POINT('Ctrl Pts',(-58.340622308193,-106.78902623395,171.985485069079));
#20189=CARTESIAN_POINT('Ctrl Pts',(-59.9782029323629,-106.520167970353,
171.985485138407));
#20190=CARTESIAN_POINT('Ctrl Pts',(-61.1332364564706,-106.302752451468,
173.157058062683));
#20191=CARTESIAN_POINT('Ctrl Pts',(-62.2882699805784,-106.085336932584,
174.328630986959));
#20192=CARTESIAN_POINT('Ctrl Pts',(-62.2783318487242,-105.992115175278,
175.985485236451));
#20193=CARTESIAN_POINT('Ctrl Pts',(-62.26839371687,-105.898893417972,177.642339485944));
#20194=CARTESIAN_POINT('Ctrl Pts',(-61.0934839694364,-105.929865417939,
178.813912312176));
#20195=CARTESIAN_POINT('Ctrl Pts',(-59.9185742220028,-105.960837417905,
179.985485138407));
#20196=CARTESIAN_POINT('Ctrl Pts',(-58.2611174719989,-106.043252152192,
179.985485069079));
#20197=CARTESIAN_POINT('Ctrl Pts',(-56.603660721995,-106.125666886478,179.985484999752));
#20198=CARTESIAN_POINT('Ctrl Pts',(-55.4287510720532,-106.156638876051,
178.813912075476));
#20199=CARTESIAN_POINT('Ctrl Pts',(-54.2538414221114,-106.187610865625,
177.6423391512));
#20200=CARTESIAN_POINT('Ctrl Pts',(-54.2439034281315,-106.09438909362,175.985484901707));
#20201=CARTESIAN_POINT('Ctrl Pts',(-54.2339654341517,-106.001167321616,
174.328630652215));
#20202=CARTESIAN_POINT('Ctrl Pts',(-55.3889990557513,-105.783751792338,
173.157057825983));
#20203=CARTESIAN_POINT('Ctrl Pts',(-56.5440326773509,-105.566336263061,
171.985484999752));
#20204=CARTESIAN_POINT('Ctrl Pts',(-58.1816133015208,-105.297477999464,
171.985485069079));
#20205=CARTESIAN_POINT('Ctrl Pts',(-59.8191939256906,-105.028619735867,
171.985485138407));
#20206=CARTESIAN_POINT('Ctrl Pts',(-60.9742274497984,-104.811204216983,
173.157058062683));
#20207=CARTESIAN_POINT('Ctrl Pts',(-62.1292609739061,-104.593788698099,
174.328630986959));
#20208=CARTESIAN_POINT('Ctrl Pts',(-62.119322842052,-104.500566940792,175.985485236451));
#20209=CARTESIAN_POINT('Ctrl Pts',(-62.1093847101978,-104.407345183486,
177.642339485944));
#20210=CARTESIAN_POINT('Ctrl Pts',(-60.9344749627642,-104.438317183453,
178.813912312176));
#20211=CARTESIAN_POINT('Ctrl Pts',(-59.7595652153305,-104.46928918342,179.985485138407));
#20212=CARTESIAN_POINT('Ctrl Pts',(-58.1021084653266,-104.551703917706,
179.985485069079));
#20213=CARTESIAN_POINT('Ctrl Pts',(-56.4446517153227,-104.634118651992,
179.985484999752));
#20214=CARTESIAN_POINT('Ctrl Pts',(-55.269742065381,-104.665090641566,178.813912075476));
#20215=CARTESIAN_POINT('Ctrl Pts',(-54.0948324154392,-104.696062631139,
177.6423391512));
#20216=CARTESIAN_POINT('Ctrl Pts',(-54.0848944214593,-104.602840859135,
175.985484901707));
#20217=CARTESIAN_POINT('Ctrl Pts',(-54.0749564274795,-104.50961908713,174.328630652215));
#20218=CARTESIAN_POINT('Ctrl Pts',(-55.2299900490791,-104.292203557853,
173.157057825983));
#20219=CARTESIAN_POINT('Ctrl Pts',(-56.3850236706787,-104.074788028575,
171.985484999752));
#20220=CARTESIAN_POINT('Ctrl Pts',(-58.0226042948486,-103.805929764978,
171.985485069079));
#20221=CARTESIAN_POINT('Ctrl Pts',(-59.6601849190184,-103.537071501381,
171.985485138407));
#20222=CARTESIAN_POINT('Ctrl Pts',(-60.8152184431262,-103.319655982497,
173.157058062683));
#20223=CARTESIAN_POINT('Ctrl Pts',(-61.9702519672339,-103.102240463613,
174.328630986959));
#20224=CARTESIAN_POINT('Ctrl Pts',(-61.9603138353797,-103.009018706307,
175.985485236451));
#20225=CARTESIAN_POINT('Ctrl Pts',(-61.9503757035256,-102.915796949001,
177.642339485944));
#20226=CARTESIAN_POINT('Ctrl Pts',(-60.7754659560919,-102.946768948967,
178.813912312176));
#20227=CARTESIAN_POINT('Ctrl Pts',(-59.6005562086583,-102.977740948934,
179.985485138407));
#20228=CARTESIAN_POINT('Ctrl Pts',(-57.9430994586544,-103.06015568322,179.985485069079));
#20229=CARTESIAN_POINT('Ctrl Pts',(-56.2856427086505,-103.142570417507,
179.985484999752));
#20230=CARTESIAN_POINT('Ctrl Pts',(-55.1107330587087,-103.17354240708,178.813912075476));
#20231=CARTESIAN_POINT('Ctrl Pts',(-53.935823408767,-103.204514396654,177.6423391512));
#20232=CARTESIAN_POINT('Ctrl Pts',(-53.9258854147871,-103.111292624649,
175.985484901707));
#20233=CARTESIAN_POINT('Ctrl Pts',(-53.9159474208072,-103.018070852645,
174.328630652215));
#20234=CARTESIAN_POINT('Ctrl Pts',(-55.0709810424069,-102.800655323367,
173.157057825983));
#20235=CARTESIAN_POINT('Ctrl Pts',(-56.2260146640065,-102.58323979409,171.985484999752));
#20236=CARTESIAN_POINT('Ctrl Pts',(-57.8635952881763,-102.314381530493,
171.985485069079));
#20237=CARTESIAN_POINT('Ctrl Pts',(-59.5011759123462,-102.045523266896,
171.985485138407));
#20238=CARTESIAN_POINT('Ctrl Pts',(-60.6562094364539,-101.828107748012,
173.157058062683));
#20239=CARTESIAN_POINT('Ctrl Pts',(-61.8112429605617,-101.610692229127,
174.328630986959));
#20240=CARTESIAN_POINT('Ctrl Pts',(-61.8013048287075,-101.517470471821,
175.985485236451));
#20241=CARTESIAN_POINT('Ctrl Pts',(-61.7913666968533,-101.424248714515,
177.642339485944));
#20242=CARTESIAN_POINT('Ctrl Pts',(-60.6164569494197,-101.455220714482,
178.813912312176));
#20243=CARTESIAN_POINT('Ctrl Pts',(-59.4415472019861,-101.486192714449,
179.985485138407));
#20244=CARTESIAN_POINT('Ctrl Pts',(-57.7840904519822,-101.568607448735,
179.985485069079));
#20245=CARTESIAN_POINT('Ctrl Pts',(-56.1266337019783,-101.651022183021,
179.985484999752));
#20246=CARTESIAN_POINT('Ctrl Pts',(-54.9517240520365,-101.681994172595,
178.813912075476));
#20247=CARTESIAN_POINT('Ctrl Pts',(-53.7768144020947,-101.712966162168,
177.6423391512));
#20248=CARTESIAN_POINT('Ctrl Pts',(-53.7668764081149,-101.619744390164,
175.985484901707));
#20249=CARTESIAN_POINT('Ctrl Pts',(-53.756938414135,-101.526522618159,174.328630652215));
#20250=CARTESIAN_POINT('Ctrl Pts',(-54.9119720357346,-101.309107088882,
173.157057825983));
#20251=CARTESIAN_POINT('Ctrl Pts',(-56.0670056573342,-101.091691559604,
171.985484999752));
#20252=CARTESIAN_POINT('Ctrl Pts',(-57.7045862815041,-100.822833296007,
171.985485069079));
#20253=CARTESIAN_POINT('Ctrl Pts',(-59.342166905674,-100.55397503241,171.985485138407));
#20254=CARTESIAN_POINT('Ctrl Pts',(-60.4972004297817,-100.336559513526,
173.157058062683));
#20255=CARTESIAN_POINT('Ctrl Pts',(-61.6522339538895,-100.119143994642,
174.328630986959));
#20256=CARTESIAN_POINT('Ctrl Pts',(-61.6422958220353,-100.025922237336,
175.985485236451));
#20257=CARTESIAN_POINT('Ctrl Pts',(-61.6323576901811,-99.9327004800294,
177.642339485944));
#20258=CARTESIAN_POINT('Ctrl Pts',(-60.4574479427475,-99.9636724799962,
178.813912312176));
#20259=CARTESIAN_POINT('Ctrl Pts',(-59.2825381953138,-99.994644479963,179.985485138407));
#20260=CARTESIAN_POINT('Ctrl Pts',(-57.6250814453099,-100.077059214249,
179.985485069079));
#20261=CARTESIAN_POINT('Ctrl Pts',(-55.9676246953061,-100.159473948536,
179.985484999752));
#20262=CARTESIAN_POINT('Ctrl Pts',(-54.7927150453643,-100.190445938109,
178.813912075476));
#20263=CARTESIAN_POINT('Ctrl Pts',(-53.6178053954225,-100.221417927683,
177.6423391512));
#20264=CARTESIAN_POINT('Ctrl Pts',(-53.6078674014426,-100.128196155678,
175.985484901707));
#20265=CARTESIAN_POINT('Ctrl Pts',(-53.5979294074628,-100.034974383673,
174.328630652215));
#20266=CARTESIAN_POINT('Ctrl Pts',(-54.7529630290624,-99.817558854396,173.157057825983));
#20267=CARTESIAN_POINT('Ctrl Pts',(-55.907996650662,-99.6001433251185,171.985484999752));
#20268=CARTESIAN_POINT('Ctrl Pts',(-57.5455772748319,-99.3312850615215,
171.985485069079));
#20269=CARTESIAN_POINT('Ctrl Pts',(-59.1831578990017,-99.0624267979246,
171.985485138407));
#20270=CARTESIAN_POINT('Ctrl Pts',(-60.3381914231095,-98.8450112790404,
173.157058062683));
#20271=CARTESIAN_POINT('Ctrl Pts',(-61.4932249472172,-98.6275957601562,
174.328630986959));
#20272=CARTESIAN_POINT('Ctrl Pts',(-61.4832868153631,-98.53437400285,175.985485236451));
#20273=CARTESIAN_POINT('Ctrl Pts',(-61.4733486835089,-98.4411522455438,
177.642339485944));
#20274=CARTESIAN_POINT('Ctrl Pts',(-60.2984389360752,-98.4721242455106,
178.813912312176));
#20275=CARTESIAN_POINT('Ctrl Pts',(-59.1235291886416,-98.5030962454774,
179.985485138407));
#20276=CARTESIAN_POINT('Ctrl Pts',(-57.4660724386377,-98.5855109797636,
179.985485069079));
#20277=CARTESIAN_POINT('Ctrl Pts',(-55.8086156886338,-98.6679257140499,
179.985484999752));
#20278=CARTESIAN_POINT('Ctrl Pts',(-54.633706038692,-98.6988977036234,178.813912075476));
#20279=CARTESIAN_POINT('Ctrl Pts',(-56.9964983346804,-113.864655531781,
178.072094410988));
#20280=CARTESIAN_POINT('Ctrl Pts',(-56.1271283009022,-113.863054956993,
177.207792449865));
#20281=CARTESIAN_POINT('Ctrl Pts',(-56.117190288842,-113.769833186916,175.985484945604));
#20282=CARTESIAN_POINT('Ctrl Pts',(-56.1072522767819,-113.676611416839,
174.763177441344));
#20283=CARTESIAN_POINT('Ctrl Pts',(-56.9567462566485,-113.491768454648,
173.89887555255));
#20284=CARTESIAN_POINT('Ctrl Pts',(-57.8062402365152,-113.306925492458,
173.034573663757));
#20285=CARTESIAN_POINT('Ctrl Pts',(-59.011722573584,-113.084131793069,173.034573714903));
#20286=CARTESIAN_POINT('Ctrl Pts',(-60.2172049106529,-112.86133809368,173.034573766048));
#20287=CARTESIAN_POINT('Ctrl Pts',(-61.0666988185971,-112.676495139156,
173.898875727171));
#20288=CARTESIAN_POINT('Ctrl Pts',(-61.9161927265413,-112.491652184633,
174.763177688294));
#20289=CARTESIAN_POINT('Ctrl Pts',(-61.9062546127674,-112.398430425399,
175.985485192554));
#20290=CARTESIAN_POINT('Ctrl Pts',(-61.8963164989935,-112.305208666166,
177.207792696815));
#20291=CARTESIAN_POINT('Ctrl Pts',(-61.0269463932928,-112.303608099046,
178.072094585608));
#20292=CARTESIAN_POINT('Ctrl Pts',(-60.1575762875921,-112.302007531926,
178.936396474401));
#20293=CARTESIAN_POINT('Ctrl Pts',(-58.9322178246893,-112.338357702004,
178.936396423256));
#20294=CARTESIAN_POINT('Ctrl Pts',(-57.7068593617864,-112.374707872082,
178.936396372111));
#20295=CARTESIAN_POINT('Ctrl Pts',(-56.8374893280082,-112.373107297295,
178.072094410988));
#20296=CARTESIAN_POINT('Ctrl Pts',(-55.9681192942299,-112.371506722508,
177.207792449865));
#20297=CARTESIAN_POINT('Ctrl Pts',(-55.9581812821698,-112.278284952431,
175.985484945604));
#20298=CARTESIAN_POINT('Ctrl Pts',(-55.9482432701096,-112.185063182354,
174.763177441344));
#20299=CARTESIAN_POINT('Ctrl Pts',(-56.7977372499763,-112.000220220163,
173.89887555255));
#20300=CARTESIAN_POINT('Ctrl Pts',(-57.647231229843,-111.815377257972,173.034573663757));
#20301=CARTESIAN_POINT('Ctrl Pts',(-58.8527135669118,-111.592583558583,
173.034573714903));
#20302=CARTESIAN_POINT('Ctrl Pts',(-60.0581959039807,-111.369789859194,
173.034573766048));
#20303=CARTESIAN_POINT('Ctrl Pts',(-60.9076898119249,-111.184946904671,
173.898875727171));
#20304=CARTESIAN_POINT('Ctrl Pts',(-61.7571837198691,-111.000103950148,
174.763177688294));
#20305=CARTESIAN_POINT('Ctrl Pts',(-61.7472456060952,-110.906882190914,
175.985485192554));
#20306=CARTESIAN_POINT('Ctrl Pts',(-61.7373074923213,-110.81366043168,177.207792696815));
#20307=CARTESIAN_POINT('Ctrl Pts',(-60.8679373866206,-110.81205986456,178.072094585608));
#20308=CARTESIAN_POINT('Ctrl Pts',(-59.9985672809199,-110.81045929744,178.936396474401));
#20309=CARTESIAN_POINT('Ctrl Pts',(-58.7732088180171,-110.846809467519,
178.936396423256));
#20310=CARTESIAN_POINT('Ctrl Pts',(-57.5478503551142,-110.883159637597,
178.936396372111));
#20311=CARTESIAN_POINT('Ctrl Pts',(-56.6784803213359,-110.881559062809,
178.072094410988));
#20312=CARTESIAN_POINT('Ctrl Pts',(-55.8091102875577,-110.879958488022,
177.207792449865));
#20313=CARTESIAN_POINT('Ctrl Pts',(-55.7991722754976,-110.786736717945,
175.985484945604));
#20314=CARTESIAN_POINT('Ctrl Pts',(-55.7892342634374,-110.693514947868,
174.763177441344));
#20315=CARTESIAN_POINT('Ctrl Pts',(-56.6387282433041,-110.508671985677,
173.89887555255));
#20316=CARTESIAN_POINT('Ctrl Pts',(-57.4882222231708,-110.323829023487,
173.034573663757));
#20317=CARTESIAN_POINT('Ctrl Pts',(-58.6937045602396,-110.101035324098,
173.034573714903));
#20318=CARTESIAN_POINT('Ctrl Pts',(-59.8991868973084,-109.878241624709,
173.034573766048));
#20319=CARTESIAN_POINT('Ctrl Pts',(-60.7486808052526,-109.693398670185,
173.898875727171));
#20320=CARTESIAN_POINT('Ctrl Pts',(-61.5981747131968,-109.508555715662,
174.763177688294));
#20321=CARTESIAN_POINT('Ctrl Pts',(-61.588236599423,-109.415333956428,175.985485192554));
#20322=CARTESIAN_POINT('Ctrl Pts',(-61.5782984856491,-109.322112197195,
177.207792696815));
#20323=CARTESIAN_POINT('Ctrl Pts',(-60.7089283799484,-109.320511630075,
178.072094585608));
#20324=CARTESIAN_POINT('Ctrl Pts',(-59.8395582742477,-109.318911062955,
178.936396474401));
#20325=CARTESIAN_POINT('Ctrl Pts',(-58.6141998113448,-109.355261233033,
178.936396423256));
#20326=CARTESIAN_POINT('Ctrl Pts',(-57.388841348442,-109.391611403111,178.936396372111));
#20327=CARTESIAN_POINT('Ctrl Pts',(-56.5194713146637,-109.390010828324,
178.072094410988));
#20328=CARTESIAN_POINT('Ctrl Pts',(-55.6501012808855,-109.388410253536,
177.207792449865));
#20329=CARTESIAN_POINT('Ctrl Pts',(-55.6401632688253,-109.295188483459,
175.985484945604));
#20330=CARTESIAN_POINT('Ctrl Pts',(-55.6302252567652,-109.201966713382,
174.763177441344));
#20331=CARTESIAN_POINT('Ctrl Pts',(-56.4797192366319,-109.017123751192,
173.89887555255));
#20332=CARTESIAN_POINT('Ctrl Pts',(-57.3292132164985,-108.832280789001,
173.034573663757));
#20333=CARTESIAN_POINT('Ctrl Pts',(-58.5346955535674,-108.609487089612,
173.034573714903));
#20334=CARTESIAN_POINT('Ctrl Pts',(-59.7401778906362,-108.386693390223,
173.034573766048));
#20335=CARTESIAN_POINT('Ctrl Pts',(-60.5896717985804,-108.2018504357,173.898875727171));
#20336=CARTESIAN_POINT('Ctrl Pts',(-61.4391657065246,-108.017007481176,
174.763177688294));
#20337=CARTESIAN_POINT('Ctrl Pts',(-61.4292275927507,-107.923785721943,
175.985485192554));
#20338=CARTESIAN_POINT('Ctrl Pts',(-61.4192894789769,-107.830563962709,
177.207792696815));
#20339=CARTESIAN_POINT('Ctrl Pts',(-60.5499193732762,-107.828963395589,
178.072094585608));
#20340=CARTESIAN_POINT('Ctrl Pts',(-59.6805492675755,-107.827362828469,
178.936396474401));
#20341=CARTESIAN_POINT('Ctrl Pts',(-58.4551908046726,-107.863712998547,
178.936396423256));
#20342=CARTESIAN_POINT('Ctrl Pts',(-57.2298323417698,-107.900063168626,
178.936396372111));
#20343=CARTESIAN_POINT('Ctrl Pts',(-56.3604623079915,-107.898462593838,
178.072094410988));
#20344=CARTESIAN_POINT('Ctrl Pts',(-55.4910922742133,-107.896862019051,
177.207792449865));
#20345=CARTESIAN_POINT('Ctrl Pts',(-55.4811542621531,-107.803640248974,
175.985484945604));
#20346=CARTESIAN_POINT('Ctrl Pts',(-55.471216250093,-107.710418478897,174.763177441344));
#20347=CARTESIAN_POINT('Ctrl Pts',(-56.3207102299596,-107.525575516706,
173.89887555255));
#20348=CARTESIAN_POINT('Ctrl Pts',(-57.1702042098263,-107.340732554515,
173.034573663757));
#20349=CARTESIAN_POINT('Ctrl Pts',(-58.3756865468951,-107.117938855126,
173.034573714903));
#20350=CARTESIAN_POINT('Ctrl Pts',(-59.581168883964,-106.895145155737,173.034573766048));
#20351=CARTESIAN_POINT('Ctrl Pts',(-60.4306627919082,-106.710302201214,
173.898875727171));
#20352=CARTESIAN_POINT('Ctrl Pts',(-61.2801566998524,-106.525459246691,
174.763177688294));
#20353=CARTESIAN_POINT('Ctrl Pts',(-61.2702185860785,-106.432237487457,
175.985485192554));
#20354=CARTESIAN_POINT('Ctrl Pts',(-61.2602804723046,-106.339015728223,
177.207792696815));
#20355=CARTESIAN_POINT('Ctrl Pts',(-60.3909103666039,-106.337415161103,
178.072094585608));
#20356=CARTESIAN_POINT('Ctrl Pts',(-59.5215402609032,-106.335814593983,
178.936396474401));
#20357=CARTESIAN_POINT('Ctrl Pts',(-58.2961817980004,-106.372164764062,
178.936396423256));
#20358=CARTESIAN_POINT('Ctrl Pts',(-57.0708233350975,-106.40851493414,178.936396372111));
#20359=CARTESIAN_POINT('Ctrl Pts',(-56.2014533013193,-106.406914359353,
178.072094410988));
#20360=CARTESIAN_POINT('Ctrl Pts',(-55.332083267541,-106.405313784565,177.207792449865));
#20361=CARTESIAN_POINT('Ctrl Pts',(-55.3221452554809,-106.312092014488,
175.985484945604));
#20362=CARTESIAN_POINT('Ctrl Pts',(-55.3122072434207,-106.218870244411,
174.763177441344));
#20363=CARTESIAN_POINT('Ctrl Pts',(-56.1617012232874,-106.034027282221,
173.89887555255));
#20364=CARTESIAN_POINT('Ctrl Pts',(-57.0111952031541,-105.84918432003,173.034573663757));
#20365=CARTESIAN_POINT('Ctrl Pts',(-58.2166775402229,-105.626390620641,
173.034573714903));
#20366=CARTESIAN_POINT('Ctrl Pts',(-59.4221598772917,-105.403596921252,
173.034573766048));
#20367=CARTESIAN_POINT('Ctrl Pts',(-60.2716537852359,-105.218753966728,
173.898875727171));
#20368=CARTESIAN_POINT('Ctrl Pts',(-61.1211476931802,-105.033911012205,
174.763177688294));
#20369=CARTESIAN_POINT('Ctrl Pts',(-61.1112095794063,-104.940689252971,
175.985485192554));
#20370=CARTESIAN_POINT('Ctrl Pts',(-61.1012714656324,-104.847467493738,
177.207792696815));
#20371=CARTESIAN_POINT('Ctrl Pts',(-60.2319013599317,-104.845866926618,
178.072094585608));
#20372=CARTESIAN_POINT('Ctrl Pts',(-59.362531254231,-104.844266359498,178.936396474401));
#20373=CARTESIAN_POINT('Ctrl Pts',(-58.1371727913281,-104.880616529576,
178.936396423256));
#20374=CARTESIAN_POINT('Ctrl Pts',(-56.9118143284253,-104.916966699654,
178.936396372111));
#20375=CARTESIAN_POINT('Ctrl Pts',(-56.042444294647,-104.915366124867,178.072094410988));
#20376=CARTESIAN_POINT('Ctrl Pts',(-55.1730742608688,-104.91376555008,177.207792449865));
#20377=CARTESIAN_POINT('Ctrl Pts',(-55.1631362488087,-104.820543780003,
175.985484945604));
#20378=CARTESIAN_POINT('Ctrl Pts',(-55.1531982367485,-104.727322009926,
174.763177441344));
#20379=CARTESIAN_POINT('Ctrl Pts',(-56.0026922166152,-104.542479047735,
173.89887555255));
#20380=CARTESIAN_POINT('Ctrl Pts',(-56.8521861964818,-104.357636085544,
173.034573663757));
#20381=CARTESIAN_POINT('Ctrl Pts',(-58.0576685335507,-104.134842386155,
173.034573714903));
#20382=CARTESIAN_POINT('Ctrl Pts',(-59.2631508706195,-103.912048686766,
173.034573766048));
#20383=CARTESIAN_POINT('Ctrl Pts',(-60.1126447785637,-103.727205732243,
173.898875727171));
#20384=CARTESIAN_POINT('Ctrl Pts',(-60.9621386865079,-103.54236277772,174.763177688294));
#20385=CARTESIAN_POINT('Ctrl Pts',(-60.952200572734,-103.449141018486,175.985485192554));
#20386=CARTESIAN_POINT('Ctrl Pts',(-60.9422624589602,-103.355919259252,
177.207792696815));
#20387=CARTESIAN_POINT('Ctrl Pts',(-60.0728923532595,-103.354318692132,
178.072094585608));
#20388=CARTESIAN_POINT('Ctrl Pts',(-59.2035222475588,-103.352718125012,
178.936396474401));
#20389=CARTESIAN_POINT('Ctrl Pts',(-57.9781637846559,-103.389068295091,
178.936396423256));
#20390=CARTESIAN_POINT('Ctrl Pts',(-56.7528053217531,-103.425418465169,
178.936396372111));
#20391=CARTESIAN_POINT('Ctrl Pts',(-55.8834352879748,-103.423817890381,
178.072094410988));
#20392=CARTESIAN_POINT('Ctrl Pts',(-55.0140652541966,-103.422217315594,
177.207792449865));
#20393=CARTESIAN_POINT('Ctrl Pts',(-55.0041272421364,-103.328995545517,
175.985484945604));
#20394=CARTESIAN_POINT('Ctrl Pts',(-54.9941892300763,-103.23577377544,174.763177441344));
#20395=CARTESIAN_POINT('Ctrl Pts',(-55.8436832099429,-103.050930813249,
173.89887555255));
#20396=CARTESIAN_POINT('Ctrl Pts',(-56.6931771898096,-102.866087851059,
173.034573663757));
#20397=CARTESIAN_POINT('Ctrl Pts',(-57.8986595268784,-102.64329415167,173.034573714903));
#20398=CARTESIAN_POINT('Ctrl Pts',(-59.1041418639473,-102.420500452281,
173.034573766048));
#20399=CARTESIAN_POINT('Ctrl Pts',(-59.9536357718915,-102.235657497757,
173.898875727171));
#20400=CARTESIAN_POINT('Ctrl Pts',(-60.8031296798357,-102.050814543234,
174.763177688294));
#20401=CARTESIAN_POINT('Ctrl Pts',(-60.7931915660618,-101.957592784,175.985485192554));
#20402=CARTESIAN_POINT('Ctrl Pts',(-60.783253452288,-101.864371024767,177.207792696815));
#20403=CARTESIAN_POINT('Ctrl Pts',(-59.9138833465873,-101.862770457647,
178.072094585608));
#20404=CARTESIAN_POINT('Ctrl Pts',(-59.0445132408866,-101.861169890527,
178.936396474401));
#20405=CARTESIAN_POINT('Ctrl Pts',(-57.8191547779837,-101.897520060605,
178.936396423256));
#20406=CARTESIAN_POINT('Ctrl Pts',(-56.5937963150808,-101.933870230683,
178.936396372111));
#20407=CARTESIAN_POINT('Ctrl Pts',(-55.7244262813026,-101.932269655896,
178.072094410988));
#20408=CARTESIAN_POINT('Ctrl Pts',(-54.8550562475244,-101.930669081108,
177.207792449865));
#20409=CARTESIAN_POINT('Ctrl Pts',(-54.8451182354642,-101.837447311031,
175.985484945604));
#20410=CARTESIAN_POINT('Ctrl Pts',(-54.8351802234041,-101.744225540954,
174.763177441344));
#20411=CARTESIAN_POINT('Ctrl Pts',(-55.6846742032707,-101.559382578764,
173.89887555255));
#20412=CARTESIAN_POINT('Ctrl Pts',(-56.5341681831374,-101.374539616573,
173.034573663757));
#20413=CARTESIAN_POINT('Ctrl Pts',(-57.7396505202062,-101.151745917184,
173.034573714903));
#20414=CARTESIAN_POINT('Ctrl Pts',(-58.9451328572751,-100.928952217795,
173.034573766048));
#20415=CARTESIAN_POINT('Ctrl Pts',(-59.7946267652193,-100.744109263272,
173.898875727171));
#20416=CARTESIAN_POINT('Ctrl Pts',(-60.6441206731635,-100.559266308748,
174.763177688294));
#20417=CARTESIAN_POINT('Ctrl Pts',(-60.6341825593896,-100.466044549515,
175.985485192554));
#20418=CARTESIAN_POINT('Ctrl Pts',(-60.6242444456157,-100.372822790281,
177.207792696815));
#20419=CARTESIAN_POINT('Ctrl Pts',(-59.754874339915,-100.371222223161,178.072094585608));
#20420=CARTESIAN_POINT('Ctrl Pts',(-58.8855042342143,-100.369621656041,
178.936396474401));
#20421=CARTESIAN_POINT('Ctrl Pts',(-57.6601457713115,-100.405971826119,
178.936396423256));
#20422=CARTESIAN_POINT('Ctrl Pts',(-56.4347873084086,-100.442321996198,
178.936396372111));
#20423=CARTESIAN_POINT('Ctrl Pts',(-55.5654172746304,-100.44072142141,178.072094410988));
#20424=CARTESIAN_POINT('Ctrl Pts',(-54.6960472408521,-100.439120846623,
177.207792449865));
#20425=CARTESIAN_POINT('Ctrl Pts',(-54.686109228792,-100.345899076546,175.985484945604));
#20426=CARTESIAN_POINT('Ctrl Pts',(-54.6761712167318,-100.252677306469,
174.763177441344));
#20427=CARTESIAN_POINT('Ctrl Pts',(-55.5256651965985,-100.067834344278,
173.89887555255));
#20428=CARTESIAN_POINT('Ctrl Pts',(-56.3751591764652,-99.8829913820874,
173.034573663757));
#20429=CARTESIAN_POINT('Ctrl Pts',(-57.580641513534,-99.6601976826983,173.034573714903));
#20430=CARTESIAN_POINT('Ctrl Pts',(-58.7861238506028,-99.4374039833093,
173.034573766048));
#20431=CARTESIAN_POINT('Ctrl Pts',(-59.635617758547,-99.252561028786,173.898875727171));
#20432=CARTESIAN_POINT('Ctrl Pts',(-60.4851116664912,-99.0677180742627,
174.763177688294));
#20433=CARTESIAN_POINT('Ctrl Pts',(-60.4751735527174,-98.9744963150291,
175.985485192554));
#20434=CARTESIAN_POINT('Ctrl Pts',(-60.4652354389435,-98.8812745557954,
177.207792696815));
#20435=CARTESIAN_POINT('Ctrl Pts',(-59.5958653332428,-98.8796739886754,
178.072094585608));
#20436=CARTESIAN_POINT('Ctrl Pts',(-58.7264952275421,-98.8780734215554,
178.936396474401));
#20437=CARTESIAN_POINT('Ctrl Pts',(-57.5011367646392,-98.9144235916337,
178.936396423256));
#20438=CARTESIAN_POINT('Ctrl Pts',(-56.2757783017364,-98.9507737617121,
178.936396372111));
#20439=CARTESIAN_POINT('Ctrl Pts',(-55.4064082679581,-98.9491731869247,
178.072094410988));
#20440=CARTESIAN_POINT('Ctrl Pts',(-61.0705815801248,-102.940927762808,
178.485485069079));
#20441=CARTESIAN_POINT('Ctrl Pts',(-60.9320093757681,-102.942642280685,
178.657813499464));
#20442=CARTESIAN_POINT('Ctrl Pts',(-60.7754659560919,-102.946768948967,
178.813912312176));
#20443=CARTESIAN_POINT('Ctrl Pts',(-59.6005562086583,-102.977740948934,
179.985485138407));
#20444=CARTESIAN_POINT('Ctrl Pts',(-57.9430994586544,-103.06015568322,179.985485069079));
#20445=CARTESIAN_POINT('Ctrl Pts',(-56.2856427086505,-103.142570417507,
179.985484999752));
#20446=CARTESIAN_POINT('Ctrl Pts',(-55.1107330587087,-103.17354240708,178.813912075476));
#20447=CARTESIAN_POINT('Ctrl Pts',(-53.935823408767,-103.204514396654,177.6423391512));
#20448=CARTESIAN_POINT('Ctrl Pts',(-53.9258854147871,-103.111292624649,
175.985484901707));
#20449=CARTESIAN_POINT('Ctrl Pts',(-53.9159474208072,-103.018070852645,
174.328630652215));
#20450=CARTESIAN_POINT('Ctrl Pts',(-55.0709810424069,-102.800655323367,
173.157057825983));
#20451=CARTESIAN_POINT('Ctrl Pts',(-56.2260146640065,-102.58323979409,171.985484999752));
#20452=CARTESIAN_POINT('Ctrl Pts',(-57.8635952881763,-102.314381530493,
171.985485069079));
#20453=CARTESIAN_POINT('Ctrl Pts',(-58.9165917619278,-102.141500391495,
171.985485113659));
#20454=CARTESIAN_POINT('Ctrl Pts',(-59.8287670060529,-101.979172801565,
172.515418850865));
#20455=CARTESIAN_POINT('Ctrl Pts',(-56.8733667677527,-112.709647553905,
178.072094410988));
#20456=CARTESIAN_POINT('Ctrl Pts',(-56.0039967339745,-112.708046979118,
177.207792449865));
#20457=CARTESIAN_POINT('Ctrl Pts',(-55.9940587219143,-112.614825209041,
175.985484945604));
#20458=CARTESIAN_POINT('Ctrl Pts',(-55.9841207098542,-112.521603438964,
174.763177441344));
#20459=CARTESIAN_POINT('Ctrl Pts',(-56.8336146897208,-112.336760476773,
173.89887555255));
#20460=CARTESIAN_POINT('Ctrl Pts',(-57.6831086695875,-112.151917514582,
173.034573663757));
#20461=CARTESIAN_POINT('Ctrl Pts',(-58.8885910066563,-111.929123815193,
173.034573714903));
#20462=CARTESIAN_POINT('Ctrl Pts',(-60.0940733437252,-111.706330115804,
173.034573766048));
#20463=CARTESIAN_POINT('Ctrl Pts',(-60.9435672516694,-111.521487161281,
173.898875727171));
#20464=CARTESIAN_POINT('Ctrl Pts',(-61.7930611596136,-111.336644206758,
174.763177688294));
#20465=CARTESIAN_POINT('Ctrl Pts',(-61.7831230458397,-111.243422447524,
175.985485192554));
#20466=CARTESIAN_POINT('Ctrl Pts',(-61.7731849320658,-111.15020068829,177.207792696815));
#20467=CARTESIAN_POINT('Ctrl Pts',(-60.9038148263651,-111.14860012117,178.072094585608));
#20468=CARTESIAN_POINT('Ctrl Pts',(-60.0344447206644,-111.14699955405,178.936396474401));
#20469=CARTESIAN_POINT('Ctrl Pts',(-58.8090862577616,-111.183349724129,
178.936396423256));
#20470=CARTESIAN_POINT('Ctrl Pts',(-57.5837277948587,-111.219699894207,
178.936396372111));
#20471=CARTESIAN_POINT('Ctrl Pts',(-56.7143577610805,-111.21809931942,178.072094410988));
#20472=CARTESIAN_POINT('Ctrl Pts',(-55.8449877273022,-111.216498744632,
177.207792449865));
#20473=CARTESIAN_POINT('Ctrl Pts',(-55.8350497152421,-111.123276974555,
175.985484945604));
#20474=CARTESIAN_POINT('Ctrl Pts',(-55.8251117031819,-111.030055204478,
174.763177441344));
#20475=CARTESIAN_POINT('Ctrl Pts',(-56.6746056830486,-110.845212242287,
173.89887555255));
#20476=CARTESIAN_POINT('Ctrl Pts',(-57.5240996629153,-110.660369280097,
173.034573663757));
#20477=CARTESIAN_POINT('Ctrl Pts',(-58.7295819999841,-110.437575580708,
173.034573714903));
#20478=CARTESIAN_POINT('Ctrl Pts',(-59.9350643370529,-110.214781881319,
173.034573766048));
#20479=CARTESIAN_POINT('Ctrl Pts',(-60.7845582449971,-110.029938926795,
173.898875727171));
#20480=CARTESIAN_POINT('Ctrl Pts',(-61.6340521529414,-109.845095972272,
174.763177688294));
#20481=CARTESIAN_POINT('Ctrl Pts',(-61.6241140391675,-109.751874213038,
175.985485192554));
#20482=CARTESIAN_POINT('Ctrl Pts',(-61.6141759253936,-109.658652453805,
177.207792696815));
#20483=CARTESIAN_POINT('Ctrl Pts',(-60.7448058196929,-109.657051886685,
178.072094585608));
#20484=CARTESIAN_POINT('Ctrl Pts',(-59.8754357139922,-109.655451319565,
178.936396474401));
#20485=CARTESIAN_POINT('Ctrl Pts',(-58.6500772510893,-109.691801489643,
178.936396423256));
#20486=CARTESIAN_POINT('Ctrl Pts',(-57.4247187881865,-109.728151659721,
178.936396372111));
#20487=CARTESIAN_POINT('Ctrl Pts',(-56.5553487544082,-109.726551084934,
178.072094410988));
#20488=CARTESIAN_POINT('Ctrl Pts',(-55.68597872063,-109.724950510147,177.207792449865));
#20489=CARTESIAN_POINT('Ctrl Pts',(-55.6760407085698,-109.63172874007,175.985484945604));
#20490=CARTESIAN_POINT('Ctrl Pts',(-55.6661026965097,-109.538506969993,
174.763177441344));
#20491=CARTESIAN_POINT('Ctrl Pts',(-56.5155966763764,-109.353664007802,
173.89887555255));
#20492=CARTESIAN_POINT('Ctrl Pts',(-57.365090656243,-109.168821045611,173.034573663757));
#20493=CARTESIAN_POINT('Ctrl Pts',(-58.5705729933119,-108.946027346222,
173.034573714903));
#20494=CARTESIAN_POINT('Ctrl Pts',(-59.7760553303807,-108.723233646833,
173.034573766048));
#20495=CARTESIAN_POINT('Ctrl Pts',(-60.6255492383249,-108.53839069231,173.898875727171));
#20496=CARTESIAN_POINT('Ctrl Pts',(-61.4750431462691,-108.353547737786,
174.763177688294));
#20497=CARTESIAN_POINT('Ctrl Pts',(-61.4651050324952,-108.260325978553,
175.985485192554));
#20498=CARTESIAN_POINT('Ctrl Pts',(-61.4551669187214,-108.167104219319,
177.207792696815));
#20499=CARTESIAN_POINT('Ctrl Pts',(-60.5857968130207,-108.165503652199,
178.072094585608));
#20500=CARTESIAN_POINT('Ctrl Pts',(-59.71642670732,-108.163903085079,178.936396474401));
#20501=CARTESIAN_POINT('Ctrl Pts',(-58.4910682444171,-108.200253255158,
178.936396423256));
#20502=CARTESIAN_POINT('Ctrl Pts',(-57.2657097815143,-108.236603425236,
178.936396372111));
#20503=CARTESIAN_POINT('Ctrl Pts',(-56.396339747736,-108.235002850448,178.072094410988));
#20504=CARTESIAN_POINT('Ctrl Pts',(-55.5269697139578,-108.233402275661,
177.207792449865));
#20505=CARTESIAN_POINT('Ctrl Pts',(-55.5170317018976,-108.140180505584,
175.985484945604));
#20506=CARTESIAN_POINT('Ctrl Pts',(-55.5070936898375,-108.046958735507,
174.763177441344));
#20507=CARTESIAN_POINT('Ctrl Pts',(-56.3565876697041,-107.862115773316,
173.89887555255));
#20508=CARTESIAN_POINT('Ctrl Pts',(-57.2060816495708,-107.677272811126,
173.034573663757));
#20509=CARTESIAN_POINT('Ctrl Pts',(-58.4115639866396,-107.454479111736,
173.034573714903));
#20510=CARTESIAN_POINT('Ctrl Pts',(-59.6170463237085,-107.231685412347,
173.034573766048));
#20511=CARTESIAN_POINT('Ctrl Pts',(-60.4665402316527,-107.046842457824,
173.898875727171));
#20512=CARTESIAN_POINT('Ctrl Pts',(-61.3160341395969,-106.861999503301,
174.763177688294));
#20513=CARTESIAN_POINT('Ctrl Pts',(-61.306096025823,-106.768777744067,175.985485192554));
#20514=CARTESIAN_POINT('Ctrl Pts',(-61.2961579120492,-106.675555984834,
177.207792696815));
#20515=CARTESIAN_POINT('Ctrl Pts',(-60.4267878063484,-106.673955417714,
178.072094585608));
#20516=CARTESIAN_POINT('Ctrl Pts',(-59.5574177006478,-106.672354850594,
178.936396474401));
#20517=CARTESIAN_POINT('Ctrl Pts',(-58.3320592377449,-106.708705020672,
178.936396423256));
#20518=CARTESIAN_POINT('Ctrl Pts',(-57.106700774842,-106.74505519075,178.936396372111));
#20519=CARTESIAN_POINT('Ctrl Pts',(-56.2373307410638,-106.743454615963,
178.072094410988));
#20520=CARTESIAN_POINT('Ctrl Pts',(-55.3679607072856,-106.741854041175,
177.207792449865));
#20521=CARTESIAN_POINT('Ctrl Pts',(-55.3580226952254,-106.648632271098,
175.985484945604));
#20522=CARTESIAN_POINT('Ctrl Pts',(-55.3480846831652,-106.555410501021,
174.763177441344));
#20523=CARTESIAN_POINT('Ctrl Pts',(-56.1975786630319,-106.370567538831,
173.89887555255));
#20524=CARTESIAN_POINT('Ctrl Pts',(-57.0470726428986,-106.18572457664,173.034573663757));
#20525=CARTESIAN_POINT('Ctrl Pts',(-58.2525549799674,-105.962930877251,
173.034573714903));
#20526=CARTESIAN_POINT('Ctrl Pts',(-59.4580373170363,-105.740137177862,
173.034573766048));
#20527=CARTESIAN_POINT('Ctrl Pts',(-60.3075312249805,-105.555294223339,
173.898875727171));
#20528=CARTESIAN_POINT('Ctrl Pts',(-61.1570251329247,-105.370451268815,
174.763177688294));
#20529=CARTESIAN_POINT('Ctrl Pts',(-61.1470870191508,-105.277229509582,
175.985485192554));
#20530=CARTESIAN_POINT('Ctrl Pts',(-61.1371489053769,-105.184007750348,
177.207792696815));
#20531=CARTESIAN_POINT('Ctrl Pts',(-60.2677787996762,-105.182407183228,
178.072094585608));
#20532=CARTESIAN_POINT('Ctrl Pts',(-59.3984086939755,-105.180806616108,
178.936396474401));
#20533=CARTESIAN_POINT('Ctrl Pts',(-58.1730502310727,-105.217156786186,
178.936396423256));
#20534=CARTESIAN_POINT('Ctrl Pts',(-56.9476917681698,-105.253506956265,
178.936396372111));
#20535=CARTESIAN_POINT('Ctrl Pts',(-56.0783217343916,-105.251906381477,
178.072094410988));
#20536=CARTESIAN_POINT('Ctrl Pts',(-55.2089517006133,-105.25030580669,177.207792449865));
#20537=CARTESIAN_POINT('Ctrl Pts',(-55.1990136885532,-105.157084036613,
175.985484945604));
#20538=CARTESIAN_POINT('Ctrl Pts',(-55.189075676493,-105.063862266536,174.763177441344));
#20539=CARTESIAN_POINT('Ctrl Pts',(-56.0385696563597,-104.879019304345,
173.89887555255));
#20540=CARTESIAN_POINT('Ctrl Pts',(-56.8880636362264,-104.694176342154,
173.034573663757));
#20541=CARTESIAN_POINT('Ctrl Pts',(-58.0935459732952,-104.471382642765,
173.034573714903));
#20542=CARTESIAN_POINT('Ctrl Pts',(-59.299028310364,-104.248588943376,173.034573766048));
#20543=CARTESIAN_POINT('Ctrl Pts',(-60.1485222183082,-104.063745988853,
173.898875727171));
#20544=CARTESIAN_POINT('Ctrl Pts',(-60.9980161262524,-103.87890303433,174.763177688294));
#20545=CARTESIAN_POINT('Ctrl Pts',(-60.9880780124786,-103.785681275096,
175.985485192554));
#20546=CARTESIAN_POINT('Ctrl Pts',(-60.9781398987047,-103.692459515862,
177.207792696815));
#20547=CARTESIAN_POINT('Ctrl Pts',(-60.108769793004,-103.690858948742,178.072094585608));
#20548=CARTESIAN_POINT('Ctrl Pts',(-59.2393996873033,-103.689258381622,
178.936396474401));
#20549=CARTESIAN_POINT('Ctrl Pts',(-58.0140412244004,-103.725608551701,
178.936396423256));
#20550=CARTESIAN_POINT('Ctrl Pts',(-56.7886827614976,-103.761958721779,
178.936396372111));
#20551=CARTESIAN_POINT('Ctrl Pts',(-55.9193127277193,-103.760358146992,
178.072094410988));
#20552=CARTESIAN_POINT('Ctrl Pts',(-55.0499426939411,-103.758757572204,
177.207792449865));
#20553=CARTESIAN_POINT('Ctrl Pts',(-55.0400046818809,-103.665535802127,
175.985484945604));
#20554=CARTESIAN_POINT('Ctrl Pts',(-55.0300666698208,-103.57231403205,174.763177441344));
#20555=CARTESIAN_POINT('Ctrl Pts',(-55.8795606496874,-103.387471069859,
173.89887555255));
#20556=CARTESIAN_POINT('Ctrl Pts',(-56.7290546295541,-103.202628107669,
173.034573663757));
#20557=CARTESIAN_POINT('Ctrl Pts',(-57.934536966623,-102.97983440828,173.034573714903));
#20558=CARTESIAN_POINT('Ctrl Pts',(-59.1400193036918,-102.757040708891,
173.034573766048));
#20559=CARTESIAN_POINT('Ctrl Pts',(-59.989513211636,-102.572197754367,173.898875727171));
#20560=CARTESIAN_POINT('Ctrl Pts',(-60.8390071195802,-102.387354799844,
174.763177688294));
#20561=CARTESIAN_POINT('Ctrl Pts',(-60.8290690058063,-102.29413304061,175.985485192554));
#20562=CARTESIAN_POINT('Ctrl Pts',(-60.8191308920325,-102.200911281377,
177.207792696815));
#20563=CARTESIAN_POINT('Ctrl Pts',(-59.9497607863318,-102.199310714257,
178.072094585608));
#20564=CARTESIAN_POINT('Ctrl Pts',(-59.0803906806311,-102.197710147137,
178.936396474401));
#20565=CARTESIAN_POINT('Ctrl Pts',(-57.8550322177282,-102.234060317215,
178.936396423256));
#20566=CARTESIAN_POINT('Ctrl Pts',(-56.6296737548253,-102.270410487293,
178.936396372111));
#20567=CARTESIAN_POINT('Ctrl Pts',(-55.7603037210471,-102.268809912506,
178.072094410988));
#20568=CARTESIAN_POINT('Ctrl Pts',(-54.8909336872689,-102.267209337719,
177.207792449865));
#20569=CARTESIAN_POINT('Ctrl Pts',(-54.8809956752087,-102.173987567642,
175.985484945604));
#20570=CARTESIAN_POINT('Ctrl Pts',(-54.8710576631486,-102.080765797565,
174.763177441344));
#20571=CARTESIAN_POINT('Ctrl Pts',(-55.7205516430152,-101.895922835374,
173.89887555255));
#20572=CARTESIAN_POINT('Ctrl Pts',(-56.5700456228819,-101.711079873183,
173.034573663757));
#20573=CARTESIAN_POINT('Ctrl Pts',(-57.7755279599507,-101.488286173794,
173.034573714903));
#20574=CARTESIAN_POINT('Ctrl Pts',(-58.9810102970196,-101.265492474405,
173.034573766048));
#20575=CARTESIAN_POINT('Ctrl Pts',(-59.8305042049638,-101.080649519882,
173.898875727171));
#20576=CARTESIAN_POINT('Ctrl Pts',(-60.679998112908,-100.895806565358,174.763177688294));
#20577=CARTESIAN_POINT('Ctrl Pts',(-60.6700599991341,-100.802584806125,
175.985485192554));
#20578=CARTESIAN_POINT('Ctrl Pts',(-60.6601218853602,-100.709363046891,
177.207792696815));
#20579=CARTESIAN_POINT('Ctrl Pts',(-59.7907517796595,-100.707762479771,
178.072094585608));
#20580=CARTESIAN_POINT('Ctrl Pts',(-58.9213816739588,-100.706161912651,
178.936396474401));
#20581=CARTESIAN_POINT('Ctrl Pts',(-57.696023211056,-100.742512082729,178.936396423256));
#20582=CARTESIAN_POINT('Ctrl Pts',(-56.4706647481531,-100.778862252808,
178.936396372111));
#20583=CARTESIAN_POINT('Ctrl Pts',(-55.6012947143749,-100.77726167802,178.072094410988));
#20584=CARTESIAN_POINT('Ctrl Pts',(-54.7319246805966,-100.775661103233,
177.207792449865));
#20585=CARTESIAN_POINT('Ctrl Pts',(-54.7219866685365,-100.682439333156,
175.985484945604));
#20586=CARTESIAN_POINT('Ctrl Pts',(-54.7120486564763,-100.589217563079,
174.763177441344));
#20587=CARTESIAN_POINT('Ctrl Pts',(-55.561542636343,-100.404374600888,173.89887555255));
#20588=CARTESIAN_POINT('Ctrl Pts',(-56.4110366162097,-100.219531638698,
173.034573663757));
#20589=CARTESIAN_POINT('Ctrl Pts',(-57.6165189532785,-99.9967379393085,
173.034573714903));
#20590=CARTESIAN_POINT('Ctrl Pts',(-58.8220012903473,-99.7739442399195,
173.034573766048));
#20591=CARTESIAN_POINT('Ctrl Pts',(-59.6714951982915,-99.5891012853962,
173.898875727171));
#20592=CARTESIAN_POINT('Ctrl Pts',(-60.5209891062358,-99.4042583308729,
174.763177688294));
#20593=CARTESIAN_POINT('Ctrl Pts',(-60.5110509924619,-99.3110365716392,
175.985485192554));
#20594=CARTESIAN_POINT('Ctrl Pts',(-60.501112878688,-99.2178148124055,177.207792696815));
#20595=CARTESIAN_POINT('Ctrl Pts',(-59.6317427729873,-99.2162142452855,
178.072094585608));
#20596=CARTESIAN_POINT('Ctrl Pts',(-58.7623726672866,-99.2146136781656,
178.936396474401));
#20597=CARTESIAN_POINT('Ctrl Pts',(-57.5370142043838,-99.2509638482439,
178.936396423256));
#20598=CARTESIAN_POINT('Ctrl Pts',(-56.3116557414809,-99.2873140183222,
178.936396372111));
#20599=CARTESIAN_POINT('Ctrl Pts',(-55.4422857077027,-99.2857134435348,
178.072094410988));
#20600=CARTESIAN_POINT('Ctrl Pts',(-54.5729156739244,-99.2841128687474,
177.207792449865));
#20601=CARTESIAN_POINT('Ctrl Pts',(-54.5629776618643,-99.1908910986704,
175.985484945604));
#20602=CARTESIAN_POINT('Ctrl Pts',(-54.5530396498041,-99.0976693285933,
174.763177441344));
#20603=CARTESIAN_POINT('Ctrl Pts',(-55.4025336296708,-98.9128263664026,
173.89887555255));
#20604=CARTESIAN_POINT('Ctrl Pts',(-56.2520276095374,-98.727983404212,173.034573663757));
#20605=CARTESIAN_POINT('Ctrl Pts',(-57.4575099466063,-98.5051897048229,
173.034573714903));
#20606=CARTESIAN_POINT('Ctrl Pts',(-58.6629922836751,-98.2823960054338,
173.034573766048));
#20607=CARTESIAN_POINT('Ctrl Pts',(-59.5124861916193,-98.0975530509106,
173.898875727171));
#20608=CARTESIAN_POINT('Ctrl Pts',(-60.3619800995635,-97.9127100963873,
174.763177688294));
#20609=CARTESIAN_POINT('Ctrl Pts',(-60.3520419857897,-97.8194883371536,
175.985485192554));
#20610=CARTESIAN_POINT('Ctrl Pts',(-60.3421038720158,-97.7262665779199,
177.207792696815));
#20611=CARTESIAN_POINT('Ctrl Pts',(-59.4727337663151,-97.7246660108,178.072094585608));
#20612=CARTESIAN_POINT('Ctrl Pts',(-58.6033636606144,-97.72306544368,178.936396474401));
#20613=CARTESIAN_POINT('Ctrl Pts',(-57.3780051977115,-97.7594156137583,
178.936396423256));
#20614=CARTESIAN_POINT('Ctrl Pts',(-56.1526467348087,-97.7957657838366,
178.936396372111));
#20615=CARTESIAN_POINT('Ctrl Pts',(-55.2832767010304,-97.7941652090492,
178.072094410988));
#20616=CARTESIAN_POINT('Ctrl Pts',(-56.1707931031902,-113.117197303651,
178.813912075476));
#20617=CARTESIAN_POINT('Ctrl Pts',(-54.9958834532485,-113.148169293224,
177.6423391512));
#20618=CARTESIAN_POINT('Ctrl Pts',(-54.9859454592686,-113.05494752122,175.985484901707));
#20619=CARTESIAN_POINT('Ctrl Pts',(-54.9760074652888,-112.961725749215,
174.328630652215));
#20620=CARTESIAN_POINT('Ctrl Pts',(-56.1310410868884,-112.744310219938,
173.157057825983));
#20621=CARTESIAN_POINT('Ctrl Pts',(-57.286074708488,-112.52689469066,171.985484999752));
#20622=CARTESIAN_POINT('Ctrl Pts',(-58.9236553326579,-112.258036427063,
171.985485069079));
#20623=CARTESIAN_POINT('Ctrl Pts',(-60.5612359568277,-111.989178163466,
171.985485138407));
#20624=CARTESIAN_POINT('Ctrl Pts',(-61.7162694809355,-111.771762644582,
173.157058062683));
#20625=CARTESIAN_POINT('Ctrl Pts',(-62.8713030050432,-111.554347125698,
174.328630986959));
#20626=CARTESIAN_POINT('Ctrl Pts',(-62.861364873189,-111.461125368392,175.985485236451));
#20627=CARTESIAN_POINT('Ctrl Pts',(-62.8514267413349,-111.367903611086,
177.642339485944));
#20628=CARTESIAN_POINT('Ctrl Pts',(-61.6765169939012,-111.398875611052,
178.813912312176));
#20629=CARTESIAN_POINT('Ctrl Pts',(-60.5016072464676,-111.429847611019,
179.985485138407));
#20630=CARTESIAN_POINT('Ctrl Pts',(-58.8441504964637,-111.512262345305,
179.985485069079));
#20631=CARTESIAN_POINT('Ctrl Pts',(-57.1866937464598,-111.594677079592,
179.985484999752));
#20632=CARTESIAN_POINT('Ctrl Pts',(-56.011784096518,-111.625649069165,178.813912075476));
#20633=CARTESIAN_POINT('Ctrl Pts',(-54.8368744465762,-111.656621058739,
177.6423391512));
#20634=CARTESIAN_POINT('Ctrl Pts',(-54.8269364525964,-111.563399286734,
175.985484901707));
#20635=CARTESIAN_POINT('Ctrl Pts',(-54.8169984586165,-111.47017751473,174.328630652215));
#20636=CARTESIAN_POINT('Ctrl Pts',(-55.9720320802161,-111.252761985452,
173.157057825983));
#20637=CARTESIAN_POINT('Ctrl Pts',(-57.1270657018158,-111.035346456175,
171.985484999752));
#20638=CARTESIAN_POINT('Ctrl Pts',(-58.7646463259856,-110.766488192578,
171.985485069079));
#20639=CARTESIAN_POINT('Ctrl Pts',(-60.4022269501555,-110.497629928981,
171.985485138407));
#20640=CARTESIAN_POINT('Ctrl Pts',(-61.5572604742632,-110.280214410097,
173.157058062683));
#20641=CARTESIAN_POINT('Ctrl Pts',(-62.712293998371,-110.062798891212,174.328630986959));
#20642=CARTESIAN_POINT('Ctrl Pts',(-62.7023558665168,-109.969577133906,
175.985485236451));
#20643=CARTESIAN_POINT('Ctrl Pts',(-62.6924177346626,-109.8763553766,177.642339485944));
#20644=CARTESIAN_POINT('Ctrl Pts',(-61.517507987229,-109.907327376567,178.813912312176));
#20645=CARTESIAN_POINT('Ctrl Pts',(-60.3425982397954,-109.938299376534,
179.985485138407));
#20646=CARTESIAN_POINT('Ctrl Pts',(-58.6851414897915,-110.02071411082,179.985485069079));
#20647=CARTESIAN_POINT('Ctrl Pts',(-57.0276847397876,-110.103128845106,
179.985484999752));
#20648=CARTESIAN_POINT('Ctrl Pts',(-55.8527750898458,-110.13410083468,178.813912075476));
#20649=CARTESIAN_POINT('Ctrl Pts',(-54.677865439904,-110.165072824253,177.6423391512));
#20650=CARTESIAN_POINT('Ctrl Pts',(-54.6679274459242,-110.071851052249,
175.985484901707));
#20651=CARTESIAN_POINT('Ctrl Pts',(-54.6579894519443,-109.978629280244,
174.328630652215));
#20652=CARTESIAN_POINT('Ctrl Pts',(-55.8130230735439,-109.761213750967,
173.157057825983));
#20653=CARTESIAN_POINT('Ctrl Pts',(-56.9680566951435,-109.543798221689,
171.985484999752));
#20654=CARTESIAN_POINT('Ctrl Pts',(-58.6056373193134,-109.274939958092,
171.985485069079));
#20655=CARTESIAN_POINT('Ctrl Pts',(-60.2432179434833,-109.006081694495,
171.985485138407));
#20656=CARTESIAN_POINT('Ctrl Pts',(-61.398251467591,-108.788666175611,173.157058062683));
#20657=CARTESIAN_POINT('Ctrl Pts',(-62.5532849916988,-108.571250656727,
174.328630986959));
#20658=CARTESIAN_POINT('Ctrl Pts',(-62.5433468598446,-108.478028899421,
175.985485236451));
#20659=CARTESIAN_POINT('Ctrl Pts',(-62.5334087279904,-108.384807142114,
177.642339485944));
#20660=CARTESIAN_POINT('Ctrl Pts',(-61.3584989805568,-108.415779142081,
178.813912312176));
#20661=CARTESIAN_POINT('Ctrl Pts',(-60.1835892331231,-108.446751142048,
179.985485138407));
#20662=CARTESIAN_POINT('Ctrl Pts',(-58.5261324831192,-108.529165876334,
179.985485069079));
#20663=CARTESIAN_POINT('Ctrl Pts',(-56.8686757331153,-108.611580610621,
179.985484999752));
#20664=CARTESIAN_POINT('Ctrl Pts',(-55.6937660831736,-108.642552600194,
178.813912075476));
#20665=CARTESIAN_POINT('Ctrl Pts',(-54.5188564332318,-108.673524589768,
177.6423391512));
#20666=CARTESIAN_POINT('Ctrl Pts',(-54.5089184392519,-108.580302817763,
175.985484901707));
#20667=CARTESIAN_POINT('Ctrl Pts',(-54.4989804452721,-108.487081045759,
174.328630652215));
#20668=CARTESIAN_POINT('Ctrl Pts',(-55.6540140668717,-108.269665516481,
173.157057825983));
#20669=CARTESIAN_POINT('Ctrl Pts',(-56.8090476884713,-108.052249987204,
171.985484999752));
#20670=CARTESIAN_POINT('Ctrl Pts',(-58.4466283126412,-107.783391723607,
171.985485069079));
#20671=CARTESIAN_POINT('Ctrl Pts',(-60.084208936811,-107.51453346001,171.985485138407));
#20672=CARTESIAN_POINT('Ctrl Pts',(-61.2392424609188,-107.297117941125,
173.157058062683));
#20673=CARTESIAN_POINT('Ctrl Pts',(-62.3942759850265,-107.079702422241,
174.328630986959));
#20674=CARTESIAN_POINT('Ctrl Pts',(-62.3843378531723,-106.986480664935,
175.985485236451));
#20675=CARTESIAN_POINT('Ctrl Pts',(-62.3743997213182,-106.893258907629,
177.642339485944));
#20676=CARTESIAN_POINT('Ctrl Pts',(-61.1994899738845,-106.924230907596,
178.813912312176));
#20677=CARTESIAN_POINT('Ctrl Pts',(-60.0245802264509,-106.955202907562,
179.985485138407));
#20678=CARTESIAN_POINT('Ctrl Pts',(-58.367123476447,-107.037617641849,179.985485069079));
#20679=CARTESIAN_POINT('Ctrl Pts',(-56.7096667264431,-107.120032376135,
179.985484999752));
#20680=CARTESIAN_POINT('Ctrl Pts',(-55.5347570765013,-107.151004365708,
178.813912075476));
#20681=CARTESIAN_POINT('Ctrl Pts',(-54.3598474265596,-107.181976355282,
177.6423391512));
#20682=CARTESIAN_POINT('Ctrl Pts',(-54.3499094325797,-107.088754583277,
175.985484901707));
#20683=CARTESIAN_POINT('Ctrl Pts',(-54.3399714385998,-106.995532811273,
174.328630652215));
#20684=CARTESIAN_POINT('Ctrl Pts',(-55.4950050601995,-106.778117281995,
173.157057825983));
#20685=CARTESIAN_POINT('Ctrl Pts',(-56.6500386817991,-106.560701752718,
171.985484999752));
#20686=CARTESIAN_POINT('Ctrl Pts',(-58.2876193059689,-106.291843489121,
171.985485069079));
#20687=CARTESIAN_POINT('Ctrl Pts',(-59.9251999301388,-106.022985225524,
171.985485138407));
#20688=CARTESIAN_POINT('Ctrl Pts',(-61.0802334542465,-105.80556970664,173.157058062683));
#20689=CARTESIAN_POINT('Ctrl Pts',(-62.2352669783543,-105.588154187756,
174.328630986959));
#20690=CARTESIAN_POINT('Ctrl Pts',(-62.2253288465001,-105.494932430449,
175.985485236451));
#20691=CARTESIAN_POINT('Ctrl Pts',(-62.2153907146459,-105.401710673143,
177.642339485944));
#20692=CARTESIAN_POINT('Ctrl Pts',(-61.0404809672123,-105.43268267311,178.813912312176));
#20693=CARTESIAN_POINT('Ctrl Pts',(-59.8655712197787,-105.463654673077,
179.985485138407));
#20694=CARTESIAN_POINT('Ctrl Pts',(-58.2081144697748,-105.546069407363,
179.985485069079));
#20695=CARTESIAN_POINT('Ctrl Pts',(-56.5506577197709,-105.628484141649,
179.985484999752));
#20696=CARTESIAN_POINT('Ctrl Pts',(-55.3757480698291,-105.659456131223,
178.813912075476));
#20697=CARTESIAN_POINT('Ctrl Pts',(-54.2008384198873,-105.690428120796,
177.6423391512));
#20698=CARTESIAN_POINT('Ctrl Pts',(-54.1909004259075,-105.597206348792,
175.985484901707));
#20699=CARTESIAN_POINT('Ctrl Pts',(-54.1809624319276,-105.503984576787,
174.328630652215));
#20700=CARTESIAN_POINT('Ctrl Pts',(-55.3359960535272,-105.28656904751,173.157057825983));
#20701=CARTESIAN_POINT('Ctrl Pts',(-56.4910296751268,-105.069153518232,
171.985484999752));
#20702=CARTESIAN_POINT('Ctrl Pts',(-58.1286102992967,-104.800295254635,
171.985485069079));
#20703=CARTESIAN_POINT('Ctrl Pts',(-59.7661909234666,-104.531436991038,
171.985485138407));
#20704=CARTESIAN_POINT('Ctrl Pts',(-60.9212244475743,-104.314021472154,
173.157058062683));
#20705=CARTESIAN_POINT('Ctrl Pts',(-62.0762579716821,-104.09660595327,174.328630986959));
#20706=CARTESIAN_POINT('Ctrl Pts',(-62.0663198398279,-104.003384195964,
175.985485236451));
#20707=CARTESIAN_POINT('Ctrl Pts',(-62.0563817079737,-103.910162438658,
177.642339485944));
#20708=CARTESIAN_POINT('Ctrl Pts',(-60.8814719605401,-103.941134438624,
178.813912312176));
#20709=CARTESIAN_POINT('Ctrl Pts',(-59.7065622131064,-103.972106438591,
179.985485138407));
#20710=CARTESIAN_POINT('Ctrl Pts',(-58.0491054631025,-104.054521172878,
179.985485069079));
#20711=CARTESIAN_POINT('Ctrl Pts',(-56.3916487130987,-104.136935907164,
179.985484999752));
#20712=CARTESIAN_POINT('Ctrl Pts',(-55.2167390631569,-104.167907896737,
178.813912075476));
#20713=CARTESIAN_POINT('Ctrl Pts',(-54.0418294132151,-104.198879886311,
177.6423391512));
#20714=CARTESIAN_POINT('Ctrl Pts',(-54.0318914192353,-104.105658114306,
175.985484901707));
#20715=CARTESIAN_POINT('Ctrl Pts',(-54.0219534252554,-104.012436342302,
174.328630652215));
#20716=CARTESIAN_POINT('Ctrl Pts',(-55.176987046855,-103.795020813024,173.157057825983));
#20717=CARTESIAN_POINT('Ctrl Pts',(-56.3320206684546,-103.577605283747,
171.985484999752));
#20718=CARTESIAN_POINT('Ctrl Pts',(-57.9696012926245,-103.30874702015,171.985485069079));
#20719=CARTESIAN_POINT('Ctrl Pts',(-59.6071819167943,-103.039888756553,
171.985485138407));
#20720=CARTESIAN_POINT('Ctrl Pts',(-60.7622154409021,-102.822473237669,
173.157058062683));
#20721=CARTESIAN_POINT('Ctrl Pts',(-61.9172489650099,-102.605057718784,
174.328630986959));
#20722=CARTESIAN_POINT('Ctrl Pts',(-61.9073108331557,-102.511835961478,
175.985485236451));
#20723=CARTESIAN_POINT('Ctrl Pts',(-61.8973727013015,-102.418614204172,
177.642339485944));
#20724=CARTESIAN_POINT('Ctrl Pts',(-60.7224629538678,-102.449586204139,
178.813912312176));
#20725=CARTESIAN_POINT('Ctrl Pts',(-59.5475532064342,-102.480558204106,
179.985485138407));
#20726=CARTESIAN_POINT('Ctrl Pts',(-57.8900964564303,-102.562972938392,
179.985485069079));
#20727=CARTESIAN_POINT('Ctrl Pts',(-56.2326397064264,-102.645387672678,
179.985484999752));
#20728=CARTESIAN_POINT('Ctrl Pts',(-55.0577300564847,-102.676359662252,
178.813912075476));
#20729=CARTESIAN_POINT('Ctrl Pts',(-53.8828204065429,-102.707331651825,
177.6423391512));
#20730=CARTESIAN_POINT('Ctrl Pts',(-53.872882412563,-102.614109879821,175.985484901707));
#20731=CARTESIAN_POINT('Ctrl Pts',(-53.8629444185832,-102.520888107816,
174.328630652215));
#20732=CARTESIAN_POINT('Ctrl Pts',(-55.0179780401828,-102.303472578539,
173.157057825983));
#20733=CARTESIAN_POINT('Ctrl Pts',(-56.1730116617824,-102.086057049261,
171.985484999752));
#20734=CARTESIAN_POINT('Ctrl Pts',(-57.8105922859523,-101.817198785664,
171.985485069079));
#20735=CARTESIAN_POINT('Ctrl Pts',(-59.4481729101221,-101.548340522067,
171.985485138407));
#20736=CARTESIAN_POINT('Ctrl Pts',(-60.6032064342299,-101.330925003183,
173.157058062683));
#20737=CARTESIAN_POINT('Ctrl Pts',(-61.7582399583376,-101.113509484299,
174.328630986959));
#20738=CARTESIAN_POINT('Ctrl Pts',(-61.7483018264834,-101.020287726993,
175.985485236451));
#20739=CARTESIAN_POINT('Ctrl Pts',(-61.7383636946293,-100.927065969686,
177.642339485944));
#20740=CARTESIAN_POINT('Ctrl Pts',(-60.5634539471956,-100.958037969653,
178.813912312176));
#20741=CARTESIAN_POINT('Ctrl Pts',(-59.388544199762,-100.98900996962,179.985485138407));
#20742=CARTESIAN_POINT('Ctrl Pts',(-57.7310874497581,-101.071424703906,
179.985485069079));
#20743=CARTESIAN_POINT('Ctrl Pts',(-56.0736306997542,-101.153839438193,
179.985484999752));
#20744=CARTESIAN_POINT('Ctrl Pts',(-54.8987210498124,-101.184811427766,
178.813912075476));
#20745=CARTESIAN_POINT('Ctrl Pts',(-53.7238113998707,-101.21578341734,177.6423391512));
#20746=CARTESIAN_POINT('Ctrl Pts',(-53.7138734058908,-101.122561645335,
175.985484901707));
#20747=CARTESIAN_POINT('Ctrl Pts',(-53.7039354119109,-101.029339873331,
174.328630652215));
#20748=CARTESIAN_POINT('Ctrl Pts',(-54.8589690335105,-100.811924344053,
173.157057825983));
#20749=CARTESIAN_POINT('Ctrl Pts',(-56.0140026551102,-100.594508814776,
171.985484999752));
#20750=CARTESIAN_POINT('Ctrl Pts',(-57.65158327928,-100.325650551179,171.985485069079));
#20751=CARTESIAN_POINT('Ctrl Pts',(-59.2891639034499,-100.056792287582,
171.985485138407));
#20752=CARTESIAN_POINT('Ctrl Pts',(-60.4441974275576,-99.8393767686974,
173.157058062683));
#20753=CARTESIAN_POINT('Ctrl Pts',(-61.5992309516654,-99.6219612498133,
174.328630986959));
#20754=CARTESIAN_POINT('Ctrl Pts',(-61.5892928198112,-99.528739492507,175.985485236451));
#20755=CARTESIAN_POINT('Ctrl Pts',(-61.579354687957,-99.4355177352008,177.642339485944));
#20756=CARTESIAN_POINT('Ctrl Pts',(-60.4044449405234,-99.4664897351676,
178.813912312176));
#20757=CARTESIAN_POINT('Ctrl Pts',(-59.2295351930898,-99.4974617351344,
179.985485138407));
#20758=CARTESIAN_POINT('Ctrl Pts',(-57.5720784430859,-99.5798764694207,
179.985485069079));
#20759=CARTESIAN_POINT('Ctrl Pts',(-55.914621693082,-99.662291203707,179.985484999752));
#20760=CARTESIAN_POINT('Ctrl Pts',(-54.7397120431402,-99.6932631932805,
178.813912075476));
#20761=CARTESIAN_POINT('Ctrl Pts',(-53.5648023931984,-99.724235182854,177.6423391512));
#20762=CARTESIAN_POINT('Ctrl Pts',(-53.5548643992186,-99.6310134108495,
175.985484901707));
#20763=CARTESIAN_POINT('Ctrl Pts',(-53.5449264052387,-99.5377916388449,
174.328630652215));
#20764=CARTESIAN_POINT('Ctrl Pts',(-54.6999600268383,-99.3203761095675,
173.157057825983));
#20765=CARTESIAN_POINT('Ctrl Pts',(-55.8549936484379,-99.10296058029,171.985484999752));
#20766=CARTESIAN_POINT('Ctrl Pts',(-57.4925742726078,-98.834102316693,171.985485069079));
#20767=CARTESIAN_POINT('Ctrl Pts',(-59.1301548967777,-98.565244053096,171.985485138407));
#20768=CARTESIAN_POINT('Ctrl Pts',(-60.2851884208854,-98.3478285342118,
173.157058062683));
#20769=CARTESIAN_POINT('Ctrl Pts',(-61.4402219449932,-98.1304130153276,
174.328630986959));
#20770=CARTESIAN_POINT('Ctrl Pts',(-61.430283813139,-98.0371912580215,175.985485236451));
#20771=CARTESIAN_POINT('Ctrl Pts',(-61.4203456812848,-97.9439695007152,
177.642339485944));
#20772=CARTESIAN_POINT('Ctrl Pts',(-60.2454359338512,-97.974941500682,178.813912312176));
#20773=CARTESIAN_POINT('Ctrl Pts',(-59.0705261864175,-98.0059135006488,
179.985485138407));
#20774=CARTESIAN_POINT('Ctrl Pts',(-57.4130694364136,-98.0883282349351,
179.985485069079));
#20775=CARTESIAN_POINT('Ctrl Pts',(-55.7556126864097,-98.1707429692214,
179.985484999752));
#20776=CARTESIAN_POINT('Ctrl Pts',(-54.580703036468,-98.2017149587949,178.813912075476));
#20777=CARTESIAN_POINT('Ctrl Pts',(-61.0175785779007,-102.443745017979,
178.485485069079));
#20778=CARTESIAN_POINT('Ctrl Pts',(-60.879006373544,-102.445459535857,178.657813499464));
#20779=CARTESIAN_POINT('Ctrl Pts',(-60.7224629538678,-102.449586204139,
178.813912312176));
#20780=CARTESIAN_POINT('Ctrl Pts',(-59.5475532064342,-102.480558204106,
179.985485138407));
#20781=CARTESIAN_POINT('Ctrl Pts',(-57.8900964564303,-102.562972938392,
179.985485069079));
#20782=CARTESIAN_POINT('Ctrl Pts',(-56.2326397064264,-102.645387672678,
179.985484999752));
#20783=CARTESIAN_POINT('Ctrl Pts',(-55.0577300564847,-102.676359662252,
178.813912075476));
#20784=CARTESIAN_POINT('Ctrl Pts',(-53.8828204798772,-102.707331649892,
177.642339224326));
#20785=CARTESIAN_POINT('Ctrl Pts',(-53.8728824136219,-102.614109889754,
175.985485078249));
#20786=CARTESIAN_POINT('Ctrl Pts',(-56.1707931031902,-113.117197303651,
178.813912075476));
#20787=CARTESIAN_POINT('Ctrl Pts',(-54.9958834532485,-113.148169293224,
177.6423391512));
#20788=CARTESIAN_POINT('Ctrl Pts',(-54.9859454592686,-113.05494752122,175.985484901707));
#20789=CARTESIAN_POINT('Ctrl Pts',(-54.9760074652888,-112.961725749215,
174.328630652215));
#20790=CARTESIAN_POINT('Ctrl Pts',(-56.1310410868884,-112.744310219938,
173.157057825983));
#20791=CARTESIAN_POINT('Ctrl Pts',(-57.286074708488,-112.52689469066,171.985484999752));
#20792=CARTESIAN_POINT('Ctrl Pts',(-58.9236553326578,-112.258036427063,
171.985485069079));
#20793=CARTESIAN_POINT('Ctrl Pts',(-60.5612359568277,-111.989178163466,
171.985485138407));
#20794=CARTESIAN_POINT('Ctrl Pts',(-61.7162694809355,-111.771762644582,
173.157058062683));
#20795=CARTESIAN_POINT('Ctrl Pts',(-62.8713030050432,-111.554347125698,
174.328630986959));
#20796=CARTESIAN_POINT('Ctrl Pts',(-62.861364873189,-111.461125368392,175.985485236451));
#20797=CARTESIAN_POINT('Ctrl Pts',(-62.8514267413349,-111.367903611086,
177.642339485944));
#20798=CARTESIAN_POINT('Ctrl Pts',(-61.6765169939012,-111.398875611052,
178.813912312176));
#20799=CARTESIAN_POINT('Ctrl Pts',(-60.5016072464676,-111.429847611019,
179.985485138407));
#20800=CARTESIAN_POINT('Ctrl Pts',(-58.8441504964637,-111.512262345305,
179.985485069079));
#20801=CARTESIAN_POINT('Ctrl Pts',(-57.1866937464598,-111.594677079592,
179.985484999752));
#20802=CARTESIAN_POINT('Ctrl Pts',(-56.011784096518,-111.625649069165,178.813912075476));
#20803=CARTESIAN_POINT('Ctrl Pts',(-54.8368744465763,-111.656621058739,
177.6423391512));
#20804=CARTESIAN_POINT('Ctrl Pts',(-54.8269364525964,-111.563399286734,
175.985484901707));
#20805=CARTESIAN_POINT('Ctrl Pts',(-54.8169984586165,-111.47017751473,174.328630652215));
#20806=CARTESIAN_POINT('Ctrl Pts',(-55.9720320802161,-111.252761985452,
173.157057825983));
#20807=CARTESIAN_POINT('Ctrl Pts',(-57.1270657018158,-111.035346456175,
171.985484999752));
#20808=CARTESIAN_POINT('Ctrl Pts',(-58.7646463259856,-110.766488192578,
171.985485069079));
#20809=CARTESIAN_POINT('Ctrl Pts',(-60.4022269501555,-110.497629928981,
171.985485138407));
#20810=CARTESIAN_POINT('Ctrl Pts',(-61.5572604742632,-110.280214410097,
173.157058062683));
#20811=CARTESIAN_POINT('Ctrl Pts',(-62.712293998371,-110.062798891212,174.328630986959));
#20812=CARTESIAN_POINT('Ctrl Pts',(-62.7023558665168,-109.969577133906,
175.985485236451));
#20813=CARTESIAN_POINT('Ctrl Pts',(-62.6924177346626,-109.8763553766,177.642339485944));
#20814=CARTESIAN_POINT('Ctrl Pts',(-61.517507987229,-109.907327376567,178.813912312176));
#20815=CARTESIAN_POINT('Ctrl Pts',(-60.3425982397954,-109.938299376534,
179.985485138407));
#20816=CARTESIAN_POINT('Ctrl Pts',(-58.6851414897915,-110.02071411082,179.985485069079));
#20817=CARTESIAN_POINT('Ctrl Pts',(-57.0276847397876,-110.103128845106,
179.985484999752));
#20818=CARTESIAN_POINT('Ctrl Pts',(-55.8527750898458,-110.13410083468,178.813912075476));
#20819=CARTESIAN_POINT('Ctrl Pts',(-54.677865439904,-110.165072824253,177.6423391512));
#20820=CARTESIAN_POINT('Ctrl Pts',(-54.6679274459242,-110.071851052249,
175.985484901707));
#20821=CARTESIAN_POINT('Ctrl Pts',(-54.6579894519443,-109.978629280244,
174.328630652215));
#20822=CARTESIAN_POINT('Ctrl Pts',(-55.8130230735439,-109.761213750967,
173.157057825983));
#20823=CARTESIAN_POINT('Ctrl Pts',(-56.9680566951435,-109.543798221689,
171.985484999752));
#20824=CARTESIAN_POINT('Ctrl Pts',(-58.6056373193134,-109.274939958092,
171.985485069079));
#20825=CARTESIAN_POINT('Ctrl Pts',(-60.2432179434833,-109.006081694495,
171.985485138407));
#20826=CARTESIAN_POINT('Ctrl Pts',(-61.398251467591,-108.788666175611,173.157058062683));
#20827=CARTESIAN_POINT('Ctrl Pts',(-62.5532849916988,-108.571250656727,
174.328630986959));
#20828=CARTESIAN_POINT('Ctrl Pts',(-62.5433468598446,-108.478028899421,
175.985485236451));
#20829=CARTESIAN_POINT('Ctrl Pts',(-62.5334087279904,-108.384807142114,
177.642339485944));
#20830=CARTESIAN_POINT('Ctrl Pts',(-61.3584989805568,-108.415779142081,
178.813912312176));
#20831=CARTESIAN_POINT('Ctrl Pts',(-60.1835892331231,-108.446751142048,
179.985485138407));
#20832=CARTESIAN_POINT('Ctrl Pts',(-58.5261324831192,-108.529165876334,
179.985485069079));
#20833=CARTESIAN_POINT('Ctrl Pts',(-56.8686757331153,-108.611580610621,
179.985484999752));
#20834=CARTESIAN_POINT('Ctrl Pts',(-55.6937660831736,-108.642552600194,
178.813912075476));
#20835=CARTESIAN_POINT('Ctrl Pts',(-54.5188564332318,-108.673524589768,
177.6423391512));
#20836=CARTESIAN_POINT('Ctrl Pts',(-54.5089184392519,-108.580302817763,
175.985484901707));
#20837=CARTESIAN_POINT('Ctrl Pts',(-54.4989804452721,-108.487081045759,
174.328630652215));
#20838=CARTESIAN_POINT('Ctrl Pts',(-55.6540140668717,-108.269665516481,
173.157057825983));
#20839=CARTESIAN_POINT('Ctrl Pts',(-56.8090476884713,-108.052249987204,
171.985484999752));
#20840=CARTESIAN_POINT('Ctrl Pts',(-58.4466283126412,-107.783391723607,
171.985485069079));
#20841=CARTESIAN_POINT('Ctrl Pts',(-60.084208936811,-107.51453346001,171.985485138407));
#20842=CARTESIAN_POINT('Ctrl Pts',(-61.2392424609188,-107.297117941125,
173.157058062683));
#20843=CARTESIAN_POINT('Ctrl Pts',(-62.3942759850265,-107.079702422241,
174.328630986959));
#20844=CARTESIAN_POINT('Ctrl Pts',(-62.3843378531723,-106.986480664935,
175.985485236451));
#20845=CARTESIAN_POINT('Ctrl Pts',(-62.3743997213182,-106.893258907629,
177.642339485944));
#20846=CARTESIAN_POINT('Ctrl Pts',(-61.1994899738845,-106.924230907596,
178.813912312176));
#20847=CARTESIAN_POINT('Ctrl Pts',(-60.0245802264509,-106.955202907562,
179.985485138407));
#20848=CARTESIAN_POINT('Ctrl Pts',(-58.367123476447,-107.037617641849,179.985485069079));
#20849=CARTESIAN_POINT('Ctrl Pts',(-56.7096667264431,-107.120032376135,
179.985484999752));
#20850=CARTESIAN_POINT('Ctrl Pts',(-55.5347570765013,-107.151004365708,
178.813912075476));
#20851=CARTESIAN_POINT('Ctrl Pts',(-54.3598474265596,-107.181976355282,
177.6423391512));
#20852=CARTESIAN_POINT('Ctrl Pts',(-54.3499094325797,-107.088754583277,
175.985484901707));
#20853=CARTESIAN_POINT('Ctrl Pts',(-54.3399714385998,-106.995532811273,
174.328630652215));
#20854=CARTESIAN_POINT('Ctrl Pts',(-55.4950050601995,-106.778117281995,
173.157057825983));
#20855=CARTESIAN_POINT('Ctrl Pts',(-56.6500386817991,-106.560701752718,
171.985484999752));
#20856=CARTESIAN_POINT('Ctrl Pts',(-58.2876193059689,-106.291843489121,
171.985485069079));
#20857=CARTESIAN_POINT('Ctrl Pts',(-59.9251999301388,-106.022985225524,
171.985485138407));
#20858=CARTESIAN_POINT('Ctrl Pts',(-61.0802334542465,-105.80556970664,173.157058062683));
#20859=CARTESIAN_POINT('Ctrl Pts',(-62.2352669783543,-105.588154187756,
174.328630986959));
#20860=CARTESIAN_POINT('Ctrl Pts',(-62.2253288465001,-105.494932430449,
175.985485236451));
#20861=CARTESIAN_POINT('Ctrl Pts',(-62.2153907146459,-105.401710673143,
177.642339485944));
#20862=CARTESIAN_POINT('Ctrl Pts',(-61.0404809672123,-105.43268267311,178.813912312176));
#20863=CARTESIAN_POINT('Ctrl Pts',(-59.8655712197787,-105.463654673077,
179.985485138407));
#20864=CARTESIAN_POINT('Ctrl Pts',(-58.2081144697748,-105.546069407363,
179.985485069079));
#20865=CARTESIAN_POINT('Ctrl Pts',(-56.5506577197709,-105.628484141649,
179.985484999752));
#20866=CARTESIAN_POINT('Ctrl Pts',(-55.3757480698291,-105.659456131223,
178.813912075476));
#20867=CARTESIAN_POINT('Ctrl Pts',(-54.2008384198873,-105.690428120796,
177.6423391512));
#20868=CARTESIAN_POINT('Ctrl Pts',(-54.1909004259075,-105.597206348792,
175.985484901707));
#20869=CARTESIAN_POINT('Ctrl Pts',(-54.1809624319276,-105.503984576787,
174.328630652215));
#20870=CARTESIAN_POINT('Ctrl Pts',(-55.3359960535272,-105.28656904751,173.157057825983));
#20871=CARTESIAN_POINT('Ctrl Pts',(-56.4910296751268,-105.069153518232,
171.985484999752));
#20872=CARTESIAN_POINT('Ctrl Pts',(-58.1286102992967,-104.800295254635,
171.985485069079));
#20873=CARTESIAN_POINT('Ctrl Pts',(-59.7661909234666,-104.531436991038,
171.985485138407));
#20874=CARTESIAN_POINT('Ctrl Pts',(-60.9212244475743,-104.314021472154,
173.157058062683));
#20875=CARTESIAN_POINT('Ctrl Pts',(-62.0762579716821,-104.09660595327,174.328630986959));
#20876=CARTESIAN_POINT('Ctrl Pts',(-62.0663198398279,-104.003384195964,
175.985485236451));
#20877=CARTESIAN_POINT('Ctrl Pts',(-62.0563817079737,-103.910162438658,
177.642339485944));
#20878=CARTESIAN_POINT('Ctrl Pts',(-60.8814719605401,-103.941134438624,
178.813912312176));
#20879=CARTESIAN_POINT('Ctrl Pts',(-59.7065622131064,-103.972106438591,
179.985485138407));
#20880=CARTESIAN_POINT('Ctrl Pts',(-58.0491054631025,-104.054521172878,
179.985485069079));
#20881=CARTESIAN_POINT('Ctrl Pts',(-56.3916487130987,-104.136935907164,
179.985484999752));
#20882=CARTESIAN_POINT('Ctrl Pts',(-55.2167390631569,-104.167907896737,
178.813912075476));
#20883=CARTESIAN_POINT('Ctrl Pts',(-54.0418294132151,-104.198879886311,
177.6423391512));
#20884=CARTESIAN_POINT('Ctrl Pts',(-54.0318914192353,-104.105658114306,
175.985484901707));
#20885=CARTESIAN_POINT('Ctrl Pts',(-54.0219534252554,-104.012436342302,
174.328630652215));
#20886=CARTESIAN_POINT('Ctrl Pts',(-55.176987046855,-103.795020813024,173.157057825983));
#20887=CARTESIAN_POINT('Ctrl Pts',(-56.3320206684546,-103.577605283747,
171.985484999752));
#20888=CARTESIAN_POINT('Ctrl Pts',(-57.9696012926245,-103.30874702015,171.985485069079));
#20889=CARTESIAN_POINT('Ctrl Pts',(-59.6071819167943,-103.039888756553,
171.985485138407));
#20890=CARTESIAN_POINT('Ctrl Pts',(-60.7622154409021,-102.822473237669,
173.157058062683));
#20891=CARTESIAN_POINT('Ctrl Pts',(-61.9172489650099,-102.605057718784,
174.328630986959));
#20892=CARTESIAN_POINT('Ctrl Pts',(-61.9073108331557,-102.511835961478,
175.985485236451));
#20893=CARTESIAN_POINT('Ctrl Pts',(-61.8973727013015,-102.418614204172,
177.642339485944));
#20894=CARTESIAN_POINT('Ctrl Pts',(-60.7224629538678,-102.449586204139,
178.813912312176));
#20895=CARTESIAN_POINT('Ctrl Pts',(-59.5475532064342,-102.480558204106,
179.985485138407));
#20896=CARTESIAN_POINT('Ctrl Pts',(-57.8900964564303,-102.562972938392,
179.985485069079));
#20897=CARTESIAN_POINT('Ctrl Pts',(-56.2326397064264,-102.645387672678,
179.985484999752));
#20898=CARTESIAN_POINT('Ctrl Pts',(-55.0577300564847,-102.676359662252,
178.813912075476));
#20899=CARTESIAN_POINT('Ctrl Pts',(-53.8828204065429,-102.707331651825,
177.6423391512));
#20900=CARTESIAN_POINT('Ctrl Pts',(-53.872882412563,-102.614109879821,175.985484901707));
#20901=CARTESIAN_POINT('Ctrl Pts',(-53.8629444185832,-102.520888107816,
174.328630652215));
#20902=CARTESIAN_POINT('Ctrl Pts',(-55.0179780401828,-102.303472578539,
173.157057825983));
#20903=CARTESIAN_POINT('Ctrl Pts',(-56.1730116617824,-102.086057049261,
171.985484999752));
#20904=CARTESIAN_POINT('Ctrl Pts',(-57.8105922859523,-101.817198785664,
171.985485069079));
#20905=CARTESIAN_POINT('Ctrl Pts',(-59.4481729101221,-101.548340522067,
171.985485138407));
#20906=CARTESIAN_POINT('Ctrl Pts',(-60.6032064342299,-101.330925003183,
173.157058062683));
#20907=CARTESIAN_POINT('Ctrl Pts',(-61.7582399583376,-101.113509484299,
174.328630986959));
#20908=CARTESIAN_POINT('Ctrl Pts',(-61.7483018264834,-101.020287726993,
175.985485236451));
#20909=CARTESIAN_POINT('Ctrl Pts',(-61.7383636946293,-100.927065969686,
177.642339485944));
#20910=CARTESIAN_POINT('Ctrl Pts',(-60.5634539471956,-100.958037969653,
178.813912312176));
#20911=CARTESIAN_POINT('Ctrl Pts',(-59.388544199762,-100.98900996962,179.985485138407));
#20912=CARTESIAN_POINT('Ctrl Pts',(-57.7310874497581,-101.071424703906,
179.985485069079));
#20913=CARTESIAN_POINT('Ctrl Pts',(-56.0736306997542,-101.153839438193,
179.985484999752));
#20914=CARTESIAN_POINT('Ctrl Pts',(-54.8987210498124,-101.184811427766,
178.813912075476));
#20915=CARTESIAN_POINT('Ctrl Pts',(-53.7238113998707,-101.21578341734,177.6423391512));
#20916=CARTESIAN_POINT('Ctrl Pts',(-53.7138734058908,-101.122561645335,
175.985484901707));
#20917=CARTESIAN_POINT('Ctrl Pts',(-53.7039354119109,-101.029339873331,
174.328630652215));
#20918=CARTESIAN_POINT('Ctrl Pts',(-54.8589690335105,-100.811924344053,
173.157057825983));
#20919=CARTESIAN_POINT('Ctrl Pts',(-56.0140026551102,-100.594508814776,
171.985484999752));
#20920=CARTESIAN_POINT('Ctrl Pts',(-57.65158327928,-100.325650551179,171.985485069079));
#20921=CARTESIAN_POINT('Ctrl Pts',(-59.2891639034499,-100.056792287582,
171.985485138407));
#20922=CARTESIAN_POINT('Ctrl Pts',(-60.4441974275576,-99.8393767686974,
173.157058062683));
#20923=CARTESIAN_POINT('Ctrl Pts',(-61.5992309516654,-99.6219612498133,
174.328630986959));
#20924=CARTESIAN_POINT('Ctrl Pts',(-61.5892928198112,-99.528739492507,175.985485236451));
#20925=CARTESIAN_POINT('Ctrl Pts',(-61.579354687957,-99.4355177352008,177.642339485944));
#20926=CARTESIAN_POINT('Ctrl Pts',(-60.4044449405234,-99.4664897351676,
178.813912312176));
#20927=CARTESIAN_POINT('Ctrl Pts',(-59.2295351930898,-99.4974617351344,
179.985485138407));
#20928=CARTESIAN_POINT('Ctrl Pts',(-57.5720784430859,-99.5798764694207,
179.985485069079));
#20929=CARTESIAN_POINT('Ctrl Pts',(-55.914621693082,-99.662291203707,179.985484999752));
#20930=CARTESIAN_POINT('Ctrl Pts',(-54.7397120431402,-99.6932631932805,
178.813912075476));
#20931=CARTESIAN_POINT('Ctrl Pts',(-53.5648023931984,-99.724235182854,177.6423391512));
#20932=CARTESIAN_POINT('Ctrl Pts',(-53.5548643992186,-99.6310134108495,
175.985484901707));
#20933=CARTESIAN_POINT('Ctrl Pts',(-53.5449264052387,-99.5377916388449,
174.328630652215));
#20934=CARTESIAN_POINT('Ctrl Pts',(-54.6999600268383,-99.3203761095675,
173.157057825983));
#20935=CARTESIAN_POINT('Ctrl Pts',(-55.8549936484379,-99.10296058029,171.985484999752));
#20936=CARTESIAN_POINT('Ctrl Pts',(-57.4925742726078,-98.834102316693,171.985485069079));
#20937=CARTESIAN_POINT('Ctrl Pts',(-59.1301548967777,-98.5652440530961,
171.985485138407));
#20938=CARTESIAN_POINT('Ctrl Pts',(-60.2851884208854,-98.3478285342118,
173.157058062683));
#20939=CARTESIAN_POINT('Ctrl Pts',(-61.4402219449932,-98.1304130153276,
174.328630986959));
#20940=CARTESIAN_POINT('Ctrl Pts',(-61.430283813139,-98.0371912580215,175.985485236451));
#20941=CARTESIAN_POINT('Ctrl Pts',(-61.4203456812848,-97.9439695007152,
177.642339485944));
#20942=CARTESIAN_POINT('Ctrl Pts',(-60.2454359338512,-97.974941500682,178.813912312176));
#20943=CARTESIAN_POINT('Ctrl Pts',(-59.0705261864175,-98.0059135006488,
179.985485138407));
#20944=CARTESIAN_POINT('Ctrl Pts',(-57.4130694364136,-98.0883282349351,
179.985485069079));
#20945=CARTESIAN_POINT('Ctrl Pts',(-55.7556126864097,-98.1707429692214,
179.985484999752));
#20946=CARTESIAN_POINT('Ctrl Pts',(-54.580703036468,-98.2017149587949,178.813912075476));
#20947=CARTESIAN_POINT('Ctrl Pts',(-56.181115489574,-113.283598570176,178.821287383467));
#20948=CARTESIAN_POINT('Ctrl Pts',(-55.0031681001975,-113.314894403068,
177.646659506339));
#20949=CARTESIAN_POINT('Ctrl Pts',(-54.9932301063974,-113.221672631044,
175.985484901271));
#20950=CARTESIAN_POINT('Ctrl Pts',(-54.9832921125973,-113.12845085902,174.324310296203));
#20951=CARTESIAN_POINT('Ctrl Pts',(-56.1413634738858,-112.910711486397,
173.149682517375));
#20952=CARTESIAN_POINT('Ctrl Pts',(-57.2994348351743,-112.692972113774,
171.975054738546));
#20953=CARTESIAN_POINT('Ctrl Pts',(-58.9413114718314,-112.423655866545,
171.975054808055));
#20954=CARTESIAN_POINT('Ctrl Pts',(-60.5831881084886,-112.154339619316,
171.975054877564));
#20955=CARTESIAN_POINT('Ctrl Pts',(-61.741259372031,-111.936600257113,173.149682754692));
#20956=CARTESIAN_POINT('Ctrl Pts',(-62.8993306355734,-111.71886089491,174.32431063182));
#20957=CARTESIAN_POINT('Ctrl Pts',(-62.8893925035395,-111.625639137623,
175.985485236888));
#20958=CARTESIAN_POINT('Ctrl Pts',(-62.8794543715055,-111.532417380336,
177.646659841956));
#20959=CARTESIAN_POINT('Ctrl Pts',(-61.701506884383,-111.563713223648,178.821287620784));
#20960=CARTESIAN_POINT('Ctrl Pts',(-60.5235593972605,-111.595009066961,
179.995915399612));
#20961=CARTESIAN_POINT('Ctrl Pts',(-58.8618066347693,-111.677881784879,
179.995915330104));
#20962=CARTESIAN_POINT('Ctrl Pts',(-57.2000538722782,-111.760754502798,
179.995915260595));
#20963=CARTESIAN_POINT('Ctrl Pts',(-56.0221064829017,-111.79205033569,178.821287383467));
#20964=CARTESIAN_POINT('Ctrl Pts',(-54.8441590935253,-111.823346168582,
177.646659506339));
#20965=CARTESIAN_POINT('Ctrl Pts',(-54.8342210997252,-111.730124396559,
175.985484901271));
#20966=CARTESIAN_POINT('Ctrl Pts',(-54.8242831059251,-111.636902624535,
174.324310296203));
#20967=CARTESIAN_POINT('Ctrl Pts',(-55.9823544672136,-111.419163251912,
173.149682517375));
#20968=CARTESIAN_POINT('Ctrl Pts',(-57.1404258285021,-111.201423879289,
171.975054738546));
#20969=CARTESIAN_POINT('Ctrl Pts',(-58.7823024651592,-110.932107632059,
171.975054808055));
#20970=CARTESIAN_POINT('Ctrl Pts',(-60.4241791018163,-110.66279138483,171.975054877564));
#20971=CARTESIAN_POINT('Ctrl Pts',(-61.5822503653587,-110.445052022627,
173.149682754692));
#20972=CARTESIAN_POINT('Ctrl Pts',(-62.7403216289012,-110.227312660424,
174.32431063182));
#20973=CARTESIAN_POINT('Ctrl Pts',(-62.7303834968672,-110.134090903137,
175.985485236888));
#20974=CARTESIAN_POINT('Ctrl Pts',(-62.7204453648333,-110.04086914585,177.646659841956));
#20975=CARTESIAN_POINT('Ctrl Pts',(-61.5424978777108,-110.072164989163,
178.821287620784));
#20976=CARTESIAN_POINT('Ctrl Pts',(-60.3645503905882,-110.103460832475,
179.995915399612));
#20977=CARTESIAN_POINT('Ctrl Pts',(-58.7027976280971,-110.186333550394,
179.995915330104));
#20978=CARTESIAN_POINT('Ctrl Pts',(-57.041044865606,-110.269206268313,179.995915260595));
#20979=CARTESIAN_POINT('Ctrl Pts',(-55.8630974762295,-110.300502101205,
178.821287383467));
#20980=CARTESIAN_POINT('Ctrl Pts',(-54.6851500868531,-110.331797934097,
177.646659506339));
#20981=CARTESIAN_POINT('Ctrl Pts',(-54.675212093053,-110.238576162073,175.985484901271));
#20982=CARTESIAN_POINT('Ctrl Pts',(-54.6652740992529,-110.145354390049,
174.324310296203));
#20983=CARTESIAN_POINT('Ctrl Pts',(-55.8233454605414,-109.927615017426,
173.149682517375));
#20984=CARTESIAN_POINT('Ctrl Pts',(-56.9814168218299,-109.709875644803,
171.975054738546));
#20985=CARTESIAN_POINT('Ctrl Pts',(-58.623293458487,-109.440559397574,171.975054808055));
#20986=CARTESIAN_POINT('Ctrl Pts',(-60.2651700951441,-109.171243150344,
171.975054877564));
#20987=CARTESIAN_POINT('Ctrl Pts',(-61.4232413586865,-108.953503788142,
173.149682754692));
#20988=CARTESIAN_POINT('Ctrl Pts',(-62.581312622229,-108.735764425939,174.32431063182));
#20989=CARTESIAN_POINT('Ctrl Pts',(-62.571374490195,-108.642542668652,175.985485236888));
#20990=CARTESIAN_POINT('Ctrl Pts',(-62.5614363581611,-108.549320911365,
177.646659841956));
#20991=CARTESIAN_POINT('Ctrl Pts',(-61.3834888710385,-108.580616754677,
178.821287620784));
#20992=CARTESIAN_POINT('Ctrl Pts',(-60.205541383916,-108.61191259799,179.995915399612));
#20993=CARTESIAN_POINT('Ctrl Pts',(-58.5437886214249,-108.694785315908,
179.995915330104));
#20994=CARTESIAN_POINT('Ctrl Pts',(-56.8820358589338,-108.777658033827,
179.995915260595));
#20995=CARTESIAN_POINT('Ctrl Pts',(-55.7040884695573,-108.808953866719,
178.821287383467));
#20996=CARTESIAN_POINT('Ctrl Pts',(-54.5261410801808,-108.840249699611,
177.646659506339));
#20997=CARTESIAN_POINT('Ctrl Pts',(-54.5162030863807,-108.747027927587,
175.985484901271));
#20998=CARTESIAN_POINT('Ctrl Pts',(-54.5062650925806,-108.653806155564,
174.324310296203));
#20999=CARTESIAN_POINT('Ctrl Pts',(-55.6643364538691,-108.436066782941,
173.149682517375));
#21000=CARTESIAN_POINT('Ctrl Pts',(-56.8224078151577,-108.218327410317,
171.975054738546));
#21001=CARTESIAN_POINT('Ctrl Pts',(-58.4642844518147,-107.949011163088,
171.975054808055));
#21002=CARTESIAN_POINT('Ctrl Pts',(-60.1061610884719,-107.679694915859,
171.975054877564));
#21003=CARTESIAN_POINT('Ctrl Pts',(-61.2642323520143,-107.461955553656,
173.149682754692));
#21004=CARTESIAN_POINT('Ctrl Pts',(-62.4223036155567,-107.244216191453,
174.32431063182));
#21005=CARTESIAN_POINT('Ctrl Pts',(-62.4123654835228,-107.150994434166,
175.985485236888));
#21006=CARTESIAN_POINT('Ctrl Pts',(-62.4024273514889,-107.057772676879,
177.646659841956));
#21007=CARTESIAN_POINT('Ctrl Pts',(-61.2244798643663,-107.089068520192,
178.821287620784));
#21008=CARTESIAN_POINT('Ctrl Pts',(-60.0465323772438,-107.120364363504,
179.995915399612));
#21009=CARTESIAN_POINT('Ctrl Pts',(-58.3847796147526,-107.203237081423,
179.995915330104));
#21010=CARTESIAN_POINT('Ctrl Pts',(-56.7230268522615,-107.286109799341,
179.995915260595));
#21011=CARTESIAN_POINT('Ctrl Pts',(-55.5450794628851,-107.317405632233,
178.821287383467));
#21012=CARTESIAN_POINT('Ctrl Pts',(-54.3671320735086,-107.348701465125,
177.646659506339));
#21013=CARTESIAN_POINT('Ctrl Pts',(-54.3571940797085,-107.255479693102,
175.985484901271));
#21014=CARTESIAN_POINT('Ctrl Pts',(-54.3472560859084,-107.162257921078,
174.324310296203));
#21015=CARTESIAN_POINT('Ctrl Pts',(-55.5053274471969,-106.944518548455,
173.149682517375));
#21016=CARTESIAN_POINT('Ctrl Pts',(-56.6633988084854,-106.726779175832,
171.975054738546));
#21017=CARTESIAN_POINT('Ctrl Pts',(-58.3052754451425,-106.457462928602,
171.975054808055));
#21018=CARTESIAN_POINT('Ctrl Pts',(-59.9471520817997,-106.188146681373,
171.975054877564));
#21019=CARTESIAN_POINT('Ctrl Pts',(-61.1052233453421,-105.97040731917,173.149682754692));
#21020=CARTESIAN_POINT('Ctrl Pts',(-62.2632946088845,-105.752667956968,
174.32431063182));
#21021=CARTESIAN_POINT('Ctrl Pts',(-62.2533564768505,-105.659446199681,
175.985485236888));
#21022=CARTESIAN_POINT('Ctrl Pts',(-62.2434183448166,-105.566224442394,
177.646659841956));
#21023=CARTESIAN_POINT('Ctrl Pts',(-61.0654708576941,-105.597520285706,
178.821287620784));
#21024=CARTESIAN_POINT('Ctrl Pts',(-59.8875233705716,-105.628816129018,
179.995915399612));
#21025=CARTESIAN_POINT('Ctrl Pts',(-58.2257706080804,-105.711688846937,
179.995915330104));
#21026=CARTESIAN_POINT('Ctrl Pts',(-56.5640178455893,-105.794561564856,
179.995915260595));
#21027=CARTESIAN_POINT('Ctrl Pts',(-55.3860704562128,-105.825857397748,
178.821287383467));
#21028=CARTESIAN_POINT('Ctrl Pts',(-54.2081230668364,-105.85715323064,177.646659506339));
#21029=CARTESIAN_POINT('Ctrl Pts',(-54.1981850730363,-105.763931458616,
175.985484901271));
#21030=CARTESIAN_POINT('Ctrl Pts',(-54.1882470792362,-105.670709686593,
174.324310296203));
#21031=CARTESIAN_POINT('Ctrl Pts',(-55.3463184405247,-105.452970313969,
173.149682517375));
#21032=CARTESIAN_POINT('Ctrl Pts',(-56.5043898018132,-105.235230941346,
171.975054738546));
#21033=CARTESIAN_POINT('Ctrl Pts',(-58.1462664384703,-104.965914694117,
171.975054808055));
#21034=CARTESIAN_POINT('Ctrl Pts',(-59.7881430751274,-104.696598446888,
171.975054877564));
#21035=CARTESIAN_POINT('Ctrl Pts',(-60.9462143386698,-104.478859084685,
173.149682754692));
#21036=CARTESIAN_POINT('Ctrl Pts',(-62.1042856022123,-104.261119722482,
174.32431063182));
#21037=CARTESIAN_POINT('Ctrl Pts',(-62.0943474701783,-104.167897965195,
175.985485236888));
#21038=CARTESIAN_POINT('Ctrl Pts',(-62.0844093381444,-104.074676207908,
177.646659841956));
#21039=CARTESIAN_POINT('Ctrl Pts',(-60.9064618510219,-104.10597205122,178.821287620784));
#21040=CARTESIAN_POINT('Ctrl Pts',(-59.7285143638993,-104.137267894533,
179.995915399612));
#21041=CARTESIAN_POINT('Ctrl Pts',(-58.0667616014082,-104.220140612451,
179.995915330104));
#21042=CARTESIAN_POINT('Ctrl Pts',(-56.4050088389171,-104.30301333037,179.995915260595));
#21043=CARTESIAN_POINT('Ctrl Pts',(-55.2270614495406,-104.334309163262,
178.821287383467));
#21044=CARTESIAN_POINT('Ctrl Pts',(-54.0491140601642,-104.365604996154,
177.646659506339));
#21045=CARTESIAN_POINT('Ctrl Pts',(-54.039176066364,-104.272383224131,175.985484901271));
#21046=CARTESIAN_POINT('Ctrl Pts',(-54.029238072564,-104.179161452107,174.324310296203));
#21047=CARTESIAN_POINT('Ctrl Pts',(-55.1873094338524,-103.961422079484,
173.149682517375));
#21048=CARTESIAN_POINT('Ctrl Pts',(-56.345380795141,-103.743682706861,171.975054738546));
#21049=CARTESIAN_POINT('Ctrl Pts',(-57.9872574317981,-103.474366459631,
171.975054808055));
#21050=CARTESIAN_POINT('Ctrl Pts',(-59.6291340684552,-103.205050212402,
171.975054877564));
#21051=CARTESIAN_POINT('Ctrl Pts',(-60.7872053319976,-102.987310850199,
173.149682754692));
#21052=CARTESIAN_POINT('Ctrl Pts',(-61.94527659554,-102.769571487996,174.32431063182));
#21053=CARTESIAN_POINT('Ctrl Pts',(-61.9353384635061,-102.676349730709,
175.985485236888));
#21054=CARTESIAN_POINT('Ctrl Pts',(-61.9254003314722,-102.583127973422,
177.646659841956));
#21055=CARTESIAN_POINT('Ctrl Pts',(-60.7474528443496,-102.614423816735,
178.821287620784));
#21056=CARTESIAN_POINT('Ctrl Pts',(-59.5695053572271,-102.645719660047,
179.995915399612));
#21057=CARTESIAN_POINT('Ctrl Pts',(-57.907752594736,-102.728592377966,179.995915330104));
#21058=CARTESIAN_POINT('Ctrl Pts',(-56.2459998322448,-102.811465095885,
179.995915260595));
#21059=CARTESIAN_POINT('Ctrl Pts',(-55.0680524428684,-102.842760928777,
178.821287383467));
#21060=CARTESIAN_POINT('Ctrl Pts',(-53.8901050534919,-102.874056761669,
177.646659506339));
#21061=CARTESIAN_POINT('Ctrl Pts',(-53.8801670596918,-102.780834989645,
175.985484901271));
#21062=CARTESIAN_POINT('Ctrl Pts',(-53.8702290658917,-102.687613217621,
174.324310296203));
#21063=CARTESIAN_POINT('Ctrl Pts',(-55.0283004271802,-102.469873844998,
173.149682517375));
#21064=CARTESIAN_POINT('Ctrl Pts',(-56.1863717884687,-102.252134472375,
171.975054738546));
#21065=CARTESIAN_POINT('Ctrl Pts',(-57.8282484251258,-101.982818225146,
171.975054808055));
#21066=CARTESIAN_POINT('Ctrl Pts',(-59.470125061783,-101.713501977916,171.975054877564));
#21067=CARTESIAN_POINT('Ctrl Pts',(-60.6281963253254,-101.495762615714,
173.149682754692));
#21068=CARTESIAN_POINT('Ctrl Pts',(-61.7862675888678,-101.278023253511,
174.32431063182));
#21069=CARTESIAN_POINT('Ctrl Pts',(-61.7763294568339,-101.184801496224,
175.985485236888));
#21070=CARTESIAN_POINT('Ctrl Pts',(-61.7663913247999,-101.091579738937,
177.646659841956));
#21071=CARTESIAN_POINT('Ctrl Pts',(-60.5884438376774,-101.122875582249,
178.821287620784));
#21072=CARTESIAN_POINT('Ctrl Pts',(-59.4104963505549,-101.154171425562,
179.995915399612));
#21073=CARTESIAN_POINT('Ctrl Pts',(-57.7487435880637,-101.23704414348,179.995915330104));
#21074=CARTESIAN_POINT('Ctrl Pts',(-56.0869908255726,-101.319916861399,
179.995915260595));
#21075=CARTESIAN_POINT('Ctrl Pts',(-54.9090434361961,-101.351212694291,
178.821287383467));
#21076=CARTESIAN_POINT('Ctrl Pts',(-53.7310960468197,-101.382508527183,
177.646659506339));
#21077=CARTESIAN_POINT('Ctrl Pts',(-53.7211580530196,-101.289286755159,
175.985484901271));
#21078=CARTESIAN_POINT('Ctrl Pts',(-53.7112200592195,-101.196064983136,
174.324310296203));
#21079=CARTESIAN_POINT('Ctrl Pts',(-54.869291420508,-100.978325610513,173.149682517375));
#21080=CARTESIAN_POINT('Ctrl Pts',(-56.0273627817965,-100.760586237889,
171.975054738546));
#21081=CARTESIAN_POINT('Ctrl Pts',(-57.6692394184536,-100.49126999066,171.975054808055));
#21082=CARTESIAN_POINT('Ctrl Pts',(-59.3111160551107,-100.221953743431,
171.975054877564));
#21083=CARTESIAN_POINT('Ctrl Pts',(-60.4691873186531,-100.004214381228,
173.149682754692));
#21084=CARTESIAN_POINT('Ctrl Pts',(-61.6272585821956,-99.7864750190253,
174.32431063182));
#21085=CARTESIAN_POINT('Ctrl Pts',(-61.6173204501616,-99.6932532617382,
175.985485236888));
#21086=CARTESIAN_POINT('Ctrl Pts',(-61.6073823181277,-99.6000315044512,
177.646659841956));
#21087=CARTESIAN_POINT('Ctrl Pts',(-60.4294348310052,-99.6313273477637,
178.821287620784));
#21088=CARTESIAN_POINT('Ctrl Pts',(-59.2514873438827,-99.6626231910761,
179.995915399612));
#21089=CARTESIAN_POINT('Ctrl Pts',(-57.5897345813915,-99.7454959089947,
179.995915330104));
#21090=CARTESIAN_POINT('Ctrl Pts',(-55.9279818189004,-99.8283686269133,
179.995915260595));
#21091=CARTESIAN_POINT('Ctrl Pts',(-54.7500344295239,-99.8596644598054,
178.821287383467));
#21092=CARTESIAN_POINT('Ctrl Pts',(-53.5720870401475,-99.8909602926975,
177.646659506339));
#21093=CARTESIAN_POINT('Ctrl Pts',(-53.5621490463474,-99.7977385206737,
175.985484901271));
#21094=CARTESIAN_POINT('Ctrl Pts',(-53.5522110525473,-99.7045167486501,
174.324310296203));
#21095=CARTESIAN_POINT('Ctrl Pts',(-54.7102824138358,-99.4867773760269,
173.149682517375));
#21096=CARTESIAN_POINT('Ctrl Pts',(-55.8683537751243,-99.2690380034038,
171.975054738546));
#21097=CARTESIAN_POINT('Ctrl Pts',(-57.5102304117814,-98.9997217561745,
171.975054808055));
#21098=CARTESIAN_POINT('Ctrl Pts',(-59.1521070484385,-98.7304055089452,
171.975054877564));
#21099=CARTESIAN_POINT('Ctrl Pts',(-60.3101783119809,-98.5126661467424,
173.149682754692));
#21100=CARTESIAN_POINT('Ctrl Pts',(-61.4682495755234,-98.2949267845397,
174.32431063182));
#21101=CARTESIAN_POINT('Ctrl Pts',(-61.4583114434894,-98.2017050272526,
175.985485236888));
#21102=CARTESIAN_POINT('Ctrl Pts',(-61.4483733114555,-98.1084832699656,
177.646659841956));
#21103=CARTESIAN_POINT('Ctrl Pts',(-60.2704258243329,-98.139779113278,178.821287620784));
#21104=CARTESIAN_POINT('Ctrl Pts',(-59.0924783372104,-98.1710749565905,
179.995915399612));
#21105=CARTESIAN_POINT('Ctrl Pts',(-57.4307255747193,-98.2539476745091,
179.995915330104));
#21106=CARTESIAN_POINT('Ctrl Pts',(-55.7689728122282,-98.3368203924277,
179.995915260595));
#21107=CARTESIAN_POINT('Ctrl Pts',(-54.5910254228517,-98.3681162253198,
178.821287383467));
#21108=CARTESIAN_POINT('Ctrl Pts',(-56.1988062143188,-113.449542435949,
178.821287383467));
#21109=CARTESIAN_POINT('Ctrl Pts',(-55.0208588249424,-113.480838268841,
177.646659506339));
#21110=CARTESIAN_POINT('Ctrl Pts',(-55.0109208311422,-113.387616496817,
175.985484901271));
#21111=CARTESIAN_POINT('Ctrl Pts',(-55.0009828373422,-113.294394724794,
174.324310296203));
#21112=CARTESIAN_POINT('Ctrl Pts',(-56.1590541986307,-113.07665535217,173.149682517375));
#21113=CARTESIAN_POINT('Ctrl Pts',(-57.3171255599192,-112.858915979547,
171.975054738546));
#21114=CARTESIAN_POINT('Ctrl Pts',(-58.9590021965763,-112.589599732318,
171.975054808055));
#21115=CARTESIAN_POINT('Ctrl Pts',(-60.6008788332334,-112.320283485089,
171.975054877564));
#21116=CARTESIAN_POINT('Ctrl Pts',(-61.7589500967758,-112.102544122886,
173.149682754692));
#21117=CARTESIAN_POINT('Ctrl Pts',(-62.9170213603182,-111.884804760683,
174.32431063182));
#21118=CARTESIAN_POINT('Ctrl Pts',(-62.9070832282843,-111.791583003396,
175.985485236888));
#21119=CARTESIAN_POINT('Ctrl Pts',(-62.8971450962504,-111.698361246109,
177.646659841956));
#21120=CARTESIAN_POINT('Ctrl Pts',(-61.7191976091278,-111.729657089422,
178.821287620784));
#21121=CARTESIAN_POINT('Ctrl Pts',(-60.5412501220053,-111.760952932734,
179.995915399612));
#21122=CARTESIAN_POINT('Ctrl Pts',(-58.8794973595142,-111.843825650653,
179.995915330104));
#21123=CARTESIAN_POINT('Ctrl Pts',(-57.217744597023,-111.926698368571,179.995915260595));
#21124=CARTESIAN_POINT('Ctrl Pts',(-56.0397972076466,-111.957994201463,
178.821287383467));
#21125=CARTESIAN_POINT('Ctrl Pts',(-54.8618498182701,-111.989290034355,
177.646659506339));
#21126=CARTESIAN_POINT('Ctrl Pts',(-54.85191182447,-111.896068262332,175.985484901271));
#21127=CARTESIAN_POINT('Ctrl Pts',(-54.8419738306699,-111.802846490308,
174.324310296203));
#21128=CARTESIAN_POINT('Ctrl Pts',(-56.0000451919584,-111.585107117685,
173.149682517375));
#21129=CARTESIAN_POINT('Ctrl Pts',(-57.158116553247,-111.367367745062,171.975054738546));
#21130=CARTESIAN_POINT('Ctrl Pts',(-58.799993189904,-111.098051497832,171.975054808055));
#21131=CARTESIAN_POINT('Ctrl Pts',(-60.4418698265612,-110.828735250603,
171.975054877564));
#21132=CARTESIAN_POINT('Ctrl Pts',(-61.5999410901036,-110.6109958884,173.149682754692));
#21133=CARTESIAN_POINT('Ctrl Pts',(-62.758012353646,-110.393256526198,174.32431063182));
#21134=CARTESIAN_POINT('Ctrl Pts',(-62.7480742216121,-110.30003476891,175.985485236888));
#21135=CARTESIAN_POINT('Ctrl Pts',(-62.7381360895782,-110.206813011623,
177.646659841956));
#21136=CARTESIAN_POINT('Ctrl Pts',(-61.5601886024556,-110.238108854936,
178.821287620784));
#21137=CARTESIAN_POINT('Ctrl Pts',(-60.3822411153331,-110.269404698248,
179.995915399612));
#21138=CARTESIAN_POINT('Ctrl Pts',(-58.7204883528419,-110.352277416167,
179.995915330104));
#21139=CARTESIAN_POINT('Ctrl Pts',(-57.0587355903508,-110.435150134086,
179.995915260595));
#21140=CARTESIAN_POINT('Ctrl Pts',(-55.8807882009743,-110.466445966978,
178.821287383467));
#21141=CARTESIAN_POINT('Ctrl Pts',(-54.7028408115979,-110.49774179987,177.646659506339));
#21142=CARTESIAN_POINT('Ctrl Pts',(-54.6929028177978,-110.404520027846,
175.985484901271));
#21143=CARTESIAN_POINT('Ctrl Pts',(-54.6829648239977,-110.311298255822,
174.324310296203));
#21144=CARTESIAN_POINT('Ctrl Pts',(-55.8410361852862,-110.093558883199,
173.149682517375));
#21145=CARTESIAN_POINT('Ctrl Pts',(-56.9991075465747,-109.875819510576,
171.975054738546));
#21146=CARTESIAN_POINT('Ctrl Pts',(-58.6409841832318,-109.606503263347,
171.975054808055));
#21147=CARTESIAN_POINT('Ctrl Pts',(-60.2828608198889,-109.337187016117,
171.975054877564));
#21148=CARTESIAN_POINT('Ctrl Pts',(-61.4409320834313,-109.119447653915,
173.149682754692));
#21149=CARTESIAN_POINT('Ctrl Pts',(-62.5990033469738,-108.901708291712,
174.32431063182));
#21150=CARTESIAN_POINT('Ctrl Pts',(-62.5890652149398,-108.808486534425,
175.985485236888));
#21151=CARTESIAN_POINT('Ctrl Pts',(-62.5791270829059,-108.715264777138,
177.646659841956));
#21152=CARTESIAN_POINT('Ctrl Pts',(-61.4011795957834,-108.74656062045,178.821287620784));
#21153=CARTESIAN_POINT('Ctrl Pts',(-60.2232321086609,-108.777856463763,
179.995915399612));
#21154=CARTESIAN_POINT('Ctrl Pts',(-58.5614793461697,-108.860729181681,
179.995915330104));
#21155=CARTESIAN_POINT('Ctrl Pts',(-56.8997265836786,-108.9436018996,179.995915260595));
#21156=CARTESIAN_POINT('Ctrl Pts',(-55.7217791943021,-108.974897732492,
178.821287383467));
#21157=CARTESIAN_POINT('Ctrl Pts',(-54.5438318049257,-109.006193565384,
177.646659506339));
#21158=CARTESIAN_POINT('Ctrl Pts',(-54.5338938111256,-108.91297179336,175.985484901271));
#21159=CARTESIAN_POINT('Ctrl Pts',(-54.5239558173255,-108.819750021337,
174.324310296203));
#21160=CARTESIAN_POINT('Ctrl Pts',(-55.682027178614,-108.602010648714,173.149682517375));
#21161=CARTESIAN_POINT('Ctrl Pts',(-56.8400985399025,-108.384271276091,
171.975054738546));
#21162=CARTESIAN_POINT('Ctrl Pts',(-58.4819751765596,-108.114955028861,
171.975054808055));
#21163=CARTESIAN_POINT('Ctrl Pts',(-60.1238518132167,-107.845638781632,
171.975054877564));
#21164=CARTESIAN_POINT('Ctrl Pts',(-61.2819230767591,-107.627899419429,
173.149682754692));
#21165=CARTESIAN_POINT('Ctrl Pts',(-62.4399943403016,-107.410160057226,
174.32431063182));
#21166=CARTESIAN_POINT('Ctrl Pts',(-62.4300562082676,-107.316938299939,
175.985485236888));
#21167=CARTESIAN_POINT('Ctrl Pts',(-62.4201180762337,-107.223716542652,
177.646659841956));
#21168=CARTESIAN_POINT('Ctrl Pts',(-61.2421705891111,-107.255012385965,
178.821287620784));
#21169=CARTESIAN_POINT('Ctrl Pts',(-60.0642231019886,-107.286308229277,
179.995915399612));
#21170=CARTESIAN_POINT('Ctrl Pts',(-58.4024703394975,-107.369180947196,
179.995915330104));
#21171=CARTESIAN_POINT('Ctrl Pts',(-56.7407175770064,-107.452053665114,
179.995915260595));
#21172=CARTESIAN_POINT('Ctrl Pts',(-55.5627701876299,-107.483349498006,
178.821287383467));
#21173=CARTESIAN_POINT('Ctrl Pts',(-54.3848227982534,-107.514645330899,
177.646659506339));
#21174=CARTESIAN_POINT('Ctrl Pts',(-54.3748848044533,-107.421423558875,
175.985484901271));
#21175=CARTESIAN_POINT('Ctrl Pts',(-54.3649468106533,-107.328201786851,
174.324310296203));
#21176=CARTESIAN_POINT('Ctrl Pts',(-55.5230181719417,-107.110462414228,
173.149682517375));
#21177=CARTESIAN_POINT('Ctrl Pts',(-56.6810895332303,-106.892723041605,
171.975054738546));
#21178=CARTESIAN_POINT('Ctrl Pts',(-58.3229661698874,-106.623406794376,
171.975054808055));
#21179=CARTESIAN_POINT('Ctrl Pts',(-59.9648428065445,-106.354090547146,
171.975054877564));
#21180=CARTESIAN_POINT('Ctrl Pts',(-61.1229140700869,-106.136351184943,
173.149682754692));
#21181=CARTESIAN_POINT('Ctrl Pts',(-62.2809853336293,-105.918611822741,
174.32431063182));
#21182=CARTESIAN_POINT('Ctrl Pts',(-62.2710472015954,-105.825390065454,
175.985485236888));
#21183=CARTESIAN_POINT('Ctrl Pts',(-62.2611090695615,-105.732168308167,
177.646659841956));
#21184=CARTESIAN_POINT('Ctrl Pts',(-61.0831615824389,-105.763464151479,
178.821287620784));
#21185=CARTESIAN_POINT('Ctrl Pts',(-59.9052140953164,-105.794759994792,
179.995915399612));
#21186=CARTESIAN_POINT('Ctrl Pts',(-58.2434613328252,-105.87763271271,179.995915330104));
#21187=CARTESIAN_POINT('Ctrl Pts',(-56.5817085703341,-105.960505430629,
179.995915260595));
#21188=CARTESIAN_POINT('Ctrl Pts',(-55.4037611809577,-105.991801263521,
178.821287383467));
#21189=CARTESIAN_POINT('Ctrl Pts',(-54.2258137915812,-106.023097096413,
177.646659506339));
#21190=CARTESIAN_POINT('Ctrl Pts',(-54.2158757977811,-105.929875324389,
175.985484901271));
#21191=CARTESIAN_POINT('Ctrl Pts',(-54.205937803981,-105.836653552366,174.324310296203));
#21192=CARTESIAN_POINT('Ctrl Pts',(-55.3640091652695,-105.618914179742,
173.149682517375));
#21193=CARTESIAN_POINT('Ctrl Pts',(-56.522080526558,-105.401174807119,171.975054738546));
#21194=CARTESIAN_POINT('Ctrl Pts',(-58.1639571632151,-105.13185855989,171.975054808055));
#21195=CARTESIAN_POINT('Ctrl Pts',(-59.8058337998722,-104.862542312661,
171.975054877564));
#21196=CARTESIAN_POINT('Ctrl Pts',(-60.9639050634147,-104.644802950458,
173.149682754692));
#21197=CARTESIAN_POINT('Ctrl Pts',(-62.1219763269571,-104.427063588255,
174.32431063182));
#21198=CARTESIAN_POINT('Ctrl Pts',(-62.1120381949232,-104.333841830968,
175.985485236888));
#21199=CARTESIAN_POINT('Ctrl Pts',(-62.1021000628892,-104.240620073681,
177.646659841956));
#21200=CARTESIAN_POINT('Ctrl Pts',(-60.9241525757667,-104.271915916993,
178.821287620784));
#21201=CARTESIAN_POINT('Ctrl Pts',(-59.7462050886442,-104.303211760306,
179.995915399612));
#21202=CARTESIAN_POINT('Ctrl Pts',(-58.084452326153,-104.386084478225,179.995915330104));
#21203=CARTESIAN_POINT('Ctrl Pts',(-56.4226995636619,-104.468957196143,
179.995915260595));
#21204=CARTESIAN_POINT('Ctrl Pts',(-55.2447521742854,-104.500253029035,
178.821287383467));
#21205=CARTESIAN_POINT('Ctrl Pts',(-54.066804784909,-104.531548861927,177.646659506339));
#21206=CARTESIAN_POINT('Ctrl Pts',(-54.0568667911089,-104.438327089904,
175.985484901271));
#21207=CARTESIAN_POINT('Ctrl Pts',(-54.0469287973088,-104.34510531788,174.324310296203));
#21208=CARTESIAN_POINT('Ctrl Pts',(-55.2050001585973,-104.127365945257,
173.149682517375));
#21209=CARTESIAN_POINT('Ctrl Pts',(-56.3630715198858,-103.909626572634,
171.975054738546));
#21210=CARTESIAN_POINT('Ctrl Pts',(-58.0049481565429,-103.640310325404,
171.975054808055));
#21211=CARTESIAN_POINT('Ctrl Pts',(-59.6468247932,-103.370994078175,171.975054877564));
#21212=CARTESIAN_POINT('Ctrl Pts',(-60.8048960567424,-103.153254715972,
173.149682754692));
#21213=CARTESIAN_POINT('Ctrl Pts',(-61.9629673202849,-102.93551535377,174.32431063182));
#21214=CARTESIAN_POINT('Ctrl Pts',(-61.9530291882509,-102.842293596483,
175.985485236888));
#21215=CARTESIAN_POINT('Ctrl Pts',(-61.943091056217,-102.749071839196,177.646659841956));
#21216=CARTESIAN_POINT('Ctrl Pts',(-60.7651435690945,-102.780367682508,
178.821287620784));
#21217=CARTESIAN_POINT('Ctrl Pts',(-59.587196081972,-102.81166352582,179.995915399612));
#21218=CARTESIAN_POINT('Ctrl Pts',(-57.9254433194808,-102.894536243739,
179.995915330104));
#21219=CARTESIAN_POINT('Ctrl Pts',(-56.2636905569897,-102.977408961658,
179.995915260595));
#21220=CARTESIAN_POINT('Ctrl Pts',(-55.0857431676132,-103.00870479455,178.821287383467));
#21221=CARTESIAN_POINT('Ctrl Pts',(-53.9077957782368,-103.040000627442,
177.646659506339));
#21222=CARTESIAN_POINT('Ctrl Pts',(-53.8978577844367,-102.946778855418,
175.985484901271));
#21223=CARTESIAN_POINT('Ctrl Pts',(-53.8879197906366,-102.853557083394,
174.324310296203));
#21224=CARTESIAN_POINT('Ctrl Pts',(-55.0459911519251,-102.635817710771,
173.149682517375));
#21225=CARTESIAN_POINT('Ctrl Pts',(-56.2040625132136,-102.418078338148,
171.975054738546));
#21226=CARTESIAN_POINT('Ctrl Pts',(-57.8459391498707,-102.148762090919,
171.975054808055));
#21227=CARTESIAN_POINT('Ctrl Pts',(-59.4878157865278,-101.879445843689,
171.975054877564));
#21228=CARTESIAN_POINT('Ctrl Pts',(-60.6458870500702,-101.661706481487,
173.149682754692));
#21229=CARTESIAN_POINT('Ctrl Pts',(-61.8039583136126,-101.443967119284,
174.32431063182));
#21230=CARTESIAN_POINT('Ctrl Pts',(-61.7940201815787,-101.350745361997,
175.985485236888));
#21231=CARTESIAN_POINT('Ctrl Pts',(-61.7840820495448,-101.25752360471,177.646659841956));
#21232=CARTESIAN_POINT('Ctrl Pts',(-60.6061345624222,-101.288819448022,
178.821287620784));
#21233=CARTESIAN_POINT('Ctrl Pts',(-59.4281870752997,-101.320115291335,
179.995915399612));
#21234=CARTESIAN_POINT('Ctrl Pts',(-57.7664343128086,-101.402988009253,
179.995915330104));
#21235=CARTESIAN_POINT('Ctrl Pts',(-56.1046815503175,-101.485860727172,
179.995915260595));
#21236=CARTESIAN_POINT('Ctrl Pts',(-54.926734160941,-101.517156560064,178.821287383467));
#21237=CARTESIAN_POINT('Ctrl Pts',(-53.7487867715645,-101.548452392956,
177.646659506339));
#21238=CARTESIAN_POINT('Ctrl Pts',(-53.7388487777644,-101.455230620932,
175.985484901271));
#21239=CARTESIAN_POINT('Ctrl Pts',(-53.7289107839643,-101.362008848909,
174.324310296203));
#21240=CARTESIAN_POINT('Ctrl Pts',(-54.8869821452528,-101.144269476286,
173.149682517375));
#21241=CARTESIAN_POINT('Ctrl Pts',(-56.0450535065414,-100.926530103662,
171.975054738546));
#21242=CARTESIAN_POINT('Ctrl Pts',(-57.6869301431984,-100.657213856433,
171.975054808055));
#21243=CARTESIAN_POINT('Ctrl Pts',(-59.3288067798556,-100.387897609204,
171.975054877564));
#21244=CARTESIAN_POINT('Ctrl Pts',(-60.486878043398,-100.170158247001,173.149682754692));
#21245=CARTESIAN_POINT('Ctrl Pts',(-61.6449493069404,-99.9524188847983,
174.32431063182));
#21246=CARTESIAN_POINT('Ctrl Pts',(-61.6350111749065,-99.8591971275113,
175.985485236888));
#21247=CARTESIAN_POINT('Ctrl Pts',(-61.6250730428726,-99.7659753702243,
177.646659841956));
#21248=CARTESIAN_POINT('Ctrl Pts',(-60.44712555575,-99.7972712135367,178.821287620784));
#21249=CARTESIAN_POINT('Ctrl Pts',(-59.2691780686275,-99.8285670568492,
179.995915399612));
#21250=CARTESIAN_POINT('Ctrl Pts',(-57.6074253061363,-99.9114397747677,
179.995915330104));
#21251=CARTESIAN_POINT('Ctrl Pts',(-55.9456725436452,-99.9943124926864,
179.995915260595));
#21252=CARTESIAN_POINT('Ctrl Pts',(-54.7677251542687,-100.025608325578,
178.821287383467));
#21253=CARTESIAN_POINT('Ctrl Pts',(-53.5897777648923,-100.05690415847,177.646659506339));
#21254=CARTESIAN_POINT('Ctrl Pts',(-53.5798397710922,-99.9636823864468,
175.985484901271));
#21255=CARTESIAN_POINT('Ctrl Pts',(-53.5699017772921,-99.8704606144232,
174.324310296203));
#21256=CARTESIAN_POINT('Ctrl Pts',(-54.7279731385806,-99.6527212418,173.149682517375));
#21257=CARTESIAN_POINT('Ctrl Pts',(-55.8860444998691,-99.4349818691769,
171.975054738546));
#21258=CARTESIAN_POINT('Ctrl Pts',(-57.5279211365262,-99.1656656219475,
171.975054808055));
#21259=CARTESIAN_POINT('Ctrl Pts',(-59.1697977731833,-98.8963493747183,
171.975054877564));
#21260=CARTESIAN_POINT('Ctrl Pts',(-60.3278690367257,-98.6786100125155,
173.149682754692));
#21261=CARTESIAN_POINT('Ctrl Pts',(-61.4859403002682,-98.4608706503128,
174.32431063182));
#21262=CARTESIAN_POINT('Ctrl Pts',(-61.4760021682342,-98.3676488930257,
175.985485236888));
#21263=CARTESIAN_POINT('Ctrl Pts',(-61.4660640362003,-98.2744271357387,
177.646659841956));
#21264=CARTESIAN_POINT('Ctrl Pts',(-60.2881165490778,-98.3057229790511,
178.821287620784));
#21265=CARTESIAN_POINT('Ctrl Pts',(-59.1101690619552,-98.3370188223636,
179.995915399612));
#21266=CARTESIAN_POINT('Ctrl Pts',(-57.4484162994641,-98.4198915402821,
179.995915330104));
#21267=CARTESIAN_POINT('Ctrl Pts',(-55.786663536973,-98.5027642582008,179.995915260595));
#21268=CARTESIAN_POINT('Ctrl Pts',(-54.6087161475965,-98.5340600910929,
178.821287383467));
#21269=CARTESIAN_POINT('Ctrl Pts',(-56.2237961054143,-113.614380048479,
178.813912075476));
#21270=CARTESIAN_POINT('Ctrl Pts',(-55.0488864554725,-113.645352038053,
177.6423391512));
#21271=CARTESIAN_POINT('Ctrl Pts',(-55.0389484614927,-113.552130266048,
175.985484901707));
#21272=CARTESIAN_POINT('Ctrl Pts',(-55.0290104675128,-113.458908494044,
174.328630652215));
#21273=CARTESIAN_POINT('Ctrl Pts',(-56.1840440891124,-113.241492964766,
173.157057825983));
#21274=CARTESIAN_POINT('Ctrl Pts',(-57.3390777107121,-113.024077435489,
171.985484999752));
#21275=CARTESIAN_POINT('Ctrl Pts',(-58.9766583348819,-112.755219171892,
171.985485069079));
#21276=CARTESIAN_POINT('Ctrl Pts',(-60.6142389590518,-112.486360908295,
171.985485138407));
#21277=CARTESIAN_POINT('Ctrl Pts',(-61.7692724831595,-112.268945389411,
173.157058062683));
#21278=CARTESIAN_POINT('Ctrl Pts',(-62.9243060072673,-112.051529870527,
174.328630986959));
#21279=CARTESIAN_POINT('Ctrl Pts',(-62.9143678754131,-111.95830811322,175.985485236451));
#21280=CARTESIAN_POINT('Ctrl Pts',(-62.9044297435589,-111.865086355914,
177.642339485944));
#21281=CARTESIAN_POINT('Ctrl Pts',(-61.7295199961253,-111.896058355881,
178.813912312176));
#21282=CARTESIAN_POINT('Ctrl Pts',(-60.5546102486917,-111.927030355848,
179.985485138407));
#21283=CARTESIAN_POINT('Ctrl Pts',(-58.8971534986878,-112.009445090134,
179.985485069079));
#21284=CARTESIAN_POINT('Ctrl Pts',(-57.2396967486839,-112.09185982442,179.985484999752));
#21285=CARTESIAN_POINT('Ctrl Pts',(-56.0647870987421,-112.122831813994,
178.813912075476));
#21286=CARTESIAN_POINT('Ctrl Pts',(-54.8898774488003,-112.153803803567,
177.6423391512));
#21287=CARTESIAN_POINT('Ctrl Pts',(-54.8799394548205,-112.060582031563,
175.985484901707));
#21288=CARTESIAN_POINT('Ctrl Pts',(-54.8700014608406,-111.967360259558,
174.328630652215));
#21289=CARTESIAN_POINT('Ctrl Pts',(-56.0250350824402,-111.749944730281,
173.157057825983));
#21290=CARTESIAN_POINT('Ctrl Pts',(-57.1800687040398,-111.532529201003,
171.985484999752));
#21291=CARTESIAN_POINT('Ctrl Pts',(-58.8176493282097,-111.263670937406,
171.985485069079));
#21292=CARTESIAN_POINT('Ctrl Pts',(-60.4552299523796,-110.994812673809,
171.985485138407));
#21293=CARTESIAN_POINT('Ctrl Pts',(-61.6102634764873,-110.777397154925,
173.157058062683));
#21294=CARTESIAN_POINT('Ctrl Pts',(-62.7652970005951,-110.559981636041,
174.328630986959));
#21295=CARTESIAN_POINT('Ctrl Pts',(-62.7553588687409,-110.466759878735,
175.985485236451));
#21296=CARTESIAN_POINT('Ctrl Pts',(-62.7454207368867,-110.373538121429,
177.642339485944));
#21297=CARTESIAN_POINT('Ctrl Pts',(-61.5705109894531,-110.404510121395,
178.813912312176));
#21298=CARTESIAN_POINT('Ctrl Pts',(-60.3956012420194,-110.435482121362,
179.985485138407));
#21299=CARTESIAN_POINT('Ctrl Pts',(-58.7381444920155,-110.517896855648,
179.985485069079));
#21300=CARTESIAN_POINT('Ctrl Pts',(-57.0806877420116,-110.600311589935,
179.985484999752));
#21301=CARTESIAN_POINT('Ctrl Pts',(-55.9057780920699,-110.631283579508,
178.813912075476));
#21302=CARTESIAN_POINT('Ctrl Pts',(-54.7308684421281,-110.662255569082,
177.6423391512));
#21303=CARTESIAN_POINT('Ctrl Pts',(-54.7209304481482,-110.569033797077,
175.985484901707));
#21304=CARTESIAN_POINT('Ctrl Pts',(-54.7109924541684,-110.475812025073,
174.328630652215));
#21305=CARTESIAN_POINT('Ctrl Pts',(-55.866026075768,-110.258396495795,173.157057825983));
#21306=CARTESIAN_POINT('Ctrl Pts',(-57.0210596973676,-110.040980966518,
171.985484999752));
#21307=CARTESIAN_POINT('Ctrl Pts',(-58.6586403215375,-109.772122702921,
171.985485069079));
#21308=CARTESIAN_POINT('Ctrl Pts',(-60.2962209457073,-109.503264439324,
171.985485138407));
#21309=CARTESIAN_POINT('Ctrl Pts',(-61.4512544698151,-109.28584892044,173.157058062683));
#21310=CARTESIAN_POINT('Ctrl Pts',(-62.6062879939228,-109.068433401555,
174.328630986959));
#21311=CARTESIAN_POINT('Ctrl Pts',(-62.5963498620687,-108.975211644249,
175.985485236451));
#21312=CARTESIAN_POINT('Ctrl Pts',(-62.5864117302145,-108.881989886943,
177.642339485944));
#21313=CARTESIAN_POINT('Ctrl Pts',(-61.4115019827808,-108.91296188691,178.813912312176));
#21314=CARTESIAN_POINT('Ctrl Pts',(-60.2365922353472,-108.943933886877,
179.985485138407));
#21315=CARTESIAN_POINT('Ctrl Pts',(-58.5791354853433,-109.026348621163,
179.985485069079));
#21316=CARTESIAN_POINT('Ctrl Pts',(-56.9216787353394,-109.108763355449,
179.985484999752));
#21317=CARTESIAN_POINT('Ctrl Pts',(-55.7467690853976,-109.139735345023,
178.813912075476));
#21318=CARTESIAN_POINT('Ctrl Pts',(-54.5718594354559,-109.170707334596,
177.6423391512));
#21319=CARTESIAN_POINT('Ctrl Pts',(-54.561921441476,-109.077485562592,175.985484901707));
#21320=CARTESIAN_POINT('Ctrl Pts',(-54.5519834474962,-108.984263790587,
174.328630652215));
#21321=CARTESIAN_POINT('Ctrl Pts',(-55.7070170690958,-108.76684826131,173.157057825983));
#21322=CARTESIAN_POINT('Ctrl Pts',(-56.8620506906954,-108.549432732032,
171.985484999752));
#21323=CARTESIAN_POINT('Ctrl Pts',(-58.4996313148652,-108.280574468435,
171.985485069079));
#21324=CARTESIAN_POINT('Ctrl Pts',(-60.1372119390351,-108.011716204838,
171.985485138407));
#21325=CARTESIAN_POINT('Ctrl Pts',(-61.2922454631428,-107.794300685954,
173.157058062683));
#21326=CARTESIAN_POINT('Ctrl Pts',(-62.4472789872506,-107.57688516707,174.328630986959));
#21327=CARTESIAN_POINT('Ctrl Pts',(-62.4373408553964,-107.483663409764,
175.985485236451));
#21328=CARTESIAN_POINT('Ctrl Pts',(-62.4274027235423,-107.390441652457,
177.642339485944));
#21329=CARTESIAN_POINT('Ctrl Pts',(-61.2524929761086,-107.421413652424,
178.813912312176));
#21330=CARTESIAN_POINT('Ctrl Pts',(-60.077583228675,-107.452385652391,179.985485138407));
#21331=CARTESIAN_POINT('Ctrl Pts',(-58.4201264786711,-107.534800386677,
179.985485069079));
#21332=CARTESIAN_POINT('Ctrl Pts',(-56.7626697286672,-107.617215120964,
179.985484999752));
#21333=CARTESIAN_POINT('Ctrl Pts',(-55.5877600787254,-107.648187110537,
178.813912075476));
#21334=CARTESIAN_POINT('Ctrl Pts',(-54.4128504287836,-107.67915910011,177.6423391512));
#21335=CARTESIAN_POINT('Ctrl Pts',(-54.4029124348038,-107.585937328106,
175.985484901707));
#21336=CARTESIAN_POINT('Ctrl Pts',(-54.3929744408239,-107.492715556102,
174.328630652215));
#21337=CARTESIAN_POINT('Ctrl Pts',(-55.5480080624235,-107.275300026824,
173.157057825983));
#21338=CARTESIAN_POINT('Ctrl Pts',(-56.7030416840231,-107.057884497547,
171.985484999752));
#21339=CARTESIAN_POINT('Ctrl Pts',(-58.340622308193,-106.78902623395,171.985485069079));
#21340=CARTESIAN_POINT('Ctrl Pts',(-59.9782029323629,-106.520167970353,
171.985485138407));
#21341=CARTESIAN_POINT('Ctrl Pts',(-61.1332364564706,-106.302752451468,
173.157058062683));
#21342=CARTESIAN_POINT('Ctrl Pts',(-62.2882699805784,-106.085336932584,
174.328630986959));
#21343=CARTESIAN_POINT('Ctrl Pts',(-62.2783318487242,-105.992115175278,
175.985485236451));
#21344=CARTESIAN_POINT('Ctrl Pts',(-62.26839371687,-105.898893417972,177.642339485944));
#21345=CARTESIAN_POINT('Ctrl Pts',(-61.0934839694364,-105.929865417939,
178.813912312176));
#21346=CARTESIAN_POINT('Ctrl Pts',(-59.9185742220028,-105.960837417905,
179.985485138407));
#21347=CARTESIAN_POINT('Ctrl Pts',(-58.2611174719989,-106.043252152192,
179.985485069079));
#21348=CARTESIAN_POINT('Ctrl Pts',(-56.603660721995,-106.125666886478,179.985484999752));
#21349=CARTESIAN_POINT('Ctrl Pts',(-55.4287510720532,-106.156638876051,
178.813912075476));
#21350=CARTESIAN_POINT('Ctrl Pts',(-54.2538414221114,-106.187610865625,
177.6423391512));
#21351=CARTESIAN_POINT('Ctrl Pts',(-54.2439034281315,-106.09438909362,175.985484901707));
#21352=CARTESIAN_POINT('Ctrl Pts',(-54.2339654341517,-106.001167321616,
174.328630652215));
#21353=CARTESIAN_POINT('Ctrl Pts',(-55.3889990557513,-105.783751792338,
173.157057825983));
#21354=CARTESIAN_POINT('Ctrl Pts',(-56.5440326773509,-105.566336263061,
171.985484999752));
#21355=CARTESIAN_POINT('Ctrl Pts',(-58.1816133015208,-105.297477999464,
171.985485069079));
#21356=CARTESIAN_POINT('Ctrl Pts',(-59.8191939256906,-105.028619735867,
171.985485138407));
#21357=CARTESIAN_POINT('Ctrl Pts',(-60.9742274497984,-104.811204216983,
173.157058062683));
#21358=CARTESIAN_POINT('Ctrl Pts',(-62.1292609739061,-104.593788698099,
174.328630986959));
#21359=CARTESIAN_POINT('Ctrl Pts',(-62.119322842052,-104.500566940792,175.985485236451));
#21360=CARTESIAN_POINT('Ctrl Pts',(-62.1093847101978,-104.407345183486,
177.642339485944));
#21361=CARTESIAN_POINT('Ctrl Pts',(-60.9344749627642,-104.438317183453,
178.813912312176));
#21362=CARTESIAN_POINT('Ctrl Pts',(-59.7595652153305,-104.46928918342,179.985485138407));
#21363=CARTESIAN_POINT('Ctrl Pts',(-58.1021084653266,-104.551703917706,
179.985485069079));
#21364=CARTESIAN_POINT('Ctrl Pts',(-56.4446517153227,-104.634118651992,
179.985484999752));
#21365=CARTESIAN_POINT('Ctrl Pts',(-55.269742065381,-104.665090641566,178.813912075476));
#21366=CARTESIAN_POINT('Ctrl Pts',(-54.0948324154392,-104.696062631139,
177.6423391512));
#21367=CARTESIAN_POINT('Ctrl Pts',(-54.0848944214593,-104.602840859135,
175.985484901707));
#21368=CARTESIAN_POINT('Ctrl Pts',(-54.0749564274795,-104.50961908713,174.328630652215));
#21369=CARTESIAN_POINT('Ctrl Pts',(-55.2299900490791,-104.292203557853,
173.157057825983));
#21370=CARTESIAN_POINT('Ctrl Pts',(-56.3850236706787,-104.074788028575,
171.985484999752));
#21371=CARTESIAN_POINT('Ctrl Pts',(-58.0226042948486,-103.805929764978,
171.985485069079));
#21372=CARTESIAN_POINT('Ctrl Pts',(-59.6601849190184,-103.537071501381,
171.985485138407));
#21373=CARTESIAN_POINT('Ctrl Pts',(-60.8152184431262,-103.319655982497,
173.157058062683));
#21374=CARTESIAN_POINT('Ctrl Pts',(-61.9702519672339,-103.102240463613,
174.328630986959));
#21375=CARTESIAN_POINT('Ctrl Pts',(-61.9603138353797,-103.009018706307,
175.985485236451));
#21376=CARTESIAN_POINT('Ctrl Pts',(-61.9503757035256,-102.915796949001,
177.642339485944));
#21377=CARTESIAN_POINT('Ctrl Pts',(-60.7754659560919,-102.946768948967,
178.813912312176));
#21378=CARTESIAN_POINT('Ctrl Pts',(-59.6005562086583,-102.977740948934,
179.985485138407));
#21379=CARTESIAN_POINT('Ctrl Pts',(-57.9430994586544,-103.06015568322,179.985485069079));
#21380=CARTESIAN_POINT('Ctrl Pts',(-56.2856427086505,-103.142570417507,
179.985484999752));
#21381=CARTESIAN_POINT('Ctrl Pts',(-55.1107330587087,-103.17354240708,178.813912075476));
#21382=CARTESIAN_POINT('Ctrl Pts',(-53.935823408767,-103.204514396654,177.6423391512));
#21383=CARTESIAN_POINT('Ctrl Pts',(-53.9258854147871,-103.111292624649,
175.985484901707));
#21384=CARTESIAN_POINT('Ctrl Pts',(-53.9159474208072,-103.018070852645,
174.328630652215));
#21385=CARTESIAN_POINT('Ctrl Pts',(-55.0709810424069,-102.800655323367,
173.157057825983));
#21386=CARTESIAN_POINT('Ctrl Pts',(-56.2260146640065,-102.58323979409,171.985484999752));
#21387=CARTESIAN_POINT('Ctrl Pts',(-57.8635952881763,-102.314381530493,
171.985485069079));
#21388=CARTESIAN_POINT('Ctrl Pts',(-59.5011759123462,-102.045523266896,
171.985485138407));
#21389=CARTESIAN_POINT('Ctrl Pts',(-60.6562094364539,-101.828107748012,
173.157058062683));
#21390=CARTESIAN_POINT('Ctrl Pts',(-61.8112429605617,-101.610692229127,
174.328630986959));
#21391=CARTESIAN_POINT('Ctrl Pts',(-61.8013048287075,-101.517470471821,
175.985485236451));
#21392=CARTESIAN_POINT('Ctrl Pts',(-61.7913666968533,-101.424248714515,
177.642339485944));
#21393=CARTESIAN_POINT('Ctrl Pts',(-60.6164569494197,-101.455220714482,
178.813912312176));
#21394=CARTESIAN_POINT('Ctrl Pts',(-59.4415472019861,-101.486192714449,
179.985485138407));
#21395=CARTESIAN_POINT('Ctrl Pts',(-57.7840904519822,-101.568607448735,
179.985485069079));
#21396=CARTESIAN_POINT('Ctrl Pts',(-56.1266337019783,-101.651022183021,
179.985484999752));
#21397=CARTESIAN_POINT('Ctrl Pts',(-54.9517240520365,-101.681994172595,
178.813912075476));
#21398=CARTESIAN_POINT('Ctrl Pts',(-53.7768144020947,-101.712966162168,
177.6423391512));
#21399=CARTESIAN_POINT('Ctrl Pts',(-53.7668764081149,-101.619744390164,
175.985484901707));
#21400=CARTESIAN_POINT('Ctrl Pts',(-53.756938414135,-101.526522618159,174.328630652215));
#21401=CARTESIAN_POINT('Ctrl Pts',(-54.9119720357346,-101.309107088882,
173.157057825983));
#21402=CARTESIAN_POINT('Ctrl Pts',(-56.0670056573342,-101.091691559604,
171.985484999752));
#21403=CARTESIAN_POINT('Ctrl Pts',(-57.7045862815041,-100.822833296007,
171.985485069079));
#21404=CARTESIAN_POINT('Ctrl Pts',(-59.342166905674,-100.55397503241,171.985485138407));
#21405=CARTESIAN_POINT('Ctrl Pts',(-60.4972004297817,-100.336559513526,
173.157058062683));
#21406=CARTESIAN_POINT('Ctrl Pts',(-61.6522339538895,-100.119143994642,
174.328630986959));
#21407=CARTESIAN_POINT('Ctrl Pts',(-61.6422958220353,-100.025922237336,
175.985485236451));
#21408=CARTESIAN_POINT('Ctrl Pts',(-61.6323576901811,-99.9327004800294,
177.642339485944));
#21409=CARTESIAN_POINT('Ctrl Pts',(-60.4574479427475,-99.9636724799962,
178.813912312176));
#21410=CARTESIAN_POINT('Ctrl Pts',(-59.2825381953138,-99.994644479963,179.985485138407));
#21411=CARTESIAN_POINT('Ctrl Pts',(-57.6250814453099,-100.077059214249,
179.985485069079));
#21412=CARTESIAN_POINT('Ctrl Pts',(-55.9676246953061,-100.159473948536,
179.985484999752));
#21413=CARTESIAN_POINT('Ctrl Pts',(-54.7927150453643,-100.190445938109,
178.813912075476));
#21414=CARTESIAN_POINT('Ctrl Pts',(-53.6178053954225,-100.221417927683,
177.6423391512));
#21415=CARTESIAN_POINT('Ctrl Pts',(-53.6078674014426,-100.128196155678,
175.985484901707));
#21416=CARTESIAN_POINT('Ctrl Pts',(-53.5979294074628,-100.034974383673,
174.328630652215));
#21417=CARTESIAN_POINT('Ctrl Pts',(-54.7529630290624,-99.817558854396,173.157057825983));
#21418=CARTESIAN_POINT('Ctrl Pts',(-55.907996650662,-99.6001433251185,171.985484999752));
#21419=CARTESIAN_POINT('Ctrl Pts',(-57.5455772748319,-99.3312850615215,
171.985485069079));
#21420=CARTESIAN_POINT('Ctrl Pts',(-59.1831578990017,-99.0624267979246,
171.985485138407));
#21421=CARTESIAN_POINT('Ctrl Pts',(-60.3381914231095,-98.8450112790404,
173.157058062683));
#21422=CARTESIAN_POINT('Ctrl Pts',(-61.4932249472172,-98.6275957601562,
174.328630986959));
#21423=CARTESIAN_POINT('Ctrl Pts',(-61.4832868153631,-98.53437400285,175.985485236451));
#21424=CARTESIAN_POINT('Ctrl Pts',(-61.4733486835089,-98.4411522455438,
177.642339485944));
#21425=CARTESIAN_POINT('Ctrl Pts',(-60.2984389360752,-98.4721242455106,
178.813912312176));
#21426=CARTESIAN_POINT('Ctrl Pts',(-59.1235291886416,-98.5030962454774,
179.985485138407));
#21427=CARTESIAN_POINT('Ctrl Pts',(-57.4660724386377,-98.5855109797636,
179.985485069079));
#21428=CARTESIAN_POINT('Ctrl Pts',(-55.8086156886338,-98.6679257140499,
179.985484999752));
#21429=CARTESIAN_POINT('Ctrl Pts',(-54.633706038692,-98.6988977036234,178.813912075476));
#21430=CARTESIAN_POINT('Ctrl Pts',(-56.1707931031902,-113.117197303651,
178.813912075476));
#21431=CARTESIAN_POINT('Ctrl Pts',(-54.9958834532485,-113.148169293224,
177.6423391512));
#21432=CARTESIAN_POINT('Ctrl Pts',(-54.9859454592686,-113.05494752122,175.985484901707));
#21433=CARTESIAN_POINT('Ctrl Pts',(-54.9760074652888,-112.961725749215,
174.328630652215));
#21434=CARTESIAN_POINT('Ctrl Pts',(-56.1310410868884,-112.744310219938,
173.157057825983));
#21435=CARTESIAN_POINT('Ctrl Pts',(-57.286074708488,-112.52689469066,171.985484999752));
#21436=CARTESIAN_POINT('Ctrl Pts',(-58.9236553326578,-112.258036427063,
171.985485069079));
#21437=CARTESIAN_POINT('Ctrl Pts',(-60.5612359568277,-111.989178163466,
171.985485138407));
#21438=CARTESIAN_POINT('Ctrl Pts',(-61.7162694809355,-111.771762644582,
173.157058062683));
#21439=CARTESIAN_POINT('Ctrl Pts',(-62.8713030050432,-111.554347125698,
174.328630986959));
#21440=CARTESIAN_POINT('Ctrl Pts',(-62.861364873189,-111.461125368392,175.985485236451));
#21441=CARTESIAN_POINT('Ctrl Pts',(-62.8514267413349,-111.367903611086,
177.642339485944));
#21442=CARTESIAN_POINT('Ctrl Pts',(-61.6765169939012,-111.398875611052,
178.813912312176));
#21443=CARTESIAN_POINT('Ctrl Pts',(-60.5016072464676,-111.429847611019,
179.985485138407));
#21444=CARTESIAN_POINT('Ctrl Pts',(-58.8441504964637,-111.512262345305,
179.985485069079));
#21445=CARTESIAN_POINT('Ctrl Pts',(-57.1866937464598,-111.594677079592,
179.985484999752));
#21446=CARTESIAN_POINT('Ctrl Pts',(-56.011784096518,-111.625649069165,178.813912075476));
#21447=CARTESIAN_POINT('Ctrl Pts',(-54.8368744465763,-111.656621058739,
177.6423391512));
#21448=CARTESIAN_POINT('Ctrl Pts',(-54.8269364525964,-111.563399286734,
175.985484901707));
#21449=CARTESIAN_POINT('Ctrl Pts',(-54.8169984586165,-111.47017751473,174.328630652215));
#21450=CARTESIAN_POINT('Ctrl Pts',(-55.9720320802161,-111.252761985452,
173.157057825983));
#21451=CARTESIAN_POINT('Ctrl Pts',(-57.1270657018158,-111.035346456175,
171.985484999752));
#21452=CARTESIAN_POINT('Ctrl Pts',(-58.7646463259856,-110.766488192578,
171.985485069079));
#21453=CARTESIAN_POINT('Ctrl Pts',(-60.4022269501555,-110.497629928981,
171.985485138407));
#21454=CARTESIAN_POINT('Ctrl Pts',(-61.5572604742632,-110.280214410097,
173.157058062683));
#21455=CARTESIAN_POINT('Ctrl Pts',(-62.712293998371,-110.062798891212,174.328630986959));
#21456=CARTESIAN_POINT('Ctrl Pts',(-62.7023558665168,-109.969577133906,
175.985485236451));
#21457=CARTESIAN_POINT('Ctrl Pts',(-62.6924177346626,-109.8763553766,177.642339485944));
#21458=CARTESIAN_POINT('Ctrl Pts',(-61.517507987229,-109.907327376567,178.813912312176));
#21459=CARTESIAN_POINT('Ctrl Pts',(-60.3425982397954,-109.938299376534,
179.985485138407));
#21460=CARTESIAN_POINT('Ctrl Pts',(-58.6851414897915,-110.02071411082,179.985485069079));
#21461=CARTESIAN_POINT('Ctrl Pts',(-57.0276847397876,-110.103128845106,
179.985484999752));
#21462=CARTESIAN_POINT('Ctrl Pts',(-55.8527750898458,-110.13410083468,178.813912075476));
#21463=CARTESIAN_POINT('Ctrl Pts',(-54.677865439904,-110.165072824253,177.6423391512));
#21464=CARTESIAN_POINT('Ctrl Pts',(-54.6679274459242,-110.071851052249,
175.985484901707));
#21465=CARTESIAN_POINT('Ctrl Pts',(-54.6579894519443,-109.978629280244,
174.328630652215));
#21466=CARTESIAN_POINT('Ctrl Pts',(-55.8130230735439,-109.761213750967,
173.157057825983));
#21467=CARTESIAN_POINT('Ctrl Pts',(-56.9680566951435,-109.543798221689,
171.985484999752));
#21468=CARTESIAN_POINT('Ctrl Pts',(-58.6056373193134,-109.274939958092,
171.985485069079));
#21469=CARTESIAN_POINT('Ctrl Pts',(-60.2432179434833,-109.006081694495,
171.985485138407));
#21470=CARTESIAN_POINT('Ctrl Pts',(-61.398251467591,-108.788666175611,173.157058062683));
#21471=CARTESIAN_POINT('Ctrl Pts',(-62.5532849916988,-108.571250656727,
174.328630986959));
#21472=CARTESIAN_POINT('Ctrl Pts',(-62.5433468598446,-108.478028899421,
175.985485236451));
#21473=CARTESIAN_POINT('Ctrl Pts',(-62.5334087279904,-108.384807142114,
177.642339485944));
#21474=CARTESIAN_POINT('Ctrl Pts',(-61.3584989805568,-108.415779142081,
178.813912312176));
#21475=CARTESIAN_POINT('Ctrl Pts',(-60.1835892331231,-108.446751142048,
179.985485138407));
#21476=CARTESIAN_POINT('Ctrl Pts',(-58.5261324831192,-108.529165876334,
179.985485069079));
#21477=CARTESIAN_POINT('Ctrl Pts',(-56.8686757331153,-108.611580610621,
179.985484999752));
#21478=CARTESIAN_POINT('Ctrl Pts',(-55.6937660831736,-108.642552600194,
178.813912075476));
#21479=CARTESIAN_POINT('Ctrl Pts',(-54.5188564332318,-108.673524589768,
177.6423391512));
#21480=CARTESIAN_POINT('Ctrl Pts',(-54.5089184392519,-108.580302817763,
175.985484901707));
#21481=CARTESIAN_POINT('Ctrl Pts',(-54.4989804452721,-108.487081045759,
174.328630652215));
#21482=CARTESIAN_POINT('Ctrl Pts',(-55.6540140668717,-108.269665516481,
173.157057825983));
#21483=CARTESIAN_POINT('Ctrl Pts',(-56.8090476884713,-108.052249987204,
171.985484999752));
#21484=CARTESIAN_POINT('Ctrl Pts',(-58.4466283126412,-107.783391723607,
171.985485069079));
#21485=CARTESIAN_POINT('Ctrl Pts',(-60.084208936811,-107.51453346001,171.985485138407));
#21486=CARTESIAN_POINT('Ctrl Pts',(-61.2392424609188,-107.297117941125,
173.157058062683));
#21487=CARTESIAN_POINT('Ctrl Pts',(-62.3942759850265,-107.079702422241,
174.328630986959));
#21488=CARTESIAN_POINT('Ctrl Pts',(-62.3843378531723,-106.986480664935,
175.985485236451));
#21489=CARTESIAN_POINT('Ctrl Pts',(-62.3743997213182,-106.893258907629,
177.642339485944));
#21490=CARTESIAN_POINT('Ctrl Pts',(-61.1994899738845,-106.924230907596,
178.813912312176));
#21491=CARTESIAN_POINT('Ctrl Pts',(-60.0245802264509,-106.955202907562,
179.985485138407));
#21492=CARTESIAN_POINT('Ctrl Pts',(-58.367123476447,-107.037617641849,179.985485069079));
#21493=CARTESIAN_POINT('Ctrl Pts',(-56.7096667264431,-107.120032376135,
179.985484999752));
#21494=CARTESIAN_POINT('Ctrl Pts',(-55.5347570765013,-107.151004365708,
178.813912075476));
#21495=CARTESIAN_POINT('Ctrl Pts',(-54.3598474265596,-107.181976355282,
177.6423391512));
#21496=CARTESIAN_POINT('Ctrl Pts',(-54.3499094325797,-107.088754583277,
175.985484901707));
#21497=CARTESIAN_POINT('Ctrl Pts',(-54.3399714385999,-106.995532811273,
174.328630652215));
#21498=CARTESIAN_POINT('Ctrl Pts',(-55.4950050601995,-106.778117281995,
173.157057825983));
#21499=CARTESIAN_POINT('Ctrl Pts',(-56.6500386817991,-106.560701752718,
171.985484999752));
#21500=CARTESIAN_POINT('Ctrl Pts',(-58.2876193059689,-106.291843489121,
171.985485069079));
#21501=CARTESIAN_POINT('Ctrl Pts',(-59.9251999301388,-106.022985225524,
171.985485138407));
#21502=CARTESIAN_POINT('Ctrl Pts',(-61.0802334542465,-105.80556970664,173.157058062683));
#21503=CARTESIAN_POINT('Ctrl Pts',(-62.2352669783543,-105.588154187756,
174.328630986959));
#21504=CARTESIAN_POINT('Ctrl Pts',(-62.2253288465001,-105.494932430449,
175.985485236451));
#21505=CARTESIAN_POINT('Ctrl Pts',(-62.2153907146459,-105.401710673143,
177.642339485944));
#21506=CARTESIAN_POINT('Ctrl Pts',(-61.0404809672123,-105.43268267311,178.813912312176));
#21507=CARTESIAN_POINT('Ctrl Pts',(-59.8655712197787,-105.463654673077,
179.985485138407));
#21508=CARTESIAN_POINT('Ctrl Pts',(-58.2081144697748,-105.546069407363,
179.985485069079));
#21509=CARTESIAN_POINT('Ctrl Pts',(-56.5506577197709,-105.628484141649,
179.985484999752));
#21510=CARTESIAN_POINT('Ctrl Pts',(-55.3757480698291,-105.659456131223,
178.813912075476));
#21511=CARTESIAN_POINT('Ctrl Pts',(-54.2008384198873,-105.690428120796,
177.6423391512));
#21512=CARTESIAN_POINT('Ctrl Pts',(-54.1909004259075,-105.597206348792,
175.985484901707));
#21513=CARTESIAN_POINT('Ctrl Pts',(-54.1809624319276,-105.503984576787,
174.328630652215));
#21514=CARTESIAN_POINT('Ctrl Pts',(-55.3359960535272,-105.28656904751,173.157057825983));
#21515=CARTESIAN_POINT('Ctrl Pts',(-56.4910296751268,-105.069153518232,
171.985484999752));
#21516=CARTESIAN_POINT('Ctrl Pts',(-58.1286102992967,-104.800295254635,
171.985485069079));
#21517=CARTESIAN_POINT('Ctrl Pts',(-59.7661909234666,-104.531436991038,
171.985485138407));
#21518=CARTESIAN_POINT('Ctrl Pts',(-60.9212244475743,-104.314021472154,
173.157058062683));
#21519=CARTESIAN_POINT('Ctrl Pts',(-62.0762579716821,-104.09660595327,174.328630986959));
#21520=CARTESIAN_POINT('Ctrl Pts',(-62.0663198398279,-104.003384195964,
175.985485236451));
#21521=CARTESIAN_POINT('Ctrl Pts',(-62.0563817079737,-103.910162438658,
177.642339485944));
#21522=CARTESIAN_POINT('Ctrl Pts',(-60.8814719605401,-103.941134438624,
178.813912312176));
#21523=CARTESIAN_POINT('Ctrl Pts',(-59.7065622131064,-103.972106438591,
179.985485138407));
#21524=CARTESIAN_POINT('Ctrl Pts',(-58.0491054631025,-104.054521172878,
179.985485069079));
#21525=CARTESIAN_POINT('Ctrl Pts',(-56.3916487130987,-104.136935907164,
179.985484999752));
#21526=CARTESIAN_POINT('Ctrl Pts',(-55.2167390631569,-104.167907896737,
178.813912075476));
#21527=CARTESIAN_POINT('Ctrl Pts',(-54.0418294132151,-104.198879886311,
177.6423391512));
#21528=CARTESIAN_POINT('Ctrl Pts',(-54.0318914192353,-104.105658114306,
175.985484901707));
#21529=CARTESIAN_POINT('Ctrl Pts',(-54.0219534252554,-104.012436342302,
174.328630652215));
#21530=CARTESIAN_POINT('Ctrl Pts',(-55.176987046855,-103.795020813024,173.157057825983));
#21531=CARTESIAN_POINT('Ctrl Pts',(-56.3320206684546,-103.577605283747,
171.985484999752));
#21532=CARTESIAN_POINT('Ctrl Pts',(-57.9696012926245,-103.30874702015,171.985485069079));
#21533=CARTESIAN_POINT('Ctrl Pts',(-59.6071819167943,-103.039888756553,
171.985485138407));
#21534=CARTESIAN_POINT('Ctrl Pts',(-60.7622154409021,-102.822473237669,
173.157058062683));
#21535=CARTESIAN_POINT('Ctrl Pts',(-61.9172489650099,-102.605057718784,
174.328630986959));
#21536=CARTESIAN_POINT('Ctrl Pts',(-61.9073108331557,-102.511835961478,
175.985485236451));
#21537=CARTESIAN_POINT('Ctrl Pts',(-61.8973727013015,-102.418614204172,
177.642339485944));
#21538=CARTESIAN_POINT('Ctrl Pts',(-60.7224629538678,-102.449586204139,
178.813912312176));
#21539=CARTESIAN_POINT('Ctrl Pts',(-59.5475532064342,-102.480558204106,
179.985485138407));
#21540=CARTESIAN_POINT('Ctrl Pts',(-57.8900964564303,-102.562972938392,
179.985485069079));
#21541=CARTESIAN_POINT('Ctrl Pts',(-56.2326397064264,-102.645387672678,
179.985484999752));
#21542=CARTESIAN_POINT('Ctrl Pts',(-55.0577300564847,-102.676359662252,
178.813912075476));
#21543=CARTESIAN_POINT('Ctrl Pts',(-53.8828204065429,-102.707331651825,
177.6423391512));
#21544=CARTESIAN_POINT('Ctrl Pts',(-53.872882412563,-102.614109879821,175.985484901707));
#21545=CARTESIAN_POINT('Ctrl Pts',(-53.8629444185832,-102.520888107816,
174.328630652215));
#21546=CARTESIAN_POINT('Ctrl Pts',(-55.0179780401828,-102.303472578539,
173.157057825983));
#21547=CARTESIAN_POINT('Ctrl Pts',(-56.1730116617824,-102.086057049261,
171.985484999752));
#21548=CARTESIAN_POINT('Ctrl Pts',(-57.8105922859523,-101.817198785664,
171.985485069079));
#21549=CARTESIAN_POINT('Ctrl Pts',(-59.4481729101221,-101.548340522067,
171.985485138407));
#21550=CARTESIAN_POINT('Ctrl Pts',(-60.6032064342299,-101.330925003183,
173.157058062683));
#21551=CARTESIAN_POINT('Ctrl Pts',(-61.7582399583376,-101.113509484299,
174.328630986959));
#21552=CARTESIAN_POINT('Ctrl Pts',(-61.7483018264834,-101.020287726993,
175.985485236451));
#21553=CARTESIAN_POINT('Ctrl Pts',(-61.7383636946293,-100.927065969686,
177.642339485944));
#21554=CARTESIAN_POINT('Ctrl Pts',(-60.5634539471956,-100.958037969653,
178.813912312176));
#21555=CARTESIAN_POINT('Ctrl Pts',(-59.388544199762,-100.98900996962,179.985485138407));
#21556=CARTESIAN_POINT('Ctrl Pts',(-57.7310874497581,-101.071424703906,
179.985485069079));
#21557=CARTESIAN_POINT('Ctrl Pts',(-56.0736306997542,-101.153839438193,
179.985484999752));
#21558=CARTESIAN_POINT('Ctrl Pts',(-54.8987210498124,-101.184811427766,
178.813912075476));
#21559=CARTESIAN_POINT('Ctrl Pts',(-53.7238113998707,-101.21578341734,177.6423391512));
#21560=CARTESIAN_POINT('Ctrl Pts',(-53.7138734058908,-101.122561645335,
175.985484901707));
#21561=CARTESIAN_POINT('Ctrl Pts',(-53.7039354119109,-101.029339873331,
174.328630652215));
#21562=CARTESIAN_POINT('Ctrl Pts',(-54.8589690335105,-100.811924344053,
173.157057825983));
#21563=CARTESIAN_POINT('Ctrl Pts',(-56.0140026551102,-100.594508814776,
171.985484999752));
#21564=CARTESIAN_POINT('Ctrl Pts',(-57.65158327928,-100.325650551179,171.985485069079));
#21565=CARTESIAN_POINT('Ctrl Pts',(-59.2891639034499,-100.056792287582,
171.985485138407));
#21566=CARTESIAN_POINT('Ctrl Pts',(-60.4441974275576,-99.8393767686974,
173.157058062683));
#21567=CARTESIAN_POINT('Ctrl Pts',(-61.5992309516654,-99.6219612498133,
174.328630986959));
#21568=CARTESIAN_POINT('Ctrl Pts',(-61.5892928198112,-99.528739492507,175.985485236451));
#21569=CARTESIAN_POINT('Ctrl Pts',(-61.579354687957,-99.4355177352008,177.642339485944));
#21570=CARTESIAN_POINT('Ctrl Pts',(-60.4044449405234,-99.4664897351676,
178.813912312176));
#21571=CARTESIAN_POINT('Ctrl Pts',(-59.2295351930898,-99.4974617351344,
179.985485138407));
#21572=CARTESIAN_POINT('Ctrl Pts',(-57.5720784430859,-99.5798764694207,
179.985485069079));
#21573=CARTESIAN_POINT('Ctrl Pts',(-55.914621693082,-99.662291203707,179.985484999752));
#21574=CARTESIAN_POINT('Ctrl Pts',(-54.7397120431402,-99.6932631932805,
178.813912075476));
#21575=CARTESIAN_POINT('Ctrl Pts',(-53.5648023931984,-99.724235182854,177.6423391512));
#21576=CARTESIAN_POINT('Ctrl Pts',(-53.5548643992186,-99.6310134108495,
175.985484901707));
#21577=CARTESIAN_POINT('Ctrl Pts',(-53.5449264052387,-99.5377916388449,
174.328630652215));
#21578=CARTESIAN_POINT('Ctrl Pts',(-54.6999600268383,-99.3203761095675,
173.157057825983));
#21579=CARTESIAN_POINT('Ctrl Pts',(-55.8549936484379,-99.10296058029,171.985484999752));
#21580=CARTESIAN_POINT('Ctrl Pts',(-57.4925742726078,-98.834102316693,171.985485069079));
#21581=CARTESIAN_POINT('Ctrl Pts',(-59.1301548967777,-98.5652440530961,
171.985485138407));
#21582=CARTESIAN_POINT('Ctrl Pts',(-60.2851884208854,-98.3478285342118,
173.157058062683));
#21583=CARTESIAN_POINT('Ctrl Pts',(-61.4402219449932,-98.1304130153276,
174.328630986959));
#21584=CARTESIAN_POINT('Ctrl Pts',(-61.430283813139,-98.0371912580215,175.985485236451));
#21585=CARTESIAN_POINT('Ctrl Pts',(-61.4203456812848,-97.9439695007152,
177.642339485944));
#21586=CARTESIAN_POINT('Ctrl Pts',(-60.2454359338512,-97.974941500682,178.813912312176));
#21587=CARTESIAN_POINT('Ctrl Pts',(-59.0705261864175,-98.0059135006488,
179.985485138407));
#21588=CARTESIAN_POINT('Ctrl Pts',(-57.4130694364136,-98.0883282349351,
179.985485069079));
#21589=CARTESIAN_POINT('Ctrl Pts',(-55.3334083509023,-98.1917364932607,
179.985484982092));
#21590=CARTESIAN_POINT('Ctrl Pts',(-54.1340831983237,-98.2115101422526,
178.284125180033));
#21591=CARTESIAN_POINT('Ctrl Pts',(-56.1811453168472,-113.284079398529,
178.821308694947));
#21592=CARTESIAN_POINT('Ctrl Pts',(-55.0031891497056,-113.315376167189,
177.646671990314));
#21593=CARTESIAN_POINT('Ctrl Pts',(-54.993251155906,-113.222154395166,175.98548490127));
#21594=CARTESIAN_POINT('Ctrl Pts',(-54.9833131621064,-113.128932623142,
174.324297812226));
#21595=CARTESIAN_POINT('Ctrl Pts',(-56.1413933011608,-112.91119231475,173.149661205893));
#21596=CARTESIAN_POINT('Ctrl Pts',(-57.2994734402153,-112.693452006359,
171.975024599561));
#21597=CARTESIAN_POINT('Ctrl Pts',(-58.9413624905075,-112.424134435753,
171.97502466907));
#21598=CARTESIAN_POINT('Ctrl Pts',(-60.5832515407998,-112.154816865147,
171.975024738579));
#21599=CARTESIAN_POINT('Ctrl Pts',(-61.7413315821074,-111.937076567176,
173.149661443212));
#21600=CARTESIAN_POINT('Ctrl Pts',(-62.8994116234151,-111.719336269205,
174.324298147845));
#21601=CARTESIAN_POINT('Ctrl Pts',(-62.8894734913806,-111.626114511918,
175.985485236889));
#21602=CARTESIAN_POINT('Ctrl Pts',(-62.8795353593462,-111.532892754631,
177.646672325933));
#21603=CARTESIAN_POINT('Ctrl Pts',(-61.7015790944577,-111.564189533712,
178.821308932265));
#21604=CARTESIAN_POINT('Ctrl Pts',(-60.5236228295692,-111.595486312793,
179.995945538598));
#21605=CARTESIAN_POINT('Ctrl Pts',(-58.8618576534429,-111.678360354088,
179.995945469089));
#21606=CARTESIAN_POINT('Ctrl Pts',(-57.2000924773167,-111.761234395383,
179.99594539958));
#21607=CARTESIAN_POINT('Ctrl Pts',(-56.022136310175,-111.792531164043,178.821308694947));
#21608=CARTESIAN_POINT('Ctrl Pts',(-54.8441801430333,-111.823827932704,
177.646671990314));
#21609=CARTESIAN_POINT('Ctrl Pts',(-54.8342421492337,-111.73060616068,175.98548490127));
#21610=CARTESIAN_POINT('Ctrl Pts',(-54.8243041554342,-111.637384388656,
174.324297812226));
#21611=CARTESIAN_POINT('Ctrl Pts',(-55.9823842944886,-111.419644080265,
173.149661205893));
#21612=CARTESIAN_POINT('Ctrl Pts',(-57.1404644335431,-111.201903771873,
171.975024599561));
#21613=CARTESIAN_POINT('Ctrl Pts',(-58.7823534838353,-110.932586201267,
171.97502466907));
#21614=CARTESIAN_POINT('Ctrl Pts',(-60.4242425341276,-110.663268630661,
171.975024738579));
#21615=CARTESIAN_POINT('Ctrl Pts',(-61.5823225754352,-110.44552833269,173.149661443212));
#21616=CARTESIAN_POINT('Ctrl Pts',(-62.7404026167429,-110.227788034719,
174.324298147845));
#21617=CARTESIAN_POINT('Ctrl Pts',(-62.7304644847084,-110.134566277432,
175.985485236889));
#21618=CARTESIAN_POINT('Ctrl Pts',(-62.720526352674,-110.041344520145,177.646672325933));
#21619=CARTESIAN_POINT('Ctrl Pts',(-61.5425700877854,-110.072641299226,
178.821308932265));
#21620=CARTESIAN_POINT('Ctrl Pts',(-60.364613822897,-110.103938078307,179.995945538598));
#21621=CARTESIAN_POINT('Ctrl Pts',(-58.7028486467707,-110.186812119602,
179.995945469089));
#21622=CARTESIAN_POINT('Ctrl Pts',(-57.0410834706445,-110.269686160897,
179.99594539958));
#21623=CARTESIAN_POINT('Ctrl Pts',(-55.8631273035028,-110.300982929558,
178.821308694947));
#21624=CARTESIAN_POINT('Ctrl Pts',(-54.6851711363611,-110.332279698218,
177.646671990314));
#21625=CARTESIAN_POINT('Ctrl Pts',(-54.6752331425615,-110.239057926194,
175.98548490127));
#21626=CARTESIAN_POINT('Ctrl Pts',(-54.665295148762,-110.145836154171,174.324297812226));
#21627=CARTESIAN_POINT('Ctrl Pts',(-55.8233752878164,-109.928095845779,
173.149661205893));
#21628=CARTESIAN_POINT('Ctrl Pts',(-56.9814554268709,-109.710355537387,
171.975024599561));
#21629=CARTESIAN_POINT('Ctrl Pts',(-58.6233444771631,-109.441037966782,
171.97502466907));
#21630=CARTESIAN_POINT('Ctrl Pts',(-60.2652335274553,-109.171720396176,
171.975024738579));
#21631=CARTESIAN_POINT('Ctrl Pts',(-61.423313568763,-108.953980098205,173.149661443212));
#21632=CARTESIAN_POINT('Ctrl Pts',(-62.5813936100706,-108.736239800234,
174.324298147845));
#21633=CARTESIAN_POINT('Ctrl Pts',(-62.5714554780362,-108.643018042946,
175.985485236889));
#21634=CARTESIAN_POINT('Ctrl Pts',(-62.5615173460017,-108.54979628566,177.646672325933));
#21635=CARTESIAN_POINT('Ctrl Pts',(-61.3835610811132,-108.58109306474,178.821308932265));
#21636=CARTESIAN_POINT('Ctrl Pts',(-60.2056048162248,-108.612389843821,
179.995945538598));
#21637=CARTESIAN_POINT('Ctrl Pts',(-58.5438396400985,-108.695263885116,
179.995945469089));
#21638=CARTESIAN_POINT('Ctrl Pts',(-56.8820744639722,-108.778137926412,
179.99594539958));
#21639=CARTESIAN_POINT('Ctrl Pts',(-55.7041182968305,-108.809434695072,
178.821308694947));
#21640=CARTESIAN_POINT('Ctrl Pts',(-54.5261621296889,-108.840731463732,
177.646671990314));
#21641=CARTESIAN_POINT('Ctrl Pts',(-54.5162241358893,-108.747509691709,
175.98548490127));
#21642=CARTESIAN_POINT('Ctrl Pts',(-54.5062861420897,-108.654287919685,
174.324297812226));
#21643=CARTESIAN_POINT('Ctrl Pts',(-55.6643662811442,-108.436547611293,
173.149661205893));
#21644=CARTESIAN_POINT('Ctrl Pts',(-56.8224464201986,-108.218807302902,
171.975024599561));
#21645=CARTESIAN_POINT('Ctrl Pts',(-58.4643354704908,-107.949489732296,
171.97502466907));
#21646=CARTESIAN_POINT('Ctrl Pts',(-60.1062245207831,-107.68017216169,171.975024738579));
#21647=CARTESIAN_POINT('Ctrl Pts',(-61.2643045620907,-107.462431863719,
173.149661443212));
#21648=CARTESIAN_POINT('Ctrl Pts',(-62.4223846033984,-107.244691565748,
174.324298147845));
#21649=CARTESIAN_POINT('Ctrl Pts',(-62.4124464713639,-107.151469808461,
175.985485236889));
#21650=CARTESIAN_POINT('Ctrl Pts',(-62.4025083393295,-107.058248051174,
177.646672325933));
#21651=CARTESIAN_POINT('Ctrl Pts',(-61.224552074441,-107.089544830255,178.821308932265));
#21652=CARTESIAN_POINT('Ctrl Pts',(-60.0465958095525,-107.120841609336,
179.995945538598));
#21653=CARTESIAN_POINT('Ctrl Pts',(-58.3848306334262,-107.203715650631,
179.995945469089));
#21654=CARTESIAN_POINT('Ctrl Pts',(-56.7230654573,-107.286589691926,179.99594539958));
#21655=CARTESIAN_POINT('Ctrl Pts',(-55.5451092901583,-107.317886460586,
178.821308694947));
#21656=CARTESIAN_POINT('Ctrl Pts',(-54.3671531230166,-107.349183229247,
177.646671990314));
#21657=CARTESIAN_POINT('Ctrl Pts',(-54.357215129217,-107.255961457223,175.98548490127));
#21658=CARTESIAN_POINT('Ctrl Pts',(-54.3472771354175,-107.162739685199,
174.324297812226));
#21659=CARTESIAN_POINT('Ctrl Pts',(-55.5053572744719,-106.944999376808,
173.149661205893));
#21660=CARTESIAN_POINT('Ctrl Pts',(-56.6634374135264,-106.727259068416,
171.975024599561));
#21661=CARTESIAN_POINT('Ctrl Pts',(-58.3053264638186,-106.45794149781,171.97502466907));
#21662=CARTESIAN_POINT('Ctrl Pts',(-59.9472155141109,-106.188623927205,
171.975024738579));
#21663=CARTESIAN_POINT('Ctrl Pts',(-61.1052955554185,-105.970883629233,
173.149661443212));
#21664=CARTESIAN_POINT('Ctrl Pts',(-62.2633755967262,-105.753143331262,
174.324298147845));
#21665=CARTESIAN_POINT('Ctrl Pts',(-62.2534374646917,-105.659921573975,
175.985485236889));
#21666=CARTESIAN_POINT('Ctrl Pts',(-62.2434993326573,-105.566699816688,
177.646672325933));
#21667=CARTESIAN_POINT('Ctrl Pts',(-61.0655430677688,-105.597996595769,
178.821308932265));
#21668=CARTESIAN_POINT('Ctrl Pts',(-59.8875868028803,-105.62929337485,179.995945538598));
#21669=CARTESIAN_POINT('Ctrl Pts',(-58.225821626754,-105.712167416145,179.995945469089));
#21670=CARTESIAN_POINT('Ctrl Pts',(-56.5640564506278,-105.79504145744,179.99594539958));
#21671=CARTESIAN_POINT('Ctrl Pts',(-55.3861002834861,-105.826338226101,
178.821308694947));
#21672=CARTESIAN_POINT('Ctrl Pts',(-54.2081441163444,-105.857634994761,
177.646671990314));
#21673=CARTESIAN_POINT('Ctrl Pts',(-54.1982061225448,-105.764413222738,
175.98548490127));
#21674=CARTESIAN_POINT('Ctrl Pts',(-54.1882681287453,-105.671191450714,
174.324297812226));
#21675=CARTESIAN_POINT('Ctrl Pts',(-55.3463482677997,-105.453451142322,
173.149661205893));
#21676=CARTESIAN_POINT('Ctrl Pts',(-56.5044284068542,-105.235710833931,
171.975024599561));
#21677=CARTESIAN_POINT('Ctrl Pts',(-58.1463174571464,-104.966393263325,
171.97502466907));
#21678=CARTESIAN_POINT('Ctrl Pts',(-59.7882065074387,-104.697075692719,
171.975024738579));
#21679=CARTESIAN_POINT('Ctrl Pts',(-60.9462865487463,-104.479335394748,
173.149661443212));
#21680=CARTESIAN_POINT('Ctrl Pts',(-62.104366590054,-104.261595096777,174.324298147845));
#21681=CARTESIAN_POINT('Ctrl Pts',(-62.0944284580195,-104.16837333949,175.985485236889));
#21682=CARTESIAN_POINT('Ctrl Pts',(-62.0844903259851,-104.075151582203,
177.646672325933));
#21683=CARTESIAN_POINT('Ctrl Pts',(-60.9065340610965,-104.106448361284,
178.821308932265));
#21684=CARTESIAN_POINT('Ctrl Pts',(-59.7285777962081,-104.137745140365,
179.995945538598));
#21685=CARTESIAN_POINT('Ctrl Pts',(-58.0668126200818,-104.22061918166,179.995945469089));
#21686=CARTESIAN_POINT('Ctrl Pts',(-56.4050474439555,-104.303493222955,
179.99594539958));
#21687=CARTESIAN_POINT('Ctrl Pts',(-55.2270912768138,-104.334789991615,
178.821308694947));
#21688=CARTESIAN_POINT('Ctrl Pts',(-54.0491351096722,-104.366086760276,
177.646671990314));
#21689=CARTESIAN_POINT('Ctrl Pts',(-54.0391971158726,-104.272864988252,
175.98548490127));
#21690=CARTESIAN_POINT('Ctrl Pts',(-54.029259122073,-104.179643216228,174.324297812226));
#21691=CARTESIAN_POINT('Ctrl Pts',(-55.1873392611275,-103.961902907837,
173.149661205893));
#21692=CARTESIAN_POINT('Ctrl Pts',(-56.3454194001819,-103.744162599445,
171.975024599561));
#21693=CARTESIAN_POINT('Ctrl Pts',(-57.9873084504742,-103.474845028839,
171.97502466907));
#21694=CARTESIAN_POINT('Ctrl Pts',(-59.6291975007664,-103.205527458233,
171.975024738579));
#21695=CARTESIAN_POINT('Ctrl Pts',(-60.7872775420741,-102.987787160262,
173.149661443212));
#21696=CARTESIAN_POINT('Ctrl Pts',(-61.9453575833817,-102.770046862291,
174.324298147845));
#21697=CARTESIAN_POINT('Ctrl Pts',(-61.9354194513472,-102.676825105004,
175.985485236889));
#21698=CARTESIAN_POINT('Ctrl Pts',(-61.9254813193128,-102.583603347717,
177.646672325933));
#21699=CARTESIAN_POINT('Ctrl Pts',(-60.7475250544243,-102.614900126798,
178.821308932265));
#21700=CARTESIAN_POINT('Ctrl Pts',(-59.5695687895358,-102.646196905879,
179.995945538598));
#21701=CARTESIAN_POINT('Ctrl Pts',(-57.9078036134095,-102.729070947174,
179.995945469089));
#21702=CARTESIAN_POINT('Ctrl Pts',(-56.2460384372833,-102.811944988469,
179.99594539958));
#21703=CARTESIAN_POINT('Ctrl Pts',(-55.0680822701416,-102.84324175713,178.821308694947));
#21704=CARTESIAN_POINT('Ctrl Pts',(-53.890126103,-102.87453852579,177.646671990314));
#21705=CARTESIAN_POINT('Ctrl Pts',(-53.8801881092004,-102.781316753766,
175.98548490127));
#21706=CARTESIAN_POINT('Ctrl Pts',(-53.8702501154008,-102.688094981743,
174.324297812226));
#21707=CARTESIAN_POINT('Ctrl Pts',(-55.0283302544552,-102.470354673351,
173.149661205893));
#21708=CARTESIAN_POINT('Ctrl Pts',(-56.1864103935097,-102.252614364959,
171.975024599561));
#21709=CARTESIAN_POINT('Ctrl Pts',(-57.8282994438019,-101.983296794354,
171.97502466907));
#21710=CARTESIAN_POINT('Ctrl Pts',(-59.4701884940942,-101.713979223748,
171.975024738579));
#21711=CARTESIAN_POINT('Ctrl Pts',(-60.6282685354018,-101.496238925777,
173.149661443212));
#21712=CARTESIAN_POINT('Ctrl Pts',(-61.7863485767095,-101.278498627806,
174.324298147845));
#21713=CARTESIAN_POINT('Ctrl Pts',(-61.776410444675,-101.185276870519,175.985485236889));
#21714=CARTESIAN_POINT('Ctrl Pts',(-61.7664723126406,-101.092055113232,
177.646672325933));
#21715=CARTESIAN_POINT('Ctrl Pts',(-60.5885160477521,-101.123351892312,
178.821308932265));
#21716=CARTESIAN_POINT('Ctrl Pts',(-59.4105597828636,-101.154648671393,
179.995945538598));
#21717=CARTESIAN_POINT('Ctrl Pts',(-57.7487946067373,-101.237522712688,
179.995945469089));
#21718=CARTESIAN_POINT('Ctrl Pts',(-56.0870294306111,-101.320396753984,
179.99594539958));
#21719=CARTESIAN_POINT('Ctrl Pts',(-54.9090732634694,-101.351693522644,
178.821308694947));
#21720=CARTESIAN_POINT('Ctrl Pts',(-53.7311170963277,-101.382990291305,
177.646671990314));
#21721=CARTESIAN_POINT('Ctrl Pts',(-53.7211791025281,-101.289768519281,
175.98548490127));
#21722=CARTESIAN_POINT('Ctrl Pts',(-53.7112411087286,-101.196546747257,
174.324297812226));
#21723=CARTESIAN_POINT('Ctrl Pts',(-54.869321247783,-100.978806438865,173.149661205893));
#21724=CARTESIAN_POINT('Ctrl Pts',(-56.0274013868375,-100.761066130474,
171.975024599561));
#21725=CARTESIAN_POINT('Ctrl Pts',(-57.6692904371297,-100.491748559868,
171.97502466907));
#21726=CARTESIAN_POINT('Ctrl Pts',(-59.311179487422,-100.222430989262,171.975024738579));
#21727=CARTESIAN_POINT('Ctrl Pts',(-60.4692595287296,-100.004690691291,
173.149661443212));
#21728=CARTESIAN_POINT('Ctrl Pts',(-61.6273395700373,-99.7869503933199,
174.324298147845));
#21729=CARTESIAN_POINT('Ctrl Pts',(-61.6174014380028,-99.6937286360329,
175.985485236889));
#21730=CARTESIAN_POINT('Ctrl Pts',(-61.6074633059684,-99.6005068787459,
177.646672325933));
#21731=CARTESIAN_POINT('Ctrl Pts',(-60.4295070410798,-99.6318036578269,
178.821308932265));
#21732=CARTESIAN_POINT('Ctrl Pts',(-59.2515507761914,-99.6631004369078,
179.995945538598));
#21733=CARTESIAN_POINT('Ctrl Pts',(-57.5897856000651,-99.7459744782029,
179.995945469089));
#21734=CARTESIAN_POINT('Ctrl Pts',(-55.9280204239389,-99.828848519498,179.99594539958));
#21735=CARTESIAN_POINT('Ctrl Pts',(-54.7500642567972,-99.8601452881584,
178.821308694947));
#21736=CARTESIAN_POINT('Ctrl Pts',(-53.5721080896555,-99.8914420568189,
177.646671990314));
#21737=CARTESIAN_POINT('Ctrl Pts',(-53.5621700958559,-99.7982202847951,
175.98548490127));
#21738=CARTESIAN_POINT('Ctrl Pts',(-53.5522321020564,-99.7049985127714,
174.324297812226));
#21739=CARTESIAN_POINT('Ctrl Pts',(-54.7103122411108,-99.4872582043798,
173.149661205893));
#21740=CARTESIAN_POINT('Ctrl Pts',(-55.8683923801653,-99.2695178959882,
171.975024599561));
#21741=CARTESIAN_POINT('Ctrl Pts',(-57.5102814304575,-99.0002003253824,
171.97502466907));
#21742=CARTESIAN_POINT('Ctrl Pts',(-59.1521704807498,-98.7308827547766,
171.975024738579));
#21743=CARTESIAN_POINT('Ctrl Pts',(-60.3102505220574,-98.5131424568055,
173.149661443212));
#21744=CARTESIAN_POINT('Ctrl Pts',(-61.468330563365,-98.2954021588343,174.324298147845));
#21745=CARTESIAN_POINT('Ctrl Pts',(-61.4583924313306,-98.2021804015473,
175.985485236889));
#21746=CARTESIAN_POINT('Ctrl Pts',(-61.4484542992961,-98.1089586442604,
177.646672325933));
#21747=CARTESIAN_POINT('Ctrl Pts',(-60.2704980344076,-98.1402554233413,
178.821308932265));
#21748=CARTESIAN_POINT('Ctrl Pts',(-59.0925417695192,-98.1715522024222,
179.995945538598));
#21749=CARTESIAN_POINT('Ctrl Pts',(-57.4307765933929,-98.2544262437173,
179.995945469089));
#21750=CARTESIAN_POINT('Ctrl Pts',(-55.3457095953916,-98.3584108084307,
179.995945381874));
#21751=CARTESIAN_POINT('Ctrl Pts',(-54.1432778809914,-98.3785156376673,
178.290136353792));
#21752=CARTESIAN_POINT('Ctrl Pts',(-56.1989083789663,-113.450500188295,
178.821287321967));
#21753=CARTESIAN_POINT('Ctrl Pts',(-55.0209610149206,-113.481796018486,
177.646659470313));
#21754=CARTESIAN_POINT('Ctrl Pts',(-55.0110230211205,-113.388574246463,
175.985484901271));
#21755=CARTESIAN_POINT('Ctrl Pts',(-55.0010850273204,-113.295352474439,
174.324310332229));
#21756=CARTESIAN_POINT('Ctrl Pts',(-56.1591563632782,-113.077613104516,
173.149682578875));
#21757=CARTESIAN_POINT('Ctrl Pts',(-57.317227699236,-112.859873734594,171.975054825521));
#21758=CARTESIAN_POINT('Ctrl Pts',(-58.95910430007,-112.590557491183,171.97505489503));
#21759=CARTESIAN_POINT('Ctrl Pts',(-60.600980900904,-112.321241247773,171.975054964538));
#21760=CARTESIAN_POINT('Ctrl Pts',(-61.7590521391157,-112.103501888271,
173.149682816192));
#21761=CARTESIAN_POINT('Ctrl Pts',(-62.9171233773274,-111.885762528768,
174.324310667846));
#21762=CARTESIAN_POINT('Ctrl Pts',(-62.9071852452935,-111.792540771481,
175.985485236888));
#21763=CARTESIAN_POINT('Ctrl Pts',(-62.8972471132596,-111.699319014194,
177.64665980593));
#21764=CARTESIAN_POINT('Ctrl Pts',(-61.7192996514678,-111.730614854806,
178.821287559284));
#21765=CARTESIAN_POINT('Ctrl Pts',(-60.541352189676,-111.761910695418,179.995915312638));
#21766=CARTESIAN_POINT('Ctrl Pts',(-58.8795994630079,-111.844783409518,
179.995915243129));
#21767=CARTESIAN_POINT('Ctrl Pts',(-57.2178467363399,-111.927656123618,
179.995915173621));
#21768=CARTESIAN_POINT('Ctrl Pts',(-56.0398993722941,-111.958951953809,
178.821287321967));
#21769=CARTESIAN_POINT('Ctrl Pts',(-54.8619520082484,-111.990247784001,
177.646659470313));
#21770=CARTESIAN_POINT('Ctrl Pts',(-54.8520140144483,-111.897026011977,
175.985484901271));
#21771=CARTESIAN_POINT('Ctrl Pts',(-54.8420760206482,-111.803804239954,
174.324310332229));
#21772=CARTESIAN_POINT('Ctrl Pts',(-56.000147356606,-111.586064870031,173.149682578875));
#21773=CARTESIAN_POINT('Ctrl Pts',(-57.1582186925638,-111.368325500108,
171.975054825521));
#21774=CARTESIAN_POINT('Ctrl Pts',(-58.8000952933978,-111.099009256698,
171.97505489503));
#21775=CARTESIAN_POINT('Ctrl Pts',(-60.4419718942318,-110.829693013287,
171.975054964538));
#21776=CARTESIAN_POINT('Ctrl Pts',(-61.6000431324435,-110.611953653785,
173.149682816192));
#21777=CARTESIAN_POINT('Ctrl Pts',(-62.7581143706552,-110.394214294283,
174.324310667846));
#21778=CARTESIAN_POINT('Ctrl Pts',(-62.7481762386213,-110.300992536996,
175.985485236888));
#21779=CARTESIAN_POINT('Ctrl Pts',(-62.7382381065874,-110.207770779709,
177.64665980593));
#21780=CARTESIAN_POINT('Ctrl Pts',(-61.5602906447956,-110.239066620321,
178.821287559284));
#21781=CARTESIAN_POINT('Ctrl Pts',(-60.3823431830037,-110.270362460933,
179.995915312638));
#21782=CARTESIAN_POINT('Ctrl Pts',(-58.7205904563357,-110.353235175032,
179.995915243129));
#21783=CARTESIAN_POINT('Ctrl Pts',(-57.0588377296676,-110.436107889132,
179.995915173621));
#21784=CARTESIAN_POINT('Ctrl Pts',(-55.8808903656219,-110.467403719324,
178.821287321967));
#21785=CARTESIAN_POINT('Ctrl Pts',(-54.7029430015762,-110.498699549515,
177.646659470313));
#21786=CARTESIAN_POINT('Ctrl Pts',(-54.6930050077761,-110.405477777492,
175.985484901271));
#21787=CARTESIAN_POINT('Ctrl Pts',(-54.683067013976,-110.312256005468,174.324310332229));
#21788=CARTESIAN_POINT('Ctrl Pts',(-55.8411383499337,-110.094516635545,
173.149682578875));
#21789=CARTESIAN_POINT('Ctrl Pts',(-56.9992096858915,-109.876777265623,
171.975054825521));
#21790=CARTESIAN_POINT('Ctrl Pts',(-58.6410862867255,-109.607461022212,
171.97505489503));
#21791=CARTESIAN_POINT('Ctrl Pts',(-60.2829628875596,-109.338144778802,
171.975054964538));
#21792=CARTESIAN_POINT('Ctrl Pts',(-61.4410341257713,-109.120405419299,
173.149682816192));
#21793=CARTESIAN_POINT('Ctrl Pts',(-62.599105363983,-108.902666059797,174.324310667846));
#21794=CARTESIAN_POINT('Ctrl Pts',(-62.589167231949,-108.80944430251,175.985485236888));
#21795=CARTESIAN_POINT('Ctrl Pts',(-62.5792290999151,-108.716222545223,
177.64665980593));
#21796=CARTESIAN_POINT('Ctrl Pts',(-61.4012816381233,-108.747518385835,
178.821287559284));
#21797=CARTESIAN_POINT('Ctrl Pts',(-60.2233341763315,-108.778814226447,
179.995915312638));
#21798=CARTESIAN_POINT('Ctrl Pts',(-58.5615814496634,-108.861686940547,
179.995915243129));
#21799=CARTESIAN_POINT('Ctrl Pts',(-56.8998287229954,-108.944559654646,
179.995915173621));
#21800=CARTESIAN_POINT('Ctrl Pts',(-55.7218813589497,-108.975855484838,
178.821287321967));
#21801=CARTESIAN_POINT('Ctrl Pts',(-54.543933994904,-109.00715131503,177.646659470313));
#21802=CARTESIAN_POINT('Ctrl Pts',(-54.5339960011038,-108.913929543006,
175.985484901271));
#21803=CARTESIAN_POINT('Ctrl Pts',(-54.5240580073037,-108.820707770982,
174.324310332229));
#21804=CARTESIAN_POINT('Ctrl Pts',(-55.6821293432615,-108.60296840106,173.149682578875));
#21805=CARTESIAN_POINT('Ctrl Pts',(-56.8402006792193,-108.385229031137,
171.975054825521));
#21806=CARTESIAN_POINT('Ctrl Pts',(-58.4820772800533,-108.115912787727,
171.97505489503));
#21807=CARTESIAN_POINT('Ctrl Pts',(-60.1239538808874,-107.846596544316,
171.975054964538));
#21808=CARTESIAN_POINT('Ctrl Pts',(-61.2820251190991,-107.628857184814,
173.149682816192));
#21809=CARTESIAN_POINT('Ctrl Pts',(-62.4400963573108,-107.411117825312,
174.324310667846));
#21810=CARTESIAN_POINT('Ctrl Pts',(-62.4301582252768,-107.317896068025,
175.985485236888));
#21811=CARTESIAN_POINT('Ctrl Pts',(-62.4202200932429,-107.224674310738,
177.64665980593));
#21812=CARTESIAN_POINT('Ctrl Pts',(-61.2422726314511,-107.25597015135,178.821287559284));
#21813=CARTESIAN_POINT('Ctrl Pts',(-60.0643251696593,-107.287265991962,
179.995915312638));
#21814=CARTESIAN_POINT('Ctrl Pts',(-58.4025724429912,-107.370138706061,
179.995915243129));
#21815=CARTESIAN_POINT('Ctrl Pts',(-56.7408197163232,-107.453011420161,
179.995915173621));
#21816=CARTESIAN_POINT('Ctrl Pts',(-55.5628723522774,-107.484307250352,
178.821287321967));
#21817=CARTESIAN_POINT('Ctrl Pts',(-54.3849249882317,-107.515603080544,
177.646659470313));
#21818=CARTESIAN_POINT('Ctrl Pts',(-54.3749869944316,-107.42238130852,175.985484901271));
#21819=CARTESIAN_POINT('Ctrl Pts',(-54.3650490006315,-107.329159536497,
174.324310332229));
#21820=CARTESIAN_POINT('Ctrl Pts',(-55.5231203365893,-107.111420166574,
173.149682578875));
#21821=CARTESIAN_POINT('Ctrl Pts',(-56.6811916725471,-106.893680796651,
171.975054825521));
#21822=CARTESIAN_POINT('Ctrl Pts',(-58.3230682733811,-106.624364553241,
171.97505489503));
#21823=CARTESIAN_POINT('Ctrl Pts',(-59.9649448742151,-106.355048309831,
171.975054964538));
#21824=CARTESIAN_POINT('Ctrl Pts',(-61.1230161124268,-106.137308950328,
173.149682816192));
#21825=CARTESIAN_POINT('Ctrl Pts',(-62.2810873506385,-105.919569590826,
174.324310667846));
#21826=CARTESIAN_POINT('Ctrl Pts',(-62.2711492186046,-105.826347833539,
175.985485236888));
#21827=CARTESIAN_POINT('Ctrl Pts',(-62.2612110865707,-105.733126076252,
177.64665980593));
#21828=CARTESIAN_POINT('Ctrl Pts',(-61.0832636247789,-105.764421916864,
178.821287559284));
#21829=CARTESIAN_POINT('Ctrl Pts',(-59.9053161629871,-105.795717757476,
179.995915312638));
#21830=CARTESIAN_POINT('Ctrl Pts',(-58.243563436319,-105.878590471576,179.995915243129));
#21831=CARTESIAN_POINT('Ctrl Pts',(-56.5818107096509,-105.961463185675,
179.995915173621));
#21832=CARTESIAN_POINT('Ctrl Pts',(-55.4038633456052,-105.992759015867,
178.821287321967));
#21833=CARTESIAN_POINT('Ctrl Pts',(-54.2259159815595,-106.024054846058,
177.646659470313));
#21834=CARTESIAN_POINT('Ctrl Pts',(-54.2159779877594,-105.930833074035,
175.985484901271));
#21835=CARTESIAN_POINT('Ctrl Pts',(-54.2060399939593,-105.837611302011,
174.324310332229));
#21836=CARTESIAN_POINT('Ctrl Pts',(-55.364111329917,-105.619871932088,173.149682578875));
#21837=CARTESIAN_POINT('Ctrl Pts',(-56.5221826658748,-105.402132562166,
171.975054825521));
#21838=CARTESIAN_POINT('Ctrl Pts',(-58.1640592667089,-105.132816318755,
171.97505489503));
#21839=CARTESIAN_POINT('Ctrl Pts',(-59.8059358675429,-104.863500075345,
171.975054964538));
#21840=CARTESIAN_POINT('Ctrl Pts',(-60.9640071057546,-104.645760715843,
173.149682816192));
#21841=CARTESIAN_POINT('Ctrl Pts',(-62.1220783439663,-104.42802135634,174.324310667846));
#21842=CARTESIAN_POINT('Ctrl Pts',(-62.1121402119324,-104.334799599053,
175.985485236888));
#21843=CARTESIAN_POINT('Ctrl Pts',(-62.1022020798985,-104.241577841766,
177.64665980593));
#21844=CARTESIAN_POINT('Ctrl Pts',(-60.9242546181066,-104.272873682378,
178.821287559284));
#21845=CARTESIAN_POINT('Ctrl Pts',(-59.7463071563148,-104.30416952299,179.995915312638));
#21846=CARTESIAN_POINT('Ctrl Pts',(-58.0845544296468,-104.38704223709,179.995915243129));
#21847=CARTESIAN_POINT('Ctrl Pts',(-56.4228017029787,-104.46991495119,179.995915173621));
#21848=CARTESIAN_POINT('Ctrl Pts',(-55.244854338933,-104.501210781381,178.821287321967));
#21849=CARTESIAN_POINT('Ctrl Pts',(-54.0669069748872,-104.532506611573,
177.646659470313));
#21850=CARTESIAN_POINT('Ctrl Pts',(-54.0569689810871,-104.439284839549,
175.985484901271));
#21851=CARTESIAN_POINT('Ctrl Pts',(-54.0470309872871,-104.346063067526,
174.324310332229));
#21852=CARTESIAN_POINT('Ctrl Pts',(-55.2051023232448,-104.128323697603,
173.149682578875));
#21853=CARTESIAN_POINT('Ctrl Pts',(-56.3631736592026,-103.91058432768,171.975054825521));
#21854=CARTESIAN_POINT('Ctrl Pts',(-58.0050502600366,-103.64126808427,171.97505489503));
#21855=CARTESIAN_POINT('Ctrl Pts',(-59.6469268608707,-103.371951840859,
171.975054964538));
#21856=CARTESIAN_POINT('Ctrl Pts',(-60.8049980990824,-103.154212481357,
173.149682816192));
#21857=CARTESIAN_POINT('Ctrl Pts',(-61.9630693372941,-102.936473121855,
174.324310667846));
#21858=CARTESIAN_POINT('Ctrl Pts',(-61.9531312052601,-102.843251364568,
175.985485236888));
#21859=CARTESIAN_POINT('Ctrl Pts',(-61.9431930732262,-102.750029607281,
177.64665980593));
#21860=CARTESIAN_POINT('Ctrl Pts',(-60.7652456114344,-102.781325447893,
178.821287559284));
#21861=CARTESIAN_POINT('Ctrl Pts',(-59.5872981496426,-102.812621288505,
179.995915312638));
#21862=CARTESIAN_POINT('Ctrl Pts',(-57.9255454229745,-102.895494002604,
179.995915243129));
#21863=CARTESIAN_POINT('Ctrl Pts',(-56.2637926963065,-102.978366716704,
179.995915173621));
#21864=CARTESIAN_POINT('Ctrl Pts',(-55.0858453322607,-103.009662546896,
178.821287321967));
#21865=CARTESIAN_POINT('Ctrl Pts',(-53.907897968215,-103.040958377087,177.646659470313));
#21866=CARTESIAN_POINT('Ctrl Pts',(-53.8979599744149,-102.947736605064,
175.985484901271));
#21867=CARTESIAN_POINT('Ctrl Pts',(-53.8880219806148,-102.85451483304,174.324310332229));
#21868=CARTESIAN_POINT('Ctrl Pts',(-55.0460933165726,-102.636775463117,
173.149682578875));
#21869=CARTESIAN_POINT('Ctrl Pts',(-56.2041646525304,-102.419036093195,
171.975054825521));
#21870=CARTESIAN_POINT('Ctrl Pts',(-57.8460412533644,-102.149719849784,
171.97505489503));
#21871=CARTESIAN_POINT('Ctrl Pts',(-59.4879178541985,-101.880403606374,
171.975054964538));
#21872=CARTESIAN_POINT('Ctrl Pts',(-60.6459890924101,-101.662664246871,
173.149682816192));
#21873=CARTESIAN_POINT('Ctrl Pts',(-61.8040603306218,-101.444924887369,
174.324310667846));
#21874=CARTESIAN_POINT('Ctrl Pts',(-61.7941221985879,-101.351703130082,
175.985485236888));
#21875=CARTESIAN_POINT('Ctrl Pts',(-61.784184066554,-101.258481372795,177.64665980593));
#21876=CARTESIAN_POINT('Ctrl Pts',(-60.6062366047622,-101.289777213407,
178.821287559284));
#21877=CARTESIAN_POINT('Ctrl Pts',(-59.4282891429704,-101.321073054019,
179.995915312638));
#21878=CARTESIAN_POINT('Ctrl Pts',(-57.7665364163023,-101.403945768119,
179.995915243129));
#21879=CARTESIAN_POINT('Ctrl Pts',(-56.1047836896342,-101.486818482218,
179.995915173621));
#21880=CARTESIAN_POINT('Ctrl Pts',(-54.9268363255885,-101.51811431241,178.821287321967));
#21881=CARTESIAN_POINT('Ctrl Pts',(-53.7488889615428,-101.549410142602,
177.646659470313));
#21882=CARTESIAN_POINT('Ctrl Pts',(-53.7389509677427,-101.456188370578,
175.985484901271));
#21883=CARTESIAN_POINT('Ctrl Pts',(-53.7290129739426,-101.362966598554,
174.324310332229));
#21884=CARTESIAN_POINT('Ctrl Pts',(-54.8870843099004,-101.145227228632,
173.149682578875));
#21885=CARTESIAN_POINT('Ctrl Pts',(-56.0451556458581,-100.927487858709,
171.975054825521));
#21886=CARTESIAN_POINT('Ctrl Pts',(-57.6870322466922,-100.658171615299,
171.97505489503));
#21887=CARTESIAN_POINT('Ctrl Pts',(-59.3289088475262,-100.388855371888,
171.975054964538));
#21888=CARTESIAN_POINT('Ctrl Pts',(-60.4869800857379,-100.171116012386,
173.149682816192));
#21889=CARTESIAN_POINT('Ctrl Pts',(-61.6450513239496,-99.9533766528836,
174.324310667846));
#21890=CARTESIAN_POINT('Ctrl Pts',(-61.6351131919157,-99.8601548955965,
175.985485236888));
#21891=CARTESIAN_POINT('Ctrl Pts',(-61.6251750598818,-99.7669331383095,
177.64665980593));
#21892=CARTESIAN_POINT('Ctrl Pts',(-60.44722759809,-99.7982289789215,178.821287559284));
#21893=CARTESIAN_POINT('Ctrl Pts',(-59.2692801362982,-99.8295248195335,
179.995915312638));
#21894=CARTESIAN_POINT('Ctrl Pts',(-57.6075274096301,-99.9123975336331,
179.995915243129));
#21895=CARTESIAN_POINT('Ctrl Pts',(-55.945774682962,-99.9952702477328,179.995915173621));
#21896=CARTESIAN_POINT('Ctrl Pts',(-54.7678273189163,-100.026566077924,
178.821287321967));
#21897=CARTESIAN_POINT('Ctrl Pts',(-53.5898799548706,-100.057861908116,
177.646659470313));
#21898=CARTESIAN_POINT('Ctrl Pts',(-53.5799419610705,-99.9646401360924,
175.985484901271));
#21899=CARTESIAN_POINT('Ctrl Pts',(-53.5700039672704,-99.8714183640688,
174.324310332229));
#21900=CARTESIAN_POINT('Ctrl Pts',(-54.7280753032281,-99.653678994146,173.149682578875));
#21901=CARTESIAN_POINT('Ctrl Pts',(-55.8861466391859,-99.4359396242233,
171.975054825521));
#21902=CARTESIAN_POINT('Ctrl Pts',(-57.5280232400199,-99.1666233808129,
171.97505489503));
#21903=CARTESIAN_POINT('Ctrl Pts',(-59.169899840854,-98.8973071374026,171.975054964538));
#21904=CARTESIAN_POINT('Ctrl Pts',(-60.3279710790657,-98.6795677779003,
173.149682816192));
#21905=CARTESIAN_POINT('Ctrl Pts',(-61.4860423172774,-98.461828418398,174.324310667846));
#21906=CARTESIAN_POINT('Ctrl Pts',(-61.4761041852435,-98.3686066611109,
175.985485236888));
#21907=CARTESIAN_POINT('Ctrl Pts',(-61.4661660532095,-98.2753849038239,
177.64665980593));
#21908=CARTESIAN_POINT('Ctrl Pts',(-60.2882185914177,-98.3066807444359,
178.821287559284));
#21909=CARTESIAN_POINT('Ctrl Pts',(-59.1102711296259,-98.3379765850479,
179.995915312638));
#21910=CARTESIAN_POINT('Ctrl Pts',(-57.4485184029579,-98.4208492991475,
179.995915243129));
#21911=CARTESIAN_POINT('Ctrl Pts',(-55.363467025668,-98.5248321985888,179.995915155915));
#21912=CARTESIAN_POINT('Ctrl Pts',(-54.1610442878665,-98.5449360708601,
178.290118984142));
#21913=CARTESIAN_POINT('Ctrl Pts',(-56.2240123501782,-113.615805207186,
178.813848124531));
#21914=CARTESIAN_POINT('Ctrl Pts',(-55.0491290403307,-113.646774388729,
177.642301689606));
#21915=CARTESIAN_POINT('Ctrl Pts',(-55.0391910463492,-113.553552616725,
175.985484901711));
#21916=CARTESIAN_POINT('Ctrl Pts',(-55.0292530523678,-113.46033084472,174.328668113817));
#21917=CARTESIAN_POINT('Ctrl Pts',(-56.184260333871,-113.242918123473,173.157121776934));
#21918=CARTESIAN_POINT('Ctrl Pts',(-57.3392676153741,-113.025505402226,
171.985575440051));
#21919=CARTESIAN_POINT('Ctrl Pts',(-58.976810989024,-112.756651109783,171.985575509377));
#21920=CARTESIAN_POINT('Ctrl Pts',(-60.6143543626737,-112.487796817341,
171.985575578703));
#21921=CARTESIAN_POINT('Ctrl Pts',(-61.7693615466873,-112.270384106486,
173.157122013628));
#21922=CARTESIAN_POINT('Ctrl Pts',(-62.9243687307007,-112.052971395632,
174.328668448553));
#21923=CARTESIAN_POINT('Ctrl Pts',(-62.9144305988482,-111.959749638326,
175.985485236448));
#21924=CARTESIAN_POINT('Ctrl Pts',(-62.9044924669955,-111.86652788102,177.642302024342));
#21925=CARTESIAN_POINT('Ctrl Pts',(-61.7296090596583,-111.897497072956,
178.813848361225));
#21926=CARTESIAN_POINT('Ctrl Pts',(-60.5547256523212,-111.928466264893,
179.985394698108));
#21927=CARTESIAN_POINT('Ctrl Pts',(-58.8973061528373,-112.010877028025,
179.985394628782));
#21928=CARTESIAN_POINT('Ctrl Pts',(-57.2398866533535,-112.093287791156,
179.985394559456));
#21929=CARTESIAN_POINT('Ctrl Pts',(-56.0650033435059,-112.1242569727,178.813848124531));
#21930=CARTESIAN_POINT('Ctrl Pts',(-54.8901200336584,-112.155226154243,
177.642301689606));
#21931=CARTESIAN_POINT('Ctrl Pts',(-54.880182039677,-112.062004382239,175.985484901711));
#21932=CARTESIAN_POINT('Ctrl Pts',(-54.8702440456956,-111.968782610235,
174.328668113817));
#21933=CARTESIAN_POINT('Ctrl Pts',(-56.0252513271988,-111.751369888988,
173.157121776934));
#21934=CARTESIAN_POINT('Ctrl Pts',(-57.1802586087019,-111.53395716774,171.985575440051));
#21935=CARTESIAN_POINT('Ctrl Pts',(-58.8178019823517,-111.265102875298,
171.985575509377));
#21936=CARTESIAN_POINT('Ctrl Pts',(-60.4553453560015,-110.996248582855,
171.985575578703));
#21937=CARTESIAN_POINT('Ctrl Pts',(-61.610352540015,-110.778835872001,173.157122013628));
#21938=CARTESIAN_POINT('Ctrl Pts',(-62.7653597240285,-110.561423161147,
174.328668448553));
#21939=CARTESIAN_POINT('Ctrl Pts',(-62.7554215921759,-110.46820140384,175.985485236448));
#21940=CARTESIAN_POINT('Ctrl Pts',(-62.7454834603233,-110.374979646534,
177.642302024342));
#21941=CARTESIAN_POINT('Ctrl Pts',(-61.5706000529861,-110.40594883847,178.813848361225));
#21942=CARTESIAN_POINT('Ctrl Pts',(-60.3957166456489,-110.436918030407,
179.985394698108));
#21943=CARTESIAN_POINT('Ctrl Pts',(-58.7382971461651,-110.519328793539,
179.985394628782));
#21944=CARTESIAN_POINT('Ctrl Pts',(-57.0808776466813,-110.601739556671,
179.985394559456));
#21945=CARTESIAN_POINT('Ctrl Pts',(-55.9059943368337,-110.632708738214,
178.813848124531));
#21946=CARTESIAN_POINT('Ctrl Pts',(-54.7311110269862,-110.663677919758,
177.642301689606));
#21947=CARTESIAN_POINT('Ctrl Pts',(-54.7211730330048,-110.570456147754,
175.985484901711));
#21948=CARTESIAN_POINT('Ctrl Pts',(-54.7112350390234,-110.477234375749,
174.328668113817));
#21949=CARTESIAN_POINT('Ctrl Pts',(-55.8662423205265,-110.259821654502,
173.157121776934));
#21950=CARTESIAN_POINT('Ctrl Pts',(-57.0212496020297,-110.042408933255,
171.985575440051));
#21951=CARTESIAN_POINT('Ctrl Pts',(-58.6587929756795,-109.773554640812,
171.985575509377));
#21952=CARTESIAN_POINT('Ctrl Pts',(-60.2963363493293,-109.504700348369,
171.985575578703));
#21953=CARTESIAN_POINT('Ctrl Pts',(-61.4513435333428,-109.287287637515,
173.157122013628));
#21954=CARTESIAN_POINT('Ctrl Pts',(-62.6063507173563,-109.069874926661,
174.328668448553));
#21955=CARTESIAN_POINT('Ctrl Pts',(-62.5964125855037,-108.976653169355,
175.985485236448));
#21956=CARTESIAN_POINT('Ctrl Pts',(-62.5864744536511,-108.883431412048,
177.642302024342));
#21957=CARTESIAN_POINT('Ctrl Pts',(-61.4115910463139,-108.914400603985,
178.813848361225));
#21958=CARTESIAN_POINT('Ctrl Pts',(-60.2367076389767,-108.945369795921,
179.985394698108));
#21959=CARTESIAN_POINT('Ctrl Pts',(-58.5792881394929,-109.027780559053,
179.985394628782));
#21960=CARTESIAN_POINT('Ctrl Pts',(-56.921868640009,-109.110191322185,179.985394559456));
#21961=CARTESIAN_POINT('Ctrl Pts',(-55.7469853301615,-109.141160503729,
178.813848124531));
#21962=CARTESIAN_POINT('Ctrl Pts',(-54.572102020314,-109.172129685272,177.642301689606));
#21963=CARTESIAN_POINT('Ctrl Pts',(-54.5621640263326,-109.078907913268,
175.985484901711));
#21964=CARTESIAN_POINT('Ctrl Pts',(-54.5522260323511,-108.985686141264,
174.328668113817));
#21965=CARTESIAN_POINT('Ctrl Pts',(-55.7072333138543,-108.768273420016,
173.157121776934));
#21966=CARTESIAN_POINT('Ctrl Pts',(-56.8622405953575,-108.550860698769,
171.985575440051));
#21967=CARTESIAN_POINT('Ctrl Pts',(-58.4997839690073,-108.282006406326,
171.985575509377));
#21968=CARTESIAN_POINT('Ctrl Pts',(-60.1373273426571,-108.013152113884,
171.985575578703));
#21969=CARTESIAN_POINT('Ctrl Pts',(-61.2923345266706,-107.79573940303,173.157122013628));
#21970=CARTESIAN_POINT('Ctrl Pts',(-62.4473417106841,-107.578326692175,
174.328668448553));
#21971=CARTESIAN_POINT('Ctrl Pts',(-62.4374035788315,-107.485104934869,
175.985485236448));
#21972=CARTESIAN_POINT('Ctrl Pts',(-62.4274654469789,-107.391883177563,
177.642302024342));
#21973=CARTESIAN_POINT('Ctrl Pts',(-61.2525820396417,-107.422852369499,
178.813848361225));
#21974=CARTESIAN_POINT('Ctrl Pts',(-60.0776986323045,-107.453821561436,
179.985394698108));
#21975=CARTESIAN_POINT('Ctrl Pts',(-58.4202791328206,-107.536232324568,
179.985394628782));
#21976=CARTESIAN_POINT('Ctrl Pts',(-56.7628596333368,-107.6186430877,179.985394559456));
#21977=CARTESIAN_POINT('Ctrl Pts',(-55.5879763234893,-107.649612269243,
178.813848124531));
#21978=CARTESIAN_POINT('Ctrl Pts',(-54.4130930136417,-107.680581450787,
177.642301689606));
#21979=CARTESIAN_POINT('Ctrl Pts',(-54.4031550196603,-107.587359678782,
175.985484901711));
#21980=CARTESIAN_POINT('Ctrl Pts',(-54.3932170256789,-107.494137906778,
174.328668113817));
#21981=CARTESIAN_POINT('Ctrl Pts',(-55.5482243071821,-107.276725185531,
173.157121776934));
#21982=CARTESIAN_POINT('Ctrl Pts',(-56.7032315886852,-107.059312464284,
171.985575440051));
#21983=CARTESIAN_POINT('Ctrl Pts',(-58.340774962335,-106.790458171841,171.985575509377));
#21984=CARTESIAN_POINT('Ctrl Pts',(-59.9783183359848,-106.521603879398,
171.985575578703));
#21985=CARTESIAN_POINT('Ctrl Pts',(-61.1333255199984,-106.304191168544,
173.157122013628));
#21986=CARTESIAN_POINT('Ctrl Pts',(-62.2883327040119,-106.08677845769,174.328668448553));
#21987=CARTESIAN_POINT('Ctrl Pts',(-62.2783945721593,-105.993556700383,
175.985485236448));
#21988=CARTESIAN_POINT('Ctrl Pts',(-62.2684564403066,-105.900334943077,
177.642302024342));
#21989=CARTESIAN_POINT('Ctrl Pts',(-61.0935730329694,-105.931304135014,
178.813848361225));
#21990=CARTESIAN_POINT('Ctrl Pts',(-59.9186896256322,-105.96227332695,179.985394698108));
#21991=CARTESIAN_POINT('Ctrl Pts',(-58.2612701261484,-106.044684090082,
179.985394628782));
#21992=CARTESIAN_POINT('Ctrl Pts',(-56.6038506266646,-106.127094853214,
179.985394559456));
#21993=CARTESIAN_POINT('Ctrl Pts',(-55.4289673168171,-106.158064034758,
178.813848124531));
#21994=CARTESIAN_POINT('Ctrl Pts',(-54.2540840069695,-106.189033216301,
177.642301689606));
#21995=CARTESIAN_POINT('Ctrl Pts',(-54.2441460129881,-106.095811444297,
175.985484901711));
#21996=CARTESIAN_POINT('Ctrl Pts',(-54.2342080190067,-106.002589672292,
174.328668113817));
#21997=CARTESIAN_POINT('Ctrl Pts',(-55.3892153005098,-105.785176951045,
173.157121776934));
#21998=CARTESIAN_POINT('Ctrl Pts',(-56.544222582013,-105.567764229798,171.985575440051));
#21999=CARTESIAN_POINT('Ctrl Pts',(-58.1817659556628,-105.298909937355,
171.985575509377));
#22000=CARTESIAN_POINT('Ctrl Pts',(-59.8193093293126,-105.030055644913,
171.985575578703));
#22001=CARTESIAN_POINT('Ctrl Pts',(-60.9743165133261,-104.812642934058,
173.157122013628));
#22002=CARTESIAN_POINT('Ctrl Pts',(-62.1293236973396,-104.595230223204,
174.328668448553));
#22003=CARTESIAN_POINT('Ctrl Pts',(-62.119385565487,-104.502008465898,175.985485236448));
#22004=CARTESIAN_POINT('Ctrl Pts',(-62.1094474336344,-104.408786708592,
177.642302024342));
#22005=CARTESIAN_POINT('Ctrl Pts',(-60.9345640262972,-104.439755900528,
178.813848361225));
#22006=CARTESIAN_POINT('Ctrl Pts',(-59.75968061896,-104.470725092465,179.985394698108));
#22007=CARTESIAN_POINT('Ctrl Pts',(-58.1022611194762,-104.553135855597,
179.985394628782));
#22008=CARTESIAN_POINT('Ctrl Pts',(-56.4448416199923,-104.635546618729,
179.985394559456));
#22009=CARTESIAN_POINT('Ctrl Pts',(-55.2699583101448,-104.666515800272,
178.813848124531));
#22010=CARTESIAN_POINT('Ctrl Pts',(-54.0950750002973,-104.697484981815,
177.642301689606));
#22011=CARTESIAN_POINT('Ctrl Pts',(-54.0851370063159,-104.604263209811,
175.985484901711));
#22012=CARTESIAN_POINT('Ctrl Pts',(-54.0751990123344,-104.511041437807,
174.328668113817));
#22013=CARTESIAN_POINT('Ctrl Pts',(-55.2302062938376,-104.29362871656,173.157121776934));
#22014=CARTESIAN_POINT('Ctrl Pts',(-56.3852135753408,-104.076215995312,
171.985575440051));
#22015=CARTESIAN_POINT('Ctrl Pts',(-58.0227569489906,-103.80736170287,171.985575509377));
#22016=CARTESIAN_POINT('Ctrl Pts',(-59.6603003226404,-103.538507410427,
171.985575578703));
#22017=CARTESIAN_POINT('Ctrl Pts',(-60.8153075066539,-103.321094699573,
173.157122013628));
#22018=CARTESIAN_POINT('Ctrl Pts',(-61.9703146906674,-103.103681988719,
174.328668448553));
#22019=CARTESIAN_POINT('Ctrl Pts',(-61.9603765588148,-103.010460231412,
175.985485236448));
#22020=CARTESIAN_POINT('Ctrl Pts',(-61.9504384269622,-102.917238474106,
177.642302024342));
#22021=CARTESIAN_POINT('Ctrl Pts',(-60.775555019625,-102.948207666042,178.813848361225));
#22022=CARTESIAN_POINT('Ctrl Pts',(-59.6006716122878,-102.979176857979,
179.985394698108));
#22023=CARTESIAN_POINT('Ctrl Pts',(-57.943252112804,-103.061587621111,179.985394628782));
#22024=CARTESIAN_POINT('Ctrl Pts',(-56.2858326133201,-103.143998384243,
179.985394559456));
#22025=CARTESIAN_POINT('Ctrl Pts',(-55.1109493034726,-103.174967565786,
178.813848124531));
#22026=CARTESIAN_POINT('Ctrl Pts',(-53.936065993625,-103.20593674733,177.642301689606));
#22027=CARTESIAN_POINT('Ctrl Pts',(-53.9261279996436,-103.112714975326,
175.985484901711));
#22028=CARTESIAN_POINT('Ctrl Pts',(-53.9161900056622,-103.019493203321,
174.328668113817));
#22029=CARTESIAN_POINT('Ctrl Pts',(-55.0711972871654,-102.802080482074,
173.157121776934));
#22030=CARTESIAN_POINT('Ctrl Pts',(-56.2262045686686,-102.584667760827,
171.985575440051));
#22031=CARTESIAN_POINT('Ctrl Pts',(-57.8637479423184,-102.315813468384,
171.985575509377));
#22032=CARTESIAN_POINT('Ctrl Pts',(-59.5012913159682,-102.046959175941,
171.985575578703));
#22033=CARTESIAN_POINT('Ctrl Pts',(-60.6562984999817,-101.829546465087,
173.157122013628));
#22034=CARTESIAN_POINT('Ctrl Pts',(-61.8113056839952,-101.612133754233,
174.328668448553));
#22035=CARTESIAN_POINT('Ctrl Pts',(-61.8013675521426,-101.518911996927,
175.985485236448));
#22036=CARTESIAN_POINT('Ctrl Pts',(-61.79142942029,-101.42569023962,177.642302024342));
#22037=CARTESIAN_POINT('Ctrl Pts',(-60.6165460129528,-101.456659431557,
178.813848361225));
#22038=CARTESIAN_POINT('Ctrl Pts',(-59.4416626056156,-101.487628623493,
179.985394698108));
#22039=CARTESIAN_POINT('Ctrl Pts',(-57.7842431061317,-101.570039386625,
179.985394628782));
#22040=CARTESIAN_POINT('Ctrl Pts',(-56.1268236066479,-101.652450149757,
179.985394559456));
#22041=CARTESIAN_POINT('Ctrl Pts',(-54.9519402968004,-101.683419331301,
178.813848124531));
#22042=CARTESIAN_POINT('Ctrl Pts',(-53.7770569869528,-101.714388512844,
177.642301689606));
#22043=CARTESIAN_POINT('Ctrl Pts',(-53.7671189929714,-101.62116674084,175.985484901711));
#22044=CARTESIAN_POINT('Ctrl Pts',(-53.75718099899,-101.527944968836,174.328668113817));
#22045=CARTESIAN_POINT('Ctrl Pts',(-54.9121882804932,-101.310532247588,
173.157121776934));
#22046=CARTESIAN_POINT('Ctrl Pts',(-56.0671955619963,-101.093119526341,
171.985575440051));
#22047=CARTESIAN_POINT('Ctrl Pts',(-57.7047389356461,-100.824265233898,
171.985575509377));
#22048=CARTESIAN_POINT('Ctrl Pts',(-59.3422823092959,-100.555410941456,
171.985575578703));
#22049=CARTESIAN_POINT('Ctrl Pts',(-60.4972894933094,-100.337998230602,
173.157122013628));
#22050=CARTESIAN_POINT('Ctrl Pts',(-61.652296677323,-100.120585519747,174.328668448553));
#22051=CARTESIAN_POINT('Ctrl Pts',(-61.6423585454703,-100.027363762441,
175.985485236448));
#22052=CARTESIAN_POINT('Ctrl Pts',(-61.6324204136177,-99.9341420051347,
177.642302024342));
#22053=CARTESIAN_POINT('Ctrl Pts',(-60.4575370062805,-99.9651111970713,
178.813848361225));
#22054=CARTESIAN_POINT('Ctrl Pts',(-59.2826535989433,-99.9960803890078,
179.985394698108));
#22055=CARTESIAN_POINT('Ctrl Pts',(-57.6252340994595,-100.07849115214,179.985394628782));
#22056=CARTESIAN_POINT('Ctrl Pts',(-55.9678145999757,-100.160901915272,
179.985394559456));
#22057=CARTESIAN_POINT('Ctrl Pts',(-54.7929312901281,-100.191871096815,
178.813848124531));
#22058=CARTESIAN_POINT('Ctrl Pts',(-53.6180479802806,-100.222840278359,
177.642301689606));
#22059=CARTESIAN_POINT('Ctrl Pts',(-53.6081099862992,-100.129618506354,
175.985484901711));
#22060=CARTESIAN_POINT('Ctrl Pts',(-53.5981719923178,-100.03639673435,174.328668113817));
#22061=CARTESIAN_POINT('Ctrl Pts',(-54.7531792738209,-99.8189840131027,
173.157121776934));
#22062=CARTESIAN_POINT('Ctrl Pts',(-55.9081865553241,-99.6015712918555,
171.985575440051));
#22063=CARTESIAN_POINT('Ctrl Pts',(-57.5457299289739,-99.3327169994129,
171.985575509377));
#22064=CARTESIAN_POINT('Ctrl Pts',(-59.1832733026237,-99.0638627069702,
171.985575578703));
#22065=CARTESIAN_POINT('Ctrl Pts',(-60.3382804866372,-98.846449996116,173.157122013628));
#22066=CARTESIAN_POINT('Ctrl Pts',(-61.4932876706507,-98.6290372852619,
174.328668448553));
#22067=CARTESIAN_POINT('Ctrl Pts',(-61.4833495387981,-98.5358155279555,
175.985485236448));
#22068=CARTESIAN_POINT('Ctrl Pts',(-61.4734114069455,-98.4425937706491,
177.642302024342));
#22069=CARTESIAN_POINT('Ctrl Pts',(-60.2985279996083,-98.4735629625857,
178.813848361225));
#22070=CARTESIAN_POINT('Ctrl Pts',(-59.1236445922711,-98.5045321545222,
179.985394698108));
#22071=CARTESIAN_POINT('Ctrl Pts',(-57.4662250927873,-98.5869429176541,
179.985394628782));
#22072=CARTESIAN_POINT('Ctrl Pts',(-55.3866107466295,-98.6903461932525,
179.985394541796));
#22073=CARTESIAN_POINT('Ctrl Pts',(-54.187312453289,-98.7101169788701,178.284073207609));
#22074=CARTESIAN_POINT('Origin',(-57.4141964578263,-98.1510622392946,175.991014745935));
#22075=CARTESIAN_POINT('Origin',(-54.6017060172855,-98.4508925102076,178.819441752331));
#22076=CARTESIAN_POINT('Ctrl Pts',(-56.1707931031902,-113.117197303651,
178.813912075476));
#22077=CARTESIAN_POINT('Ctrl Pts',(-54.9958834532485,-113.148169293224,
177.6423391512));
#22078=CARTESIAN_POINT('Ctrl Pts',(-54.9859454592686,-113.05494752122,175.985484901707));
#22079=CARTESIAN_POINT('Ctrl Pts',(-54.9760074652888,-112.961725749215,
174.328630652215));
#22080=CARTESIAN_POINT('Ctrl Pts',(-56.1310410868884,-112.744310219938,
173.157057825983));
#22081=CARTESIAN_POINT('Ctrl Pts',(-57.286074708488,-112.52689469066,171.985484999752));
#22082=CARTESIAN_POINT('Ctrl Pts',(-58.9236553326578,-112.258036427063,
171.985485069079));
#22083=CARTESIAN_POINT('Ctrl Pts',(-60.5612359568277,-111.989178163466,
171.985485138407));
#22084=CARTESIAN_POINT('Ctrl Pts',(-61.7162694809355,-111.771762644582,
173.157058062683));
#22085=CARTESIAN_POINT('Ctrl Pts',(-62.8713030050432,-111.554347125698,
174.328630986959));
#22086=CARTESIAN_POINT('Ctrl Pts',(-62.861364873189,-111.461125368392,175.985485236451));
#22087=CARTESIAN_POINT('Ctrl Pts',(-62.8514267413349,-111.367903611086,
177.642339485944));
#22088=CARTESIAN_POINT('Ctrl Pts',(-61.6765169939012,-111.398875611052,
178.813912312176));
#22089=CARTESIAN_POINT('Ctrl Pts',(-60.5016072464676,-111.429847611019,
179.985485138407));
#22090=CARTESIAN_POINT('Ctrl Pts',(-58.8441504964637,-111.512262345305,
179.985485069079));
#22091=CARTESIAN_POINT('Ctrl Pts',(-57.1866937464598,-111.594677079592,
179.985484999752));
#22092=CARTESIAN_POINT('Ctrl Pts',(-56.011784096518,-111.625649069165,178.813912075476));
#22093=CARTESIAN_POINT('Ctrl Pts',(-54.8368744465763,-111.656621058739,
177.6423391512));
#22094=CARTESIAN_POINT('Ctrl Pts',(-54.8269364525964,-111.563399286734,
175.985484901707));
#22095=CARTESIAN_POINT('Ctrl Pts',(-54.8169984586165,-111.47017751473,174.328630652215));
#22096=CARTESIAN_POINT('Ctrl Pts',(-55.9720320802161,-111.252761985452,
173.157057825983));
#22097=CARTESIAN_POINT('Ctrl Pts',(-57.1270657018158,-111.035346456175,
171.985484999752));
#22098=CARTESIAN_POINT('Ctrl Pts',(-58.7646463259856,-110.766488192578,
171.985485069079));
#22099=CARTESIAN_POINT('Ctrl Pts',(-60.4022269501555,-110.497629928981,
171.985485138407));
#22100=CARTESIAN_POINT('Ctrl Pts',(-61.5572604742632,-110.280214410097,
173.157058062683));
#22101=CARTESIAN_POINT('Ctrl Pts',(-62.712293998371,-110.062798891212,174.328630986959));
#22102=CARTESIAN_POINT('Ctrl Pts',(-62.7023558665168,-109.969577133906,
175.985485236451));
#22103=CARTESIAN_POINT('Ctrl Pts',(-62.6924177346626,-109.8763553766,177.642339485944));
#22104=CARTESIAN_POINT('Ctrl Pts',(-61.517507987229,-109.907327376567,178.813912312176));
#22105=CARTESIAN_POINT('Ctrl Pts',(-60.3425982397954,-109.938299376534,
179.985485138407));
#22106=CARTESIAN_POINT('Ctrl Pts',(-58.6851414897915,-110.02071411082,179.985485069079));
#22107=CARTESIAN_POINT('Ctrl Pts',(-57.0276847397876,-110.103128845106,
179.985484999752));
#22108=CARTESIAN_POINT('Ctrl Pts',(-55.8527750898458,-110.13410083468,178.813912075476));
#22109=CARTESIAN_POINT('Ctrl Pts',(-54.677865439904,-110.165072824253,177.6423391512));
#22110=CARTESIAN_POINT('Ctrl Pts',(-54.6679274459242,-110.071851052249,
175.985484901707));
#22111=CARTESIAN_POINT('Ctrl Pts',(-54.6579894519443,-109.978629280244,
174.328630652215));
#22112=CARTESIAN_POINT('Ctrl Pts',(-55.8130230735439,-109.761213750967,
173.157057825983));
#22113=CARTESIAN_POINT('Ctrl Pts',(-56.9680566951435,-109.543798221689,
171.985484999752));
#22114=CARTESIAN_POINT('Ctrl Pts',(-58.6056373193134,-109.274939958092,
171.985485069079));
#22115=CARTESIAN_POINT('Ctrl Pts',(-60.2432179434833,-109.006081694495,
171.985485138407));
#22116=CARTESIAN_POINT('Ctrl Pts',(-61.398251467591,-108.788666175611,173.157058062683));
#22117=CARTESIAN_POINT('Ctrl Pts',(-62.5532849916988,-108.571250656727,
174.328630986959));
#22118=CARTESIAN_POINT('Ctrl Pts',(-62.5433468598446,-108.478028899421,
175.985485236451));
#22119=CARTESIAN_POINT('Ctrl Pts',(-62.5334087279904,-108.384807142114,
177.642339485944));
#22120=CARTESIAN_POINT('Ctrl Pts',(-61.3584989805568,-108.415779142081,
178.813912312176));
#22121=CARTESIAN_POINT('Ctrl Pts',(-60.1835892331231,-108.446751142048,
179.985485138407));
#22122=CARTESIAN_POINT('Ctrl Pts',(-58.5261324831192,-108.529165876334,
179.985485069079));
#22123=CARTESIAN_POINT('Ctrl Pts',(-56.8686757331153,-108.611580610621,
179.985484999752));
#22124=CARTESIAN_POINT('Ctrl Pts',(-55.6937660831736,-108.642552600194,
178.813912075476));
#22125=CARTESIAN_POINT('Ctrl Pts',(-54.5188564332318,-108.673524589768,
177.6423391512));
#22126=CARTESIAN_POINT('Ctrl Pts',(-54.5089184392519,-108.580302817763,
175.985484901707));
#22127=CARTESIAN_POINT('Ctrl Pts',(-54.4989804452721,-108.487081045759,
174.328630652215));
#22128=CARTESIAN_POINT('Ctrl Pts',(-55.6540140668717,-108.269665516481,
173.157057825983));
#22129=CARTESIAN_POINT('Ctrl Pts',(-56.8090476884713,-108.052249987204,
171.985484999752));
#22130=CARTESIAN_POINT('Ctrl Pts',(-58.4466283126412,-107.783391723607,
171.985485069079));
#22131=CARTESIAN_POINT('Ctrl Pts',(-60.084208936811,-107.51453346001,171.985485138407));
#22132=CARTESIAN_POINT('Ctrl Pts',(-61.2392424609188,-107.297117941125,
173.157058062683));
#22133=CARTESIAN_POINT('Ctrl Pts',(-62.3942759850265,-107.079702422241,
174.328630986959));
#22134=CARTESIAN_POINT('Ctrl Pts',(-62.3843378531723,-106.986480664935,
175.985485236451));
#22135=CARTESIAN_POINT('Ctrl Pts',(-62.3743997213182,-106.893258907629,
177.642339485944));
#22136=CARTESIAN_POINT('Ctrl Pts',(-61.1994899738845,-106.924230907596,
178.813912312176));
#22137=CARTESIAN_POINT('Ctrl Pts',(-60.0245802264509,-106.955202907562,
179.985485138407));
#22138=CARTESIAN_POINT('Ctrl Pts',(-58.367123476447,-107.037617641849,179.985485069079));
#22139=CARTESIAN_POINT('Ctrl Pts',(-56.7096667264431,-107.120032376135,
179.985484999752));
#22140=CARTESIAN_POINT('Ctrl Pts',(-55.5347570765013,-107.151004365708,
178.813912075476));
#22141=CARTESIAN_POINT('Ctrl Pts',(-54.3598474265596,-107.181976355282,
177.6423391512));
#22142=CARTESIAN_POINT('Ctrl Pts',(-54.3499094325797,-107.088754583277,
175.985484901707));
#22143=CARTESIAN_POINT('Ctrl Pts',(-54.3399714385998,-106.995532811273,
174.328630652215));
#22144=CARTESIAN_POINT('Ctrl Pts',(-55.4950050601995,-106.778117281995,
173.157057825983));
#22145=CARTESIAN_POINT('Ctrl Pts',(-56.6500386817991,-106.560701752718,
171.985484999752));
#22146=CARTESIAN_POINT('Ctrl Pts',(-58.2876193059689,-106.291843489121,
171.985485069079));
#22147=CARTESIAN_POINT('Ctrl Pts',(-59.9251999301388,-106.022985225524,
171.985485138407));
#22148=CARTESIAN_POINT('Ctrl Pts',(-61.0802334542465,-105.80556970664,173.157058062683));
#22149=CARTESIAN_POINT('Ctrl Pts',(-62.2352669783543,-105.588154187756,
174.328630986959));
#22150=CARTESIAN_POINT('Ctrl Pts',(-62.2253288465001,-105.494932430449,
175.985485236451));
#22151=CARTESIAN_POINT('Ctrl Pts',(-62.2153907146459,-105.401710673143,
177.642339485944));
#22152=CARTESIAN_POINT('Ctrl Pts',(-61.0404809672123,-105.43268267311,178.813912312176));
#22153=CARTESIAN_POINT('Ctrl Pts',(-59.8655712197787,-105.463654673077,
179.985485138407));
#22154=CARTESIAN_POINT('Ctrl Pts',(-58.2081144697748,-105.546069407363,
179.985485069079));
#22155=CARTESIAN_POINT('Ctrl Pts',(-56.5506577197709,-105.628484141649,
179.985484999752));
#22156=CARTESIAN_POINT('Ctrl Pts',(-55.3757480698291,-105.659456131223,
178.813912075476));
#22157=CARTESIAN_POINT('Ctrl Pts',(-54.2008384198873,-105.690428120796,
177.6423391512));
#22158=CARTESIAN_POINT('Ctrl Pts',(-54.1909004259075,-105.597206348792,
175.985484901707));
#22159=CARTESIAN_POINT('Ctrl Pts',(-54.1809624319276,-105.503984576787,
174.328630652215));
#22160=CARTESIAN_POINT('Ctrl Pts',(-55.3359960535272,-105.28656904751,173.157057825983));
#22161=CARTESIAN_POINT('Ctrl Pts',(-56.4910296751268,-105.069153518232,
171.985484999752));
#22162=CARTESIAN_POINT('Ctrl Pts',(-58.1286102992967,-104.800295254635,
171.985485069079));
#22163=CARTESIAN_POINT('Ctrl Pts',(-59.7661909234666,-104.531436991038,
171.985485138407));
#22164=CARTESIAN_POINT('Ctrl Pts',(-60.9212244475743,-104.314021472154,
173.157058062683));
#22165=CARTESIAN_POINT('Ctrl Pts',(-62.0762579716821,-104.09660595327,174.328630986959));
#22166=CARTESIAN_POINT('Ctrl Pts',(-62.0663198398279,-104.003384195964,
175.985485236451));
#22167=CARTESIAN_POINT('Ctrl Pts',(-62.0563817079737,-103.910162438658,
177.642339485944));
#22168=CARTESIAN_POINT('Ctrl Pts',(-60.8814719605401,-103.941134438624,
178.813912312176));
#22169=CARTESIAN_POINT('Ctrl Pts',(-59.7065622131064,-103.972106438591,
179.985485138407));
#22170=CARTESIAN_POINT('Ctrl Pts',(-58.0491054631025,-104.054521172878,
179.985485069079));
#22171=CARTESIAN_POINT('Ctrl Pts',(-56.3916487130987,-104.136935907164,
179.985484999752));
#22172=CARTESIAN_POINT('Ctrl Pts',(-55.2167390631569,-104.167907896737,
178.813912075476));
#22173=CARTESIAN_POINT('Ctrl Pts',(-54.0418294132151,-104.198879886311,
177.6423391512));
#22174=CARTESIAN_POINT('Ctrl Pts',(-54.0318914192353,-104.105658114306,
175.985484901707));
#22175=CARTESIAN_POINT('Ctrl Pts',(-54.0219534252554,-104.012436342302,
174.328630652215));
#22176=CARTESIAN_POINT('Ctrl Pts',(-55.176987046855,-103.795020813024,173.157057825983));
#22177=CARTESIAN_POINT('Ctrl Pts',(-56.3320206684546,-103.577605283747,
171.985484999752));
#22178=CARTESIAN_POINT('Ctrl Pts',(-57.9696012926245,-103.30874702015,171.985485069079));
#22179=CARTESIAN_POINT('Ctrl Pts',(-59.6071819167943,-103.039888756553,
171.985485138407));
#22180=CARTESIAN_POINT('Ctrl Pts',(-60.7622154409021,-102.822473237669,
173.157058062683));
#22181=CARTESIAN_POINT('Ctrl Pts',(-61.9172489650099,-102.605057718784,
174.328630986959));
#22182=CARTESIAN_POINT('Ctrl Pts',(-61.9073108331557,-102.511835961478,
175.985485236451));
#22183=CARTESIAN_POINT('Ctrl Pts',(-61.8973727013015,-102.418614204172,
177.642339485944));
#22184=CARTESIAN_POINT('Ctrl Pts',(-60.7224629538678,-102.449586204139,
178.813912312176));
#22185=CARTESIAN_POINT('Ctrl Pts',(-59.5475532064342,-102.480558204106,
179.985485138407));
#22186=CARTESIAN_POINT('Ctrl Pts',(-57.8900964564303,-102.562972938392,
179.985485069079));
#22187=CARTESIAN_POINT('Ctrl Pts',(-56.2326397064264,-102.645387672678,
179.985484999752));
#22188=CARTESIAN_POINT('Ctrl Pts',(-55.0577300564847,-102.676359662252,
178.813912075476));
#22189=CARTESIAN_POINT('Ctrl Pts',(-53.8828204065429,-102.707331651825,
177.6423391512));
#22190=CARTESIAN_POINT('Ctrl Pts',(-53.872882412563,-102.614109879821,175.985484901707));
#22191=CARTESIAN_POINT('Ctrl Pts',(-53.8629444185832,-102.520888107816,
174.328630652215));
#22192=CARTESIAN_POINT('Ctrl Pts',(-55.0179780401828,-102.303472578539,
173.157057825983));
#22193=CARTESIAN_POINT('Ctrl Pts',(-56.1730116617824,-102.086057049261,
171.985484999752));
#22194=CARTESIAN_POINT('Ctrl Pts',(-57.8105922859523,-101.817198785664,
171.985485069079));
#22195=CARTESIAN_POINT('Ctrl Pts',(-59.4481729101221,-101.548340522067,
171.985485138407));
#22196=CARTESIAN_POINT('Ctrl Pts',(-60.6032064342299,-101.330925003183,
173.157058062683));
#22197=CARTESIAN_POINT('Ctrl Pts',(-61.7582399583376,-101.113509484299,
174.328630986959));
#22198=CARTESIAN_POINT('Ctrl Pts',(-61.7483018264834,-101.020287726993,
175.985485236451));
#22199=CARTESIAN_POINT('Ctrl Pts',(-61.7383636946293,-100.927065969686,
177.642339485944));
#22200=CARTESIAN_POINT('Ctrl Pts',(-60.5634539471956,-100.958037969653,
178.813912312176));
#22201=CARTESIAN_POINT('Ctrl Pts',(-59.388544199762,-100.98900996962,179.985485138407));
#22202=CARTESIAN_POINT('Ctrl Pts',(-57.7310874497581,-101.071424703906,
179.985485069079));
#22203=CARTESIAN_POINT('Ctrl Pts',(-56.0736306997542,-101.153839438193,
179.985484999752));
#22204=CARTESIAN_POINT('Ctrl Pts',(-54.8987210498124,-101.184811427766,
178.813912075476));
#22205=CARTESIAN_POINT('Ctrl Pts',(-53.7238113998707,-101.21578341734,177.6423391512));
#22206=CARTESIAN_POINT('Ctrl Pts',(-53.7138734058908,-101.122561645335,
175.985484901707));
#22207=CARTESIAN_POINT('Ctrl Pts',(-53.7039354119109,-101.029339873331,
174.328630652215));
#22208=CARTESIAN_POINT('Ctrl Pts',(-54.8589690335105,-100.811924344053,
173.157057825983));
#22209=CARTESIAN_POINT('Ctrl Pts',(-56.0140026551102,-100.594508814776,
171.985484999752));
#22210=CARTESIAN_POINT('Ctrl Pts',(-57.65158327928,-100.325650551179,171.985485069079));
#22211=CARTESIAN_POINT('Ctrl Pts',(-59.2891639034499,-100.056792287582,
171.985485138407));
#22212=CARTESIAN_POINT('Ctrl Pts',(-60.4441974275576,-99.8393767686974,
173.157058062683));
#22213=CARTESIAN_POINT('Ctrl Pts',(-61.5992309516654,-99.6219612498133,
174.328630986959));
#22214=CARTESIAN_POINT('Ctrl Pts',(-61.5892928198112,-99.528739492507,175.985485236451));
#22215=CARTESIAN_POINT('Ctrl Pts',(-61.579354687957,-99.4355177352008,177.642339485944));
#22216=CARTESIAN_POINT('Ctrl Pts',(-60.4044449405234,-99.4664897351676,
178.813912312176));
#22217=CARTESIAN_POINT('Ctrl Pts',(-59.2295351930898,-99.4974617351344,
179.985485138407));
#22218=CARTESIAN_POINT('Ctrl Pts',(-57.5720784430859,-99.5798764694207,
179.985485069079));
#22219=CARTESIAN_POINT('Ctrl Pts',(-55.914621693082,-99.662291203707,179.985484999752));
#22220=CARTESIAN_POINT('Ctrl Pts',(-54.7397120431402,-99.6932631932805,
178.813912075476));
#22221=CARTESIAN_POINT('Ctrl Pts',(-53.5648023931984,-99.724235182854,177.6423391512));
#22222=CARTESIAN_POINT('Ctrl Pts',(-53.5548643992186,-99.6310134108495,
175.985484901707));
#22223=CARTESIAN_POINT('Ctrl Pts',(-53.5449264052387,-99.5377916388449,
174.328630652215));
#22224=CARTESIAN_POINT('Ctrl Pts',(-54.6999600268383,-99.3203761095675,
173.157057825983));
#22225=CARTESIAN_POINT('Ctrl Pts',(-55.8549936484379,-99.10296058029,171.985484999752));
#22226=CARTESIAN_POINT('Ctrl Pts',(-57.4925742726078,-98.834102316693,171.985485069079));
#22227=CARTESIAN_POINT('Ctrl Pts',(-59.1301548967777,-98.5652440530961,
171.985485138407));
#22228=CARTESIAN_POINT('Ctrl Pts',(-60.2851884208854,-98.3478285342118,
173.157058062683));
#22229=CARTESIAN_POINT('Ctrl Pts',(-61.4402219449932,-98.1304130153276,
174.328630986959));
#22230=CARTESIAN_POINT('Ctrl Pts',(-61.430283813139,-98.0371912580215,175.985485236451));
#22231=CARTESIAN_POINT('Ctrl Pts',(-61.4203456812848,-97.9439695007152,
177.642339485944));
#22232=CARTESIAN_POINT('Ctrl Pts',(-60.2454359338512,-97.974941500682,178.813912312176));
#22233=CARTESIAN_POINT('Ctrl Pts',(-59.0705261864175,-98.0059135006488,
179.985485138407));
#22234=CARTESIAN_POINT('Ctrl Pts',(-57.4130694364136,-98.0883282349351,
179.985485069079));
#22235=CARTESIAN_POINT('Ctrl Pts',(-55.7556126864097,-98.1707429692214,
179.985484999752));
#22236=CARTESIAN_POINT('Ctrl Pts',(-54.580703036468,-98.2017149587949,178.813912075476));
#22237=CARTESIAN_POINT('Ctrl Pts',(-56.181115489574,-113.283598570176,178.821287383467));
#22238=CARTESIAN_POINT('Ctrl Pts',(-55.0031681001975,-113.314894403068,
177.646659506339));
#22239=CARTESIAN_POINT('Ctrl Pts',(-54.9932301063974,-113.221672631044,
175.985484901271));
#22240=CARTESIAN_POINT('Ctrl Pts',(-54.9832921125973,-113.12845085902,174.324310296203));
#22241=CARTESIAN_POINT('Ctrl Pts',(-56.1413634738858,-112.910711486397,
173.149682517375));
#22242=CARTESIAN_POINT('Ctrl Pts',(-57.2994348351743,-112.692972113774,
171.975054738546));
#22243=CARTESIAN_POINT('Ctrl Pts',(-58.9413114718314,-112.423655866545,
171.975054808055));
#22244=CARTESIAN_POINT('Ctrl Pts',(-60.5831881084886,-112.154339619316,
171.975054877564));
#22245=CARTESIAN_POINT('Ctrl Pts',(-61.741259372031,-111.936600257113,173.149682754692));
#22246=CARTESIAN_POINT('Ctrl Pts',(-62.8993306355734,-111.71886089491,174.32431063182));
#22247=CARTESIAN_POINT('Ctrl Pts',(-62.8893925035395,-111.625639137623,
175.985485236888));
#22248=CARTESIAN_POINT('Ctrl Pts',(-62.8794543715055,-111.532417380336,
177.646659841956));
#22249=CARTESIAN_POINT('Ctrl Pts',(-61.701506884383,-111.563713223648,178.821287620784));
#22250=CARTESIAN_POINT('Ctrl Pts',(-60.5235593972605,-111.595009066961,
179.995915399612));
#22251=CARTESIAN_POINT('Ctrl Pts',(-58.8618066347693,-111.677881784879,
179.995915330104));
#22252=CARTESIAN_POINT('Ctrl Pts',(-57.2000538722782,-111.760754502798,
179.995915260595));
#22253=CARTESIAN_POINT('Ctrl Pts',(-56.0221064829017,-111.79205033569,178.821287383467));
#22254=CARTESIAN_POINT('Ctrl Pts',(-54.8441590935253,-111.823346168582,
177.646659506339));
#22255=CARTESIAN_POINT('Ctrl Pts',(-54.8342210997252,-111.730124396559,
175.985484901271));
#22256=CARTESIAN_POINT('Ctrl Pts',(-54.8242831059251,-111.636902624535,
174.324310296203));
#22257=CARTESIAN_POINT('Ctrl Pts',(-55.9823544672136,-111.419163251912,
173.149682517375));
#22258=CARTESIAN_POINT('Ctrl Pts',(-57.1404258285021,-111.201423879289,
171.975054738546));
#22259=CARTESIAN_POINT('Ctrl Pts',(-58.7823024651592,-110.932107632059,
171.975054808055));
#22260=CARTESIAN_POINT('Ctrl Pts',(-60.4241791018163,-110.66279138483,171.975054877564));
#22261=CARTESIAN_POINT('Ctrl Pts',(-61.5822503653587,-110.445052022627,
173.149682754692));
#22262=CARTESIAN_POINT('Ctrl Pts',(-62.7403216289012,-110.227312660424,
174.32431063182));
#22263=CARTESIAN_POINT('Ctrl Pts',(-62.7303834968672,-110.134090903137,
175.985485236888));
#22264=CARTESIAN_POINT('Ctrl Pts',(-62.7204453648333,-110.04086914585,177.646659841956));
#22265=CARTESIAN_POINT('Ctrl Pts',(-61.5424978777108,-110.072164989163,
178.821287620784));
#22266=CARTESIAN_POINT('Ctrl Pts',(-60.3645503905882,-110.103460832475,
179.995915399612));
#22267=CARTESIAN_POINT('Ctrl Pts',(-58.7027976280971,-110.186333550394,
179.995915330104));
#22268=CARTESIAN_POINT('Ctrl Pts',(-57.041044865606,-110.269206268313,179.995915260595));
#22269=CARTESIAN_POINT('Ctrl Pts',(-55.8630974762295,-110.300502101205,
178.821287383467));
#22270=CARTESIAN_POINT('Ctrl Pts',(-54.6851500868531,-110.331797934097,
177.646659506339));
#22271=CARTESIAN_POINT('Ctrl Pts',(-54.675212093053,-110.238576162073,175.985484901271));
#22272=CARTESIAN_POINT('Ctrl Pts',(-54.6652740992529,-110.145354390049,
174.324310296203));
#22273=CARTESIAN_POINT('Ctrl Pts',(-55.8233454605414,-109.927615017426,
173.149682517375));
#22274=CARTESIAN_POINT('Ctrl Pts',(-56.9814168218299,-109.709875644803,
171.975054738546));
#22275=CARTESIAN_POINT('Ctrl Pts',(-58.623293458487,-109.440559397574,171.975054808055));
#22276=CARTESIAN_POINT('Ctrl Pts',(-60.2651700951441,-109.171243150344,
171.975054877564));
#22277=CARTESIAN_POINT('Ctrl Pts',(-61.4232413586865,-108.953503788142,
173.149682754692));
#22278=CARTESIAN_POINT('Ctrl Pts',(-62.581312622229,-108.735764425939,174.32431063182));
#22279=CARTESIAN_POINT('Ctrl Pts',(-62.571374490195,-108.642542668652,175.985485236888));
#22280=CARTESIAN_POINT('Ctrl Pts',(-62.5614363581611,-108.549320911365,
177.646659841956));
#22281=CARTESIAN_POINT('Ctrl Pts',(-61.3834888710385,-108.580616754677,
178.821287620784));
#22282=CARTESIAN_POINT('Ctrl Pts',(-60.205541383916,-108.61191259799,179.995915399612));
#22283=CARTESIAN_POINT('Ctrl Pts',(-58.5437886214249,-108.694785315908,
179.995915330104));
#22284=CARTESIAN_POINT('Ctrl Pts',(-56.8820358589338,-108.777658033827,
179.995915260595));
#22285=CARTESIAN_POINT('Ctrl Pts',(-55.7040884695573,-108.808953866719,
178.821287383467));
#22286=CARTESIAN_POINT('Ctrl Pts',(-54.5261410801808,-108.840249699611,
177.646659506339));
#22287=CARTESIAN_POINT('Ctrl Pts',(-54.5162030863807,-108.747027927587,
175.985484901271));
#22288=CARTESIAN_POINT('Ctrl Pts',(-54.5062650925806,-108.653806155564,
174.324310296203));
#22289=CARTESIAN_POINT('Ctrl Pts',(-55.6643364538691,-108.436066782941,
173.149682517375));
#22290=CARTESIAN_POINT('Ctrl Pts',(-56.8224078151577,-108.218327410317,
171.975054738546));
#22291=CARTESIAN_POINT('Ctrl Pts',(-58.4642844518147,-107.949011163088,
171.975054808055));
#22292=CARTESIAN_POINT('Ctrl Pts',(-60.1061610884719,-107.679694915859,
171.975054877564));
#22293=CARTESIAN_POINT('Ctrl Pts',(-61.2642323520143,-107.461955553656,
173.149682754692));
#22294=CARTESIAN_POINT('Ctrl Pts',(-62.4223036155567,-107.244216191453,
174.32431063182));
#22295=CARTESIAN_POINT('Ctrl Pts',(-62.4123654835228,-107.150994434166,
175.985485236888));
#22296=CARTESIAN_POINT('Ctrl Pts',(-62.4024273514889,-107.057772676879,
177.646659841956));
#22297=CARTESIAN_POINT('Ctrl Pts',(-61.2244798643663,-107.089068520192,
178.821287620784));
#22298=CARTESIAN_POINT('Ctrl Pts',(-60.0465323772438,-107.120364363504,
179.995915399612));
#22299=CARTESIAN_POINT('Ctrl Pts',(-58.3847796147526,-107.203237081423,
179.995915330104));
#22300=CARTESIAN_POINT('Ctrl Pts',(-56.7230268522615,-107.286109799341,
179.995915260595));
#22301=CARTESIAN_POINT('Ctrl Pts',(-55.5450794628851,-107.317405632233,
178.821287383467));
#22302=CARTESIAN_POINT('Ctrl Pts',(-54.3671320735086,-107.348701465125,
177.646659506339));
#22303=CARTESIAN_POINT('Ctrl Pts',(-54.3571940797085,-107.255479693102,
175.985484901271));
#22304=CARTESIAN_POINT('Ctrl Pts',(-54.3472560859084,-107.162257921078,
174.324310296203));
#22305=CARTESIAN_POINT('Ctrl Pts',(-55.5053274471969,-106.944518548455,
173.149682517375));
#22306=CARTESIAN_POINT('Ctrl Pts',(-56.6633988084854,-106.726779175832,
171.975054738546));
#22307=CARTESIAN_POINT('Ctrl Pts',(-58.3052754451425,-106.457462928602,
171.975054808055));
#22308=CARTESIAN_POINT('Ctrl Pts',(-59.9471520817997,-106.188146681373,
171.975054877564));
#22309=CARTESIAN_POINT('Ctrl Pts',(-61.1052233453421,-105.97040731917,173.149682754692));
#22310=CARTESIAN_POINT('Ctrl Pts',(-62.2632946088845,-105.752667956968,
174.32431063182));
#22311=CARTESIAN_POINT('Ctrl Pts',(-62.2533564768505,-105.659446199681,
175.985485236888));
#22312=CARTESIAN_POINT('Ctrl Pts',(-62.2434183448166,-105.566224442394,
177.646659841956));
#22313=CARTESIAN_POINT('Ctrl Pts',(-61.0654708576941,-105.597520285706,
178.821287620784));
#22314=CARTESIAN_POINT('Ctrl Pts',(-59.8875233705716,-105.628816129018,
179.995915399612));
#22315=CARTESIAN_POINT('Ctrl Pts',(-58.2257706080804,-105.711688846937,
179.995915330104));
#22316=CARTESIAN_POINT('Ctrl Pts',(-56.5640178455893,-105.794561564856,
179.995915260595));
#22317=CARTESIAN_POINT('Ctrl Pts',(-55.3860704562128,-105.825857397748,
178.821287383467));
#22318=CARTESIAN_POINT('Ctrl Pts',(-54.2081230668364,-105.85715323064,177.646659506339));
#22319=CARTESIAN_POINT('Ctrl Pts',(-54.1981850730363,-105.763931458616,
175.985484901271));
#22320=CARTESIAN_POINT('Ctrl Pts',(-54.1882470792362,-105.670709686593,
174.324310296203));
#22321=CARTESIAN_POINT('Ctrl Pts',(-55.3463184405247,-105.452970313969,
173.149682517375));
#22322=CARTESIAN_POINT('Ctrl Pts',(-56.5043898018132,-105.235230941346,
171.975054738546));
#22323=CARTESIAN_POINT('Ctrl Pts',(-58.1462664384703,-104.965914694117,
171.975054808055));
#22324=CARTESIAN_POINT('Ctrl Pts',(-59.7881430751274,-104.696598446888,
171.975054877564));
#22325=CARTESIAN_POINT('Ctrl Pts',(-60.9462143386698,-104.478859084685,
173.149682754692));
#22326=CARTESIAN_POINT('Ctrl Pts',(-62.1042856022123,-104.261119722482,
174.32431063182));
#22327=CARTESIAN_POINT('Ctrl Pts',(-62.0943474701783,-104.167897965195,
175.985485236888));
#22328=CARTESIAN_POINT('Ctrl Pts',(-62.0844093381444,-104.074676207908,
177.646659841956));
#22329=CARTESIAN_POINT('Ctrl Pts',(-60.9064618510219,-104.10597205122,178.821287620784));
#22330=CARTESIAN_POINT('Ctrl Pts',(-59.7285143638993,-104.137267894533,
179.995915399612));
#22331=CARTESIAN_POINT('Ctrl Pts',(-58.0667616014082,-104.220140612451,
179.995915330104));
#22332=CARTESIAN_POINT('Ctrl Pts',(-56.4050088389171,-104.30301333037,179.995915260595));
#22333=CARTESIAN_POINT('Ctrl Pts',(-55.2270614495406,-104.334309163262,
178.821287383467));
#22334=CARTESIAN_POINT('Ctrl Pts',(-54.0491140601642,-104.365604996154,
177.646659506339));
#22335=CARTESIAN_POINT('Ctrl Pts',(-54.039176066364,-104.272383224131,175.985484901271));
#22336=CARTESIAN_POINT('Ctrl Pts',(-54.029238072564,-104.179161452107,174.324310296203));
#22337=CARTESIAN_POINT('Ctrl Pts',(-55.1873094338524,-103.961422079484,
173.149682517375));
#22338=CARTESIAN_POINT('Ctrl Pts',(-56.345380795141,-103.743682706861,171.975054738546));
#22339=CARTESIAN_POINT('Ctrl Pts',(-57.9872574317981,-103.474366459631,
171.975054808055));
#22340=CARTESIAN_POINT('Ctrl Pts',(-59.6291340684552,-103.205050212402,
171.975054877564));
#22341=CARTESIAN_POINT('Ctrl Pts',(-60.7872053319976,-102.987310850199,
173.149682754692));
#22342=CARTESIAN_POINT('Ctrl Pts',(-61.94527659554,-102.769571487996,174.32431063182));
#22343=CARTESIAN_POINT('Ctrl Pts',(-61.9353384635061,-102.676349730709,
175.985485236888));
#22344=CARTESIAN_POINT('Ctrl Pts',(-61.9254003314722,-102.583127973422,
177.646659841956));
#22345=CARTESIAN_POINT('Ctrl Pts',(-60.7474528443496,-102.614423816735,
178.821287620784));
#22346=CARTESIAN_POINT('Ctrl Pts',(-59.5695053572271,-102.645719660047,
179.995915399612));
#22347=CARTESIAN_POINT('Ctrl Pts',(-57.907752594736,-102.728592377966,179.995915330104));
#22348=CARTESIAN_POINT('Ctrl Pts',(-56.2459998322448,-102.811465095885,
179.995915260595));
#22349=CARTESIAN_POINT('Ctrl Pts',(-55.0680524428684,-102.842760928777,
178.821287383467));
#22350=CARTESIAN_POINT('Ctrl Pts',(-53.8901050534919,-102.874056761669,
177.646659506339));
#22351=CARTESIAN_POINT('Ctrl Pts',(-53.8801670596918,-102.780834989645,
175.985484901271));
#22352=CARTESIAN_POINT('Ctrl Pts',(-53.8702290658917,-102.687613217621,
174.324310296203));
#22353=CARTESIAN_POINT('Ctrl Pts',(-55.0283004271802,-102.469873844998,
173.149682517375));
#22354=CARTESIAN_POINT('Ctrl Pts',(-56.1863717884687,-102.252134472375,
171.975054738546));
#22355=CARTESIAN_POINT('Ctrl Pts',(-57.8282484251258,-101.982818225146,
171.975054808055));
#22356=CARTESIAN_POINT('Ctrl Pts',(-59.470125061783,-101.713501977916,171.975054877564));
#22357=CARTESIAN_POINT('Ctrl Pts',(-60.6281963253254,-101.495762615714,
173.149682754692));
#22358=CARTESIAN_POINT('Ctrl Pts',(-61.7862675888678,-101.278023253511,
174.32431063182));
#22359=CARTESIAN_POINT('Ctrl Pts',(-61.7763294568339,-101.184801496224,
175.985485236888));
#22360=CARTESIAN_POINT('Ctrl Pts',(-61.7663913247999,-101.091579738937,
177.646659841956));
#22361=CARTESIAN_POINT('Ctrl Pts',(-60.5884438376774,-101.122875582249,
178.821287620784));
#22362=CARTESIAN_POINT('Ctrl Pts',(-59.4104963505549,-101.154171425562,
179.995915399612));
#22363=CARTESIAN_POINT('Ctrl Pts',(-57.7487435880637,-101.23704414348,179.995915330104));
#22364=CARTESIAN_POINT('Ctrl Pts',(-56.0869908255726,-101.319916861399,
179.995915260595));
#22365=CARTESIAN_POINT('Ctrl Pts',(-54.9090434361961,-101.351212694291,
178.821287383467));
#22366=CARTESIAN_POINT('Ctrl Pts',(-53.7310960468197,-101.382508527183,
177.646659506339));
#22367=CARTESIAN_POINT('Ctrl Pts',(-53.7211580530196,-101.289286755159,
175.985484901271));
#22368=CARTESIAN_POINT('Ctrl Pts',(-53.7112200592195,-101.196064983136,
174.324310296203));
#22369=CARTESIAN_POINT('Ctrl Pts',(-54.869291420508,-100.978325610513,173.149682517375));
#22370=CARTESIAN_POINT('Ctrl Pts',(-56.0273627817965,-100.760586237889,
171.975054738546));
#22371=CARTESIAN_POINT('Ctrl Pts',(-57.6692394184536,-100.49126999066,171.975054808055));
#22372=CARTESIAN_POINT('Ctrl Pts',(-59.3111160551107,-100.221953743431,
171.975054877564));
#22373=CARTESIAN_POINT('Ctrl Pts',(-60.4691873186531,-100.004214381228,
173.149682754692));
#22374=CARTESIAN_POINT('Ctrl Pts',(-61.6272585821956,-99.7864750190253,
174.32431063182));
#22375=CARTESIAN_POINT('Ctrl Pts',(-61.6173204501616,-99.6932532617382,
175.985485236888));
#22376=CARTESIAN_POINT('Ctrl Pts',(-61.6073823181277,-99.6000315044512,
177.646659841956));
#22377=CARTESIAN_POINT('Ctrl Pts',(-60.4294348310052,-99.6313273477637,
178.821287620784));
#22378=CARTESIAN_POINT('Ctrl Pts',(-59.2514873438827,-99.6626231910761,
179.995915399612));
#22379=CARTESIAN_POINT('Ctrl Pts',(-57.5897345813915,-99.7454959089947,
179.995915330104));
#22380=CARTESIAN_POINT('Ctrl Pts',(-55.9279818189004,-99.8283686269133,
179.995915260595));
#22381=CARTESIAN_POINT('Ctrl Pts',(-54.7500344295239,-99.8596644598054,
178.821287383467));
#22382=CARTESIAN_POINT('Ctrl Pts',(-53.5720870401475,-99.8909602926975,
177.646659506339));
#22383=CARTESIAN_POINT('Ctrl Pts',(-53.5621490463474,-99.7977385206737,
175.985484901271));
#22384=CARTESIAN_POINT('Ctrl Pts',(-53.5522110525473,-99.7045167486501,
174.324310296203));
#22385=CARTESIAN_POINT('Ctrl Pts',(-54.7102824138358,-99.4867773760269,
173.149682517375));
#22386=CARTESIAN_POINT('Ctrl Pts',(-55.8683537751243,-99.2690380034038,
171.975054738546));
#22387=CARTESIAN_POINT('Ctrl Pts',(-57.5102304117814,-98.9997217561745,
171.975054808055));
#22388=CARTESIAN_POINT('Ctrl Pts',(-59.1521070484385,-98.7304055089452,
171.975054877564));
#22389=CARTESIAN_POINT('Ctrl Pts',(-60.3101783119809,-98.5126661467424,
173.149682754692));
#22390=CARTESIAN_POINT('Ctrl Pts',(-61.4682495755234,-98.2949267845397,
174.32431063182));
#22391=CARTESIAN_POINT('Ctrl Pts',(-61.4583114434894,-98.2017050272526,
175.985485236888));
#22392=CARTESIAN_POINT('Ctrl Pts',(-61.4483733114555,-98.1084832699656,
177.646659841956));
#22393=CARTESIAN_POINT('Ctrl Pts',(-60.2704258243329,-98.139779113278,178.821287620784));
#22394=CARTESIAN_POINT('Ctrl Pts',(-59.0924783372104,-98.1710749565905,
179.995915399612));
#22395=CARTESIAN_POINT('Ctrl Pts',(-57.4307255747193,-98.2539476745091,
179.995915330104));
#22396=CARTESIAN_POINT('Ctrl Pts',(-55.7689728122282,-98.3368203924277,
179.995915260595));
#22397=CARTESIAN_POINT('Ctrl Pts',(-54.5910254228517,-98.3681162253198,
178.821287383467));
#22398=CARTESIAN_POINT('Ctrl Pts',(-56.1988062143188,-113.449542435949,
178.821287383467));
#22399=CARTESIAN_POINT('Ctrl Pts',(-55.0208588249424,-113.480838268841,
177.646659506339));
#22400=CARTESIAN_POINT('Ctrl Pts',(-55.0109208311422,-113.387616496817,
175.985484901271));
#22401=CARTESIAN_POINT('Ctrl Pts',(-55.0009828373422,-113.294394724794,
174.324310296203));
#22402=CARTESIAN_POINT('Ctrl Pts',(-56.1590541986307,-113.07665535217,173.149682517375));
#22403=CARTESIAN_POINT('Ctrl Pts',(-57.3171255599192,-112.858915979547,
171.975054738546));
#22404=CARTESIAN_POINT('Ctrl Pts',(-58.9590021965763,-112.589599732318,
171.975054808055));
#22405=CARTESIAN_POINT('Ctrl Pts',(-60.6008788332334,-112.320283485089,
171.975054877564));
#22406=CARTESIAN_POINT('Ctrl Pts',(-61.7589500967758,-112.102544122886,
173.149682754692));
#22407=CARTESIAN_POINT('Ctrl Pts',(-62.9170213603182,-111.884804760683,
174.32431063182));
#22408=CARTESIAN_POINT('Ctrl Pts',(-62.9070832282843,-111.791583003396,
175.985485236888));
#22409=CARTESIAN_POINT('Ctrl Pts',(-62.8971450962504,-111.698361246109,
177.646659841956));
#22410=CARTESIAN_POINT('Ctrl Pts',(-61.7191976091278,-111.729657089422,
178.821287620784));
#22411=CARTESIAN_POINT('Ctrl Pts',(-60.5412501220053,-111.760952932734,
179.995915399612));
#22412=CARTESIAN_POINT('Ctrl Pts',(-58.8794973595142,-111.843825650653,
179.995915330104));
#22413=CARTESIAN_POINT('Ctrl Pts',(-57.217744597023,-111.926698368571,179.995915260595));
#22414=CARTESIAN_POINT('Ctrl Pts',(-56.0397972076466,-111.957994201463,
178.821287383467));
#22415=CARTESIAN_POINT('Ctrl Pts',(-54.8618498182701,-111.989290034355,
177.646659506339));
#22416=CARTESIAN_POINT('Ctrl Pts',(-54.85191182447,-111.896068262332,175.985484901271));
#22417=CARTESIAN_POINT('Ctrl Pts',(-54.8419738306699,-111.802846490308,
174.324310296203));
#22418=CARTESIAN_POINT('Ctrl Pts',(-56.0000451919584,-111.585107117685,
173.149682517375));
#22419=CARTESIAN_POINT('Ctrl Pts',(-57.158116553247,-111.367367745062,171.975054738546));
#22420=CARTESIAN_POINT('Ctrl Pts',(-58.799993189904,-111.098051497832,171.975054808055));
#22421=CARTESIAN_POINT('Ctrl Pts',(-60.4418698265612,-110.828735250603,
171.975054877564));
#22422=CARTESIAN_POINT('Ctrl Pts',(-61.5999410901036,-110.6109958884,173.149682754692));
#22423=CARTESIAN_POINT('Ctrl Pts',(-62.758012353646,-110.393256526198,174.32431063182));
#22424=CARTESIAN_POINT('Ctrl Pts',(-62.7480742216121,-110.30003476891,175.985485236888));
#22425=CARTESIAN_POINT('Ctrl Pts',(-62.7381360895782,-110.206813011623,
177.646659841956));
#22426=CARTESIAN_POINT('Ctrl Pts',(-61.5601886024556,-110.238108854936,
178.821287620784));
#22427=CARTESIAN_POINT('Ctrl Pts',(-60.3822411153331,-110.269404698248,
179.995915399612));
#22428=CARTESIAN_POINT('Ctrl Pts',(-58.7204883528419,-110.352277416167,
179.995915330104));
#22429=CARTESIAN_POINT('Ctrl Pts',(-57.0587355903508,-110.435150134086,
179.995915260595));
#22430=CARTESIAN_POINT('Ctrl Pts',(-55.8807882009743,-110.466445966978,
178.821287383467));
#22431=CARTESIAN_POINT('Ctrl Pts',(-54.7028408115979,-110.49774179987,177.646659506339));
#22432=CARTESIAN_POINT('Ctrl Pts',(-54.6929028177978,-110.404520027846,
175.985484901271));
#22433=CARTESIAN_POINT('Ctrl Pts',(-54.6829648239977,-110.311298255822,
174.324310296203));
#22434=CARTESIAN_POINT('Ctrl Pts',(-55.8410361852862,-110.093558883199,
173.149682517375));
#22435=CARTESIAN_POINT('Ctrl Pts',(-56.9991075465747,-109.875819510576,
171.975054738546));
#22436=CARTESIAN_POINT('Ctrl Pts',(-58.6409841832318,-109.606503263347,
171.975054808055));
#22437=CARTESIAN_POINT('Ctrl Pts',(-60.2828608198889,-109.337187016117,
171.975054877564));
#22438=CARTESIAN_POINT('Ctrl Pts',(-61.4409320834313,-109.119447653915,
173.149682754692));
#22439=CARTESIAN_POINT('Ctrl Pts',(-62.5990033469738,-108.901708291712,
174.32431063182));
#22440=CARTESIAN_POINT('Ctrl Pts',(-62.5890652149398,-108.808486534425,
175.985485236888));
#22441=CARTESIAN_POINT('Ctrl Pts',(-62.5791270829059,-108.715264777138,
177.646659841956));
#22442=CARTESIAN_POINT('Ctrl Pts',(-61.4011795957834,-108.74656062045,178.821287620784));
#22443=CARTESIAN_POINT('Ctrl Pts',(-60.2232321086609,-108.777856463763,
179.995915399612));
#22444=CARTESIAN_POINT('Ctrl Pts',(-58.5614793461697,-108.860729181681,
179.995915330104));
#22445=CARTESIAN_POINT('Ctrl Pts',(-56.8997265836786,-108.9436018996,179.995915260595));
#22446=CARTESIAN_POINT('Ctrl Pts',(-55.7217791943021,-108.974897732492,
178.821287383467));
#22447=CARTESIAN_POINT('Ctrl Pts',(-54.5438318049257,-109.006193565384,
177.646659506339));
#22448=CARTESIAN_POINT('Ctrl Pts',(-54.5338938111256,-108.91297179336,175.985484901271));
#22449=CARTESIAN_POINT('Ctrl Pts',(-54.5239558173255,-108.819750021337,
174.324310296203));
#22450=CARTESIAN_POINT('Ctrl Pts',(-55.682027178614,-108.602010648714,173.149682517375));
#22451=CARTESIAN_POINT('Ctrl Pts',(-56.8400985399025,-108.384271276091,
171.975054738546));
#22452=CARTESIAN_POINT('Ctrl Pts',(-58.4819751765596,-108.114955028861,
171.975054808055));
#22453=CARTESIAN_POINT('Ctrl Pts',(-60.1238518132167,-107.845638781632,
171.975054877564));
#22454=CARTESIAN_POINT('Ctrl Pts',(-61.2819230767591,-107.627899419429,
173.149682754692));
#22455=CARTESIAN_POINT('Ctrl Pts',(-62.4399943403016,-107.410160057226,
174.32431063182));
#22456=CARTESIAN_POINT('Ctrl Pts',(-62.4300562082676,-107.316938299939,
175.985485236888));
#22457=CARTESIAN_POINT('Ctrl Pts',(-62.4201180762337,-107.223716542652,
177.646659841956));
#22458=CARTESIAN_POINT('Ctrl Pts',(-61.2421705891111,-107.255012385965,
178.821287620784));
#22459=CARTESIAN_POINT('Ctrl Pts',(-60.0642231019886,-107.286308229277,
179.995915399612));
#22460=CARTESIAN_POINT('Ctrl Pts',(-58.4024703394975,-107.369180947196,
179.995915330104));
#22461=CARTESIAN_POINT('Ctrl Pts',(-56.7407175770064,-107.452053665114,
179.995915260595));
#22462=CARTESIAN_POINT('Ctrl Pts',(-55.5627701876299,-107.483349498006,
178.821287383467));
#22463=CARTESIAN_POINT('Ctrl Pts',(-54.3848227982534,-107.514645330899,
177.646659506339));
#22464=CARTESIAN_POINT('Ctrl Pts',(-54.3748848044533,-107.421423558875,
175.985484901271));
#22465=CARTESIAN_POINT('Ctrl Pts',(-54.3649468106533,-107.328201786851,
174.324310296203));
#22466=CARTESIAN_POINT('Ctrl Pts',(-55.5230181719417,-107.110462414228,
173.149682517375));
#22467=CARTESIAN_POINT('Ctrl Pts',(-56.6810895332303,-106.892723041605,
171.975054738546));
#22468=CARTESIAN_POINT('Ctrl Pts',(-58.3229661698874,-106.623406794376,
171.975054808055));
#22469=CARTESIAN_POINT('Ctrl Pts',(-59.9648428065445,-106.354090547146,
171.975054877564));
#22470=CARTESIAN_POINT('Ctrl Pts',(-61.1229140700869,-106.136351184943,
173.149682754692));
#22471=CARTESIAN_POINT('Ctrl Pts',(-62.2809853336293,-105.918611822741,
174.32431063182));
#22472=CARTESIAN_POINT('Ctrl Pts',(-62.2710472015954,-105.825390065454,
175.985485236888));
#22473=CARTESIAN_POINT('Ctrl Pts',(-62.2611090695615,-105.732168308167,
177.646659841956));
#22474=CARTESIAN_POINT('Ctrl Pts',(-61.0831615824389,-105.763464151479,
178.821287620784));
#22475=CARTESIAN_POINT('Ctrl Pts',(-59.9052140953164,-105.794759994792,
179.995915399612));
#22476=CARTESIAN_POINT('Ctrl Pts',(-58.2434613328252,-105.87763271271,179.995915330104));
#22477=CARTESIAN_POINT('Ctrl Pts',(-56.5817085703341,-105.960505430629,
179.995915260595));
#22478=CARTESIAN_POINT('Ctrl Pts',(-55.4037611809577,-105.991801263521,
178.821287383467));
#22479=CARTESIAN_POINT('Ctrl Pts',(-54.2258137915812,-106.023097096413,
177.646659506339));
#22480=CARTESIAN_POINT('Ctrl Pts',(-54.2158757977811,-105.929875324389,
175.985484901271));
#22481=CARTESIAN_POINT('Ctrl Pts',(-54.205937803981,-105.836653552366,174.324310296203));
#22482=CARTESIAN_POINT('Ctrl Pts',(-55.3640091652695,-105.618914179742,
173.149682517375));
#22483=CARTESIAN_POINT('Ctrl Pts',(-56.522080526558,-105.401174807119,171.975054738546));
#22484=CARTESIAN_POINT('Ctrl Pts',(-58.1639571632151,-105.13185855989,171.975054808055));
#22485=CARTESIAN_POINT('Ctrl Pts',(-59.8058337998722,-104.862542312661,
171.975054877564));
#22486=CARTESIAN_POINT('Ctrl Pts',(-60.9639050634147,-104.644802950458,
173.149682754692));
#22487=CARTESIAN_POINT('Ctrl Pts',(-62.1219763269571,-104.427063588255,
174.32431063182));
#22488=CARTESIAN_POINT('Ctrl Pts',(-62.1120381949232,-104.333841830968,
175.985485236888));
#22489=CARTESIAN_POINT('Ctrl Pts',(-62.1021000628892,-104.240620073681,
177.646659841956));
#22490=CARTESIAN_POINT('Ctrl Pts',(-60.9241525757667,-104.271915916993,
178.821287620784));
#22491=CARTESIAN_POINT('Ctrl Pts',(-59.7462050886442,-104.303211760306,
179.995915399612));
#22492=CARTESIAN_POINT('Ctrl Pts',(-58.084452326153,-104.386084478225,179.995915330104));
#22493=CARTESIAN_POINT('Ctrl Pts',(-56.4226995636619,-104.468957196143,
179.995915260595));
#22494=CARTESIAN_POINT('Ctrl Pts',(-55.2447521742854,-104.500253029035,
178.821287383467));
#22495=CARTESIAN_POINT('Ctrl Pts',(-54.066804784909,-104.531548861927,177.646659506339));
#22496=CARTESIAN_POINT('Ctrl Pts',(-54.0568667911089,-104.438327089904,
175.985484901271));
#22497=CARTESIAN_POINT('Ctrl Pts',(-54.0469287973088,-104.34510531788,174.324310296203));
#22498=CARTESIAN_POINT('Ctrl Pts',(-55.2050001585973,-104.127365945257,
173.149682517375));
#22499=CARTESIAN_POINT('Ctrl Pts',(-56.3630715198858,-103.909626572634,
171.975054738546));
#22500=CARTESIAN_POINT('Ctrl Pts',(-58.0049481565429,-103.640310325404,
171.975054808055));
#22501=CARTESIAN_POINT('Ctrl Pts',(-59.6468247932,-103.370994078175,171.975054877564));
#22502=CARTESIAN_POINT('Ctrl Pts',(-60.8048960567424,-103.153254715972,
173.149682754692));
#22503=CARTESIAN_POINT('Ctrl Pts',(-61.9629673202849,-102.93551535377,174.32431063182));
#22504=CARTESIAN_POINT('Ctrl Pts',(-61.9530291882509,-102.842293596483,
175.985485236888));
#22505=CARTESIAN_POINT('Ctrl Pts',(-61.943091056217,-102.749071839196,177.646659841956));
#22506=CARTESIAN_POINT('Ctrl Pts',(-60.7651435690945,-102.780367682508,
178.821287620784));
#22507=CARTESIAN_POINT('Ctrl Pts',(-59.587196081972,-102.81166352582,179.995915399612));
#22508=CARTESIAN_POINT('Ctrl Pts',(-57.9254433194808,-102.894536243739,
179.995915330104));
#22509=CARTESIAN_POINT('Ctrl Pts',(-56.2636905569897,-102.977408961658,
179.995915260595));
#22510=CARTESIAN_POINT('Ctrl Pts',(-55.0857431676132,-103.00870479455,178.821287383467));
#22511=CARTESIAN_POINT('Ctrl Pts',(-53.9077957782368,-103.040000627442,
177.646659506339));
#22512=CARTESIAN_POINT('Ctrl Pts',(-53.8978577844367,-102.946778855418,
175.985484901271));
#22513=CARTESIAN_POINT('Ctrl Pts',(-53.8879197906366,-102.853557083394,
174.324310296203));
#22514=CARTESIAN_POINT('Ctrl Pts',(-55.0459911519251,-102.635817710771,
173.149682517375));
#22515=CARTESIAN_POINT('Ctrl Pts',(-56.2040625132136,-102.418078338148,
171.975054738546));
#22516=CARTESIAN_POINT('Ctrl Pts',(-57.8459391498707,-102.148762090919,
171.975054808055));
#22517=CARTESIAN_POINT('Ctrl Pts',(-59.4878157865278,-101.879445843689,
171.975054877564));
#22518=CARTESIAN_POINT('Ctrl Pts',(-60.6458870500702,-101.661706481487,
173.149682754692));
#22519=CARTESIAN_POINT('Ctrl Pts',(-61.8039583136126,-101.443967119284,
174.32431063182));
#22520=CARTESIAN_POINT('Ctrl Pts',(-61.7940201815787,-101.350745361997,
175.985485236888));
#22521=CARTESIAN_POINT('Ctrl Pts',(-61.7840820495448,-101.25752360471,177.646659841956));
#22522=CARTESIAN_POINT('Ctrl Pts',(-60.6061345624222,-101.288819448022,
178.821287620784));
#22523=CARTESIAN_POINT('Ctrl Pts',(-59.4281870752997,-101.320115291335,
179.995915399612));
#22524=CARTESIAN_POINT('Ctrl Pts',(-57.7664343128086,-101.402988009253,
179.995915330104));
#22525=CARTESIAN_POINT('Ctrl Pts',(-56.1046815503175,-101.485860727172,
179.995915260595));
#22526=CARTESIAN_POINT('Ctrl Pts',(-54.926734160941,-101.517156560064,178.821287383467));
#22527=CARTESIAN_POINT('Ctrl Pts',(-53.7487867715645,-101.548452392956,
177.646659506339));
#22528=CARTESIAN_POINT('Ctrl Pts',(-53.7388487777644,-101.455230620932,
175.985484901271));
#22529=CARTESIAN_POINT('Ctrl Pts',(-53.7289107839643,-101.362008848909,
174.324310296203));
#22530=CARTESIAN_POINT('Ctrl Pts',(-54.8869821452528,-101.144269476286,
173.149682517375));
#22531=CARTESIAN_POINT('Ctrl Pts',(-56.0450535065414,-100.926530103662,
171.975054738546));
#22532=CARTESIAN_POINT('Ctrl Pts',(-57.6869301431984,-100.657213856433,
171.975054808055));
#22533=CARTESIAN_POINT('Ctrl Pts',(-59.3288067798556,-100.387897609204,
171.975054877564));
#22534=CARTESIAN_POINT('Ctrl Pts',(-60.486878043398,-100.170158247001,173.149682754692));
#22535=CARTESIAN_POINT('Ctrl Pts',(-61.6449493069404,-99.9524188847983,
174.32431063182));
#22536=CARTESIAN_POINT('Ctrl Pts',(-61.6350111749065,-99.8591971275113,
175.985485236888));
#22537=CARTESIAN_POINT('Ctrl Pts',(-61.6250730428726,-99.7659753702243,
177.646659841956));
#22538=CARTESIAN_POINT('Ctrl Pts',(-60.44712555575,-99.7972712135367,178.821287620784));
#22539=CARTESIAN_POINT('Ctrl Pts',(-59.2691780686275,-99.8285670568492,
179.995915399612));
#22540=CARTESIAN_POINT('Ctrl Pts',(-57.6074253061363,-99.9114397747677,
179.995915330104));
#22541=CARTESIAN_POINT('Ctrl Pts',(-55.9456725436452,-99.9943124926864,
179.995915260595));
#22542=CARTESIAN_POINT('Ctrl Pts',(-54.7677251542687,-100.025608325578,
178.821287383467));
#22543=CARTESIAN_POINT('Ctrl Pts',(-53.5897777648923,-100.05690415847,177.646659506339));
#22544=CARTESIAN_POINT('Ctrl Pts',(-53.5798397710922,-99.9636823864468,
175.985484901271));
#22545=CARTESIAN_POINT('Ctrl Pts',(-53.5699017772921,-99.8704606144232,
174.324310296203));
#22546=CARTESIAN_POINT('Ctrl Pts',(-54.7279731385806,-99.6527212418,173.149682517375));
#22547=CARTESIAN_POINT('Ctrl Pts',(-55.8860444998691,-99.4349818691769,
171.975054738546));
#22548=CARTESIAN_POINT('Ctrl Pts',(-57.5279211365262,-99.1656656219475,
171.975054808055));
#22549=CARTESIAN_POINT('Ctrl Pts',(-59.1697977731833,-98.8963493747183,
171.975054877564));
#22550=CARTESIAN_POINT('Ctrl Pts',(-60.3278690367257,-98.6786100125155,
173.149682754692));
#22551=CARTESIAN_POINT('Ctrl Pts',(-61.4859403002682,-98.4608706503128,
174.32431063182));
#22552=CARTESIAN_POINT('Ctrl Pts',(-61.4760021682342,-98.3676488930257,
175.985485236888));
#22553=CARTESIAN_POINT('Ctrl Pts',(-61.4660640362003,-98.2744271357387,
177.646659841956));
#22554=CARTESIAN_POINT('Ctrl Pts',(-60.2881165490778,-98.3057229790511,
178.821287620784));
#22555=CARTESIAN_POINT('Ctrl Pts',(-59.1101690619552,-98.3370188223636,
179.995915399612));
#22556=CARTESIAN_POINT('Ctrl Pts',(-57.4484162994641,-98.4198915402821,
179.995915330104));
#22557=CARTESIAN_POINT('Ctrl Pts',(-55.786663536973,-98.5027642582008,179.995915260595));
#22558=CARTESIAN_POINT('Ctrl Pts',(-54.6087161475965,-98.5340600910929,
178.821287383467));
#22559=CARTESIAN_POINT('Ctrl Pts',(-56.2237961054143,-113.614380048479,
178.813912075476));
#22560=CARTESIAN_POINT('Ctrl Pts',(-55.0488864554725,-113.645352038053,
177.6423391512));
#22561=CARTESIAN_POINT('Ctrl Pts',(-55.0389484614927,-113.552130266048,
175.985484901707));
#22562=CARTESIAN_POINT('Ctrl Pts',(-55.0290104675128,-113.458908494044,
174.328630652215));
#22563=CARTESIAN_POINT('Ctrl Pts',(-56.1840440891124,-113.241492964766,
173.157057825983));
#22564=CARTESIAN_POINT('Ctrl Pts',(-57.3390777107121,-113.024077435489,
171.985484999752));
#22565=CARTESIAN_POINT('Ctrl Pts',(-58.9766583348819,-112.755219171892,
171.985485069079));
#22566=CARTESIAN_POINT('Ctrl Pts',(-60.6142389590518,-112.486360908295,
171.985485138407));
#22567=CARTESIAN_POINT('Ctrl Pts',(-61.7692724831595,-112.268945389411,
173.157058062683));
#22568=CARTESIAN_POINT('Ctrl Pts',(-62.9243060072673,-112.051529870527,
174.328630986959));
#22569=CARTESIAN_POINT('Ctrl Pts',(-62.9143678754131,-111.95830811322,175.985485236451));
#22570=CARTESIAN_POINT('Ctrl Pts',(-62.9044297435589,-111.865086355914,
177.642339485944));
#22571=CARTESIAN_POINT('Ctrl Pts',(-61.7295199961253,-111.896058355881,
178.813912312176));
#22572=CARTESIAN_POINT('Ctrl Pts',(-60.5546102486917,-111.927030355848,
179.985485138407));
#22573=CARTESIAN_POINT('Ctrl Pts',(-58.8971534986878,-112.009445090134,
179.985485069079));
#22574=CARTESIAN_POINT('Ctrl Pts',(-57.2396967486839,-112.09185982442,179.985484999752));
#22575=CARTESIAN_POINT('Ctrl Pts',(-56.0647870987421,-112.122831813994,
178.813912075476));
#22576=CARTESIAN_POINT('Ctrl Pts',(-54.8898774488003,-112.153803803567,
177.6423391512));
#22577=CARTESIAN_POINT('Ctrl Pts',(-54.8799394548205,-112.060582031563,
175.985484901707));
#22578=CARTESIAN_POINT('Ctrl Pts',(-54.8700014608406,-111.967360259558,
174.328630652215));
#22579=CARTESIAN_POINT('Ctrl Pts',(-56.0250350824402,-111.749944730281,
173.157057825983));
#22580=CARTESIAN_POINT('Ctrl Pts',(-57.1800687040398,-111.532529201003,
171.985484999752));
#22581=CARTESIAN_POINT('Ctrl Pts',(-58.8176493282097,-111.263670937406,
171.985485069079));
#22582=CARTESIAN_POINT('Ctrl Pts',(-60.4552299523796,-110.994812673809,
171.985485138407));
#22583=CARTESIAN_POINT('Ctrl Pts',(-61.6102634764873,-110.777397154925,
173.157058062683));
#22584=CARTESIAN_POINT('Ctrl Pts',(-62.7652970005951,-110.559981636041,
174.328630986959));
#22585=CARTESIAN_POINT('Ctrl Pts',(-62.7553588687409,-110.466759878735,
175.985485236451));
#22586=CARTESIAN_POINT('Ctrl Pts',(-62.7454207368867,-110.373538121429,
177.642339485944));
#22587=CARTESIAN_POINT('Ctrl Pts',(-61.5705109894531,-110.404510121395,
178.813912312176));
#22588=CARTESIAN_POINT('Ctrl Pts',(-60.3956012420194,-110.435482121362,
179.985485138407));
#22589=CARTESIAN_POINT('Ctrl Pts',(-58.7381444920155,-110.517896855648,
179.985485069079));
#22590=CARTESIAN_POINT('Ctrl Pts',(-57.0806877420116,-110.600311589935,
179.985484999752));
#22591=CARTESIAN_POINT('Ctrl Pts',(-55.9057780920699,-110.631283579508,
178.813912075476));
#22592=CARTESIAN_POINT('Ctrl Pts',(-54.7308684421281,-110.662255569082,
177.6423391512));
#22593=CARTESIAN_POINT('Ctrl Pts',(-54.7209304481482,-110.569033797077,
175.985484901707));
#22594=CARTESIAN_POINT('Ctrl Pts',(-54.7109924541684,-110.475812025073,
174.328630652215));
#22595=CARTESIAN_POINT('Ctrl Pts',(-55.866026075768,-110.258396495795,173.157057825983));
#22596=CARTESIAN_POINT('Ctrl Pts',(-57.0210596973676,-110.040980966518,
171.985484999752));
#22597=CARTESIAN_POINT('Ctrl Pts',(-58.6586403215375,-109.772122702921,
171.985485069079));
#22598=CARTESIAN_POINT('Ctrl Pts',(-60.2962209457073,-109.503264439324,
171.985485138407));
#22599=CARTESIAN_POINT('Ctrl Pts',(-61.4512544698151,-109.28584892044,173.157058062683));
#22600=CARTESIAN_POINT('Ctrl Pts',(-62.6062879939228,-109.068433401555,
174.328630986959));
#22601=CARTESIAN_POINT('Ctrl Pts',(-62.5963498620687,-108.975211644249,
175.985485236451));
#22602=CARTESIAN_POINT('Ctrl Pts',(-62.5864117302145,-108.881989886943,
177.642339485944));
#22603=CARTESIAN_POINT('Ctrl Pts',(-61.4115019827808,-108.91296188691,178.813912312176));
#22604=CARTESIAN_POINT('Ctrl Pts',(-60.2365922353472,-108.943933886877,
179.985485138407));
#22605=CARTESIAN_POINT('Ctrl Pts',(-58.5791354853433,-109.026348621163,
179.985485069079));
#22606=CARTESIAN_POINT('Ctrl Pts',(-56.9216787353394,-109.108763355449,
179.985484999752));
#22607=CARTESIAN_POINT('Ctrl Pts',(-55.7467690853976,-109.139735345023,
178.813912075476));
#22608=CARTESIAN_POINT('Ctrl Pts',(-54.5718594354559,-109.170707334596,
177.6423391512));
#22609=CARTESIAN_POINT('Ctrl Pts',(-54.561921441476,-109.077485562592,175.985484901707));
#22610=CARTESIAN_POINT('Ctrl Pts',(-54.5519834474962,-108.984263790587,
174.328630652215));
#22611=CARTESIAN_POINT('Ctrl Pts',(-55.7070170690958,-108.76684826131,173.157057825983));
#22612=CARTESIAN_POINT('Ctrl Pts',(-56.8620506906954,-108.549432732032,
171.985484999752));
#22613=CARTESIAN_POINT('Ctrl Pts',(-58.4996313148652,-108.280574468435,
171.985485069079));
#22614=CARTESIAN_POINT('Ctrl Pts',(-60.1372119390351,-108.011716204838,
171.985485138407));
#22615=CARTESIAN_POINT('Ctrl Pts',(-61.2922454631428,-107.794300685954,
173.157058062683));
#22616=CARTESIAN_POINT('Ctrl Pts',(-62.4472789872506,-107.57688516707,174.328630986959));
#22617=CARTESIAN_POINT('Ctrl Pts',(-62.4373408553964,-107.483663409764,
175.985485236451));
#22618=CARTESIAN_POINT('Ctrl Pts',(-62.4274027235423,-107.390441652457,
177.642339485944));
#22619=CARTESIAN_POINT('Ctrl Pts',(-61.2524929761086,-107.421413652424,
178.813912312176));
#22620=CARTESIAN_POINT('Ctrl Pts',(-60.077583228675,-107.452385652391,179.985485138407));
#22621=CARTESIAN_POINT('Ctrl Pts',(-58.4201264786711,-107.534800386677,
179.985485069079));
#22622=CARTESIAN_POINT('Ctrl Pts',(-56.7626697286672,-107.617215120964,
179.985484999752));
#22623=CARTESIAN_POINT('Ctrl Pts',(-55.5877600787254,-107.648187110537,
178.813912075476));
#22624=CARTESIAN_POINT('Ctrl Pts',(-54.4128504287836,-107.67915910011,177.6423391512));
#22625=CARTESIAN_POINT('Ctrl Pts',(-54.4029124348038,-107.585937328106,
175.985484901707));
#22626=CARTESIAN_POINT('Ctrl Pts',(-54.3929744408239,-107.492715556102,
174.328630652215));
#22627=CARTESIAN_POINT('Ctrl Pts',(-55.5480080624235,-107.275300026824,
173.157057825983));
#22628=CARTESIAN_POINT('Ctrl Pts',(-56.7030416840231,-107.057884497547,
171.985484999752));
#22629=CARTESIAN_POINT('Ctrl Pts',(-58.340622308193,-106.78902623395,171.985485069079));
#22630=CARTESIAN_POINT('Ctrl Pts',(-59.9782029323629,-106.520167970353,
171.985485138407));
#22631=CARTESIAN_POINT('Ctrl Pts',(-61.1332364564706,-106.302752451468,
173.157058062683));
#22632=CARTESIAN_POINT('Ctrl Pts',(-62.2882699805784,-106.085336932584,
174.328630986959));
#22633=CARTESIAN_POINT('Ctrl Pts',(-62.2783318487242,-105.992115175278,
175.985485236451));
#22634=CARTESIAN_POINT('Ctrl Pts',(-62.26839371687,-105.898893417972,177.642339485944));
#22635=CARTESIAN_POINT('Ctrl Pts',(-61.0934839694364,-105.929865417939,
178.813912312176));
#22636=CARTESIAN_POINT('Ctrl Pts',(-59.9185742220028,-105.960837417905,
179.985485138407));
#22637=CARTESIAN_POINT('Ctrl Pts',(-58.2611174719989,-106.043252152192,
179.985485069079));
#22638=CARTESIAN_POINT('Ctrl Pts',(-56.603660721995,-106.125666886478,179.985484999752));
#22639=CARTESIAN_POINT('Ctrl Pts',(-55.4287510720532,-106.156638876051,
178.813912075476));
#22640=CARTESIAN_POINT('Ctrl Pts',(-54.2538414221114,-106.187610865625,
177.6423391512));
#22641=CARTESIAN_POINT('Ctrl Pts',(-54.2439034281315,-106.09438909362,175.985484901707));
#22642=CARTESIAN_POINT('Ctrl Pts',(-54.2339654341517,-106.001167321616,
174.328630652215));
#22643=CARTESIAN_POINT('Ctrl Pts',(-55.3889990557513,-105.783751792338,
173.157057825983));
#22644=CARTESIAN_POINT('Ctrl Pts',(-56.5440326773509,-105.566336263061,
171.985484999752));
#22645=CARTESIAN_POINT('Ctrl Pts',(-58.1816133015208,-105.297477999464,
171.985485069079));
#22646=CARTESIAN_POINT('Ctrl Pts',(-59.8191939256906,-105.028619735867,
171.985485138407));
#22647=CARTESIAN_POINT('Ctrl Pts',(-60.9742274497984,-104.811204216983,
173.157058062683));
#22648=CARTESIAN_POINT('Ctrl Pts',(-62.1292609739061,-104.593788698099,
174.328630986959));
#22649=CARTESIAN_POINT('Ctrl Pts',(-62.119322842052,-104.500566940792,175.985485236451));
#22650=CARTESIAN_POINT('Ctrl Pts',(-62.1093847101978,-104.407345183486,
177.642339485944));
#22651=CARTESIAN_POINT('Ctrl Pts',(-60.9344749627642,-104.438317183453,
178.813912312176));
#22652=CARTESIAN_POINT('Ctrl Pts',(-59.7595652153305,-104.46928918342,179.985485138407));
#22653=CARTESIAN_POINT('Ctrl Pts',(-58.1021084653266,-104.551703917706,
179.985485069079));
#22654=CARTESIAN_POINT('Ctrl Pts',(-56.4446517153227,-104.634118651992,
179.985484999752));
#22655=CARTESIAN_POINT('Ctrl Pts',(-55.269742065381,-104.665090641566,178.813912075476));
#22656=CARTESIAN_POINT('Ctrl Pts',(-54.0948324154392,-104.696062631139,
177.6423391512));
#22657=CARTESIAN_POINT('Ctrl Pts',(-54.0848944214593,-104.602840859135,
175.985484901707));
#22658=CARTESIAN_POINT('Ctrl Pts',(-54.0749564274795,-104.50961908713,174.328630652215));
#22659=CARTESIAN_POINT('Ctrl Pts',(-55.2299900490791,-104.292203557853,
173.157057825983));
#22660=CARTESIAN_POINT('Ctrl Pts',(-56.3850236706787,-104.074788028575,
171.985484999752));
#22661=CARTESIAN_POINT('Ctrl Pts',(-58.0226042948486,-103.805929764978,
171.985485069079));
#22662=CARTESIAN_POINT('Ctrl Pts',(-59.6601849190184,-103.537071501381,
171.985485138407));
#22663=CARTESIAN_POINT('Ctrl Pts',(-60.8152184431262,-103.319655982497,
173.157058062683));
#22664=CARTESIAN_POINT('Ctrl Pts',(-61.9702519672339,-103.102240463613,
174.328630986959));
#22665=CARTESIAN_POINT('Ctrl Pts',(-61.9603138353797,-103.009018706307,
175.985485236451));
#22666=CARTESIAN_POINT('Ctrl Pts',(-61.9503757035256,-102.915796949001,
177.642339485944));
#22667=CARTESIAN_POINT('Ctrl Pts',(-60.7754659560919,-102.946768948967,
178.813912312176));
#22668=CARTESIAN_POINT('Ctrl Pts',(-59.6005562086583,-102.977740948934,
179.985485138407));
#22669=CARTESIAN_POINT('Ctrl Pts',(-57.9430994586544,-103.06015568322,179.985485069079));
#22670=CARTESIAN_POINT('Ctrl Pts',(-56.2856427086505,-103.142570417507,
179.985484999752));
#22671=CARTESIAN_POINT('Ctrl Pts',(-55.1107330587087,-103.17354240708,178.813912075476));
#22672=CARTESIAN_POINT('Ctrl Pts',(-53.935823408767,-103.204514396654,177.6423391512));
#22673=CARTESIAN_POINT('Ctrl Pts',(-53.9258854147871,-103.111292624649,
175.985484901707));
#22674=CARTESIAN_POINT('Ctrl Pts',(-53.9159474208072,-103.018070852645,
174.328630652215));
#22675=CARTESIAN_POINT('Ctrl Pts',(-55.0709810424069,-102.800655323367,
173.157057825983));
#22676=CARTESIAN_POINT('Ctrl Pts',(-56.2260146640065,-102.58323979409,171.985484999752));
#22677=CARTESIAN_POINT('Ctrl Pts',(-57.8635952881763,-102.314381530493,
171.985485069079));
#22678=CARTESIAN_POINT('Ctrl Pts',(-59.5011759123462,-102.045523266896,
171.985485138407));
#22679=CARTESIAN_POINT('Ctrl Pts',(-60.6562094364539,-101.828107748012,
173.157058062683));
#22680=CARTESIAN_POINT('Ctrl Pts',(-61.8112429605617,-101.610692229127,
174.328630986959));
#22681=CARTESIAN_POINT('Ctrl Pts',(-61.8013048287075,-101.517470471821,
175.985485236451));
#22682=CARTESIAN_POINT('Ctrl Pts',(-61.7913666968533,-101.424248714515,
177.642339485944));
#22683=CARTESIAN_POINT('Ctrl Pts',(-60.6164569494197,-101.455220714482,
178.813912312176));
#22684=CARTESIAN_POINT('Ctrl Pts',(-59.4415472019861,-101.486192714449,
179.985485138407));
#22685=CARTESIAN_POINT('Ctrl Pts',(-57.7840904519822,-101.568607448735,
179.985485069079));
#22686=CARTESIAN_POINT('Ctrl Pts',(-56.1266337019783,-101.651022183021,
179.985484999752));
#22687=CARTESIAN_POINT('Ctrl Pts',(-54.9517240520365,-101.681994172595,
178.813912075476));
#22688=CARTESIAN_POINT('Ctrl Pts',(-53.7768144020947,-101.712966162168,
177.6423391512));
#22689=CARTESIAN_POINT('Ctrl Pts',(-53.7668764081149,-101.619744390164,
175.985484901707));
#22690=CARTESIAN_POINT('Ctrl Pts',(-53.756938414135,-101.526522618159,174.328630652215));
#22691=CARTESIAN_POINT('Ctrl Pts',(-54.9119720357346,-101.309107088882,
173.157057825983));
#22692=CARTESIAN_POINT('Ctrl Pts',(-56.0670056573342,-101.091691559604,
171.985484999752));
#22693=CARTESIAN_POINT('Ctrl Pts',(-57.7045862815041,-100.822833296007,
171.985485069079));
#22694=CARTESIAN_POINT('Ctrl Pts',(-59.342166905674,-100.55397503241,171.985485138407));
#22695=CARTESIAN_POINT('Ctrl Pts',(-60.4972004297817,-100.336559513526,
173.157058062683));
#22696=CARTESIAN_POINT('Ctrl Pts',(-61.6522339538895,-100.119143994642,
174.328630986959));
#22697=CARTESIAN_POINT('Ctrl Pts',(-61.6422958220353,-100.025922237336,
175.985485236451));
#22698=CARTESIAN_POINT('Ctrl Pts',(-61.6323576901811,-99.9327004800294,
177.642339485944));
#22699=CARTESIAN_POINT('Ctrl Pts',(-60.4574479427475,-99.9636724799962,
178.813912312176));
#22700=CARTESIAN_POINT('Ctrl Pts',(-59.2825381953138,-99.994644479963,179.985485138407));
#22701=CARTESIAN_POINT('Ctrl Pts',(-57.6250814453099,-100.077059214249,
179.985485069079));
#22702=CARTESIAN_POINT('Ctrl Pts',(-55.9676246953061,-100.159473948536,
179.985484999752));
#22703=CARTESIAN_POINT('Ctrl Pts',(-54.7927150453643,-100.190445938109,
178.813912075476));
#22704=CARTESIAN_POINT('Ctrl Pts',(-53.6178053954225,-100.221417927683,
177.6423391512));
#22705=CARTESIAN_POINT('Ctrl Pts',(-53.6078674014426,-100.128196155678,
175.985484901707));
#22706=CARTESIAN_POINT('Ctrl Pts',(-53.5979294074628,-100.034974383673,
174.328630652215));
#22707=CARTESIAN_POINT('Ctrl Pts',(-54.7529630290624,-99.817558854396,173.157057825983));
#22708=CARTESIAN_POINT('Ctrl Pts',(-55.907996650662,-99.6001433251185,171.985484999752));
#22709=CARTESIAN_POINT('Ctrl Pts',(-57.5455772748319,-99.3312850615215,
171.985485069079));
#22710=CARTESIAN_POINT('Ctrl Pts',(-59.1831578990017,-99.0624267979246,
171.985485138407));
#22711=CARTESIAN_POINT('Ctrl Pts',(-60.3381914231095,-98.8450112790404,
173.157058062683));
#22712=CARTESIAN_POINT('Ctrl Pts',(-61.4932249472172,-98.6275957601562,
174.328630986959));
#22713=CARTESIAN_POINT('Ctrl Pts',(-61.4832868153631,-98.53437400285,175.985485236451));
#22714=CARTESIAN_POINT('Ctrl Pts',(-61.4733486835089,-98.4411522455438,
177.642339485944));
#22715=CARTESIAN_POINT('Ctrl Pts',(-60.2984389360752,-98.4721242455106,
178.813912312176));
#22716=CARTESIAN_POINT('Ctrl Pts',(-59.1235291886416,-98.5030962454774,
179.985485138407));
#22717=CARTESIAN_POINT('Ctrl Pts',(-57.4660724386377,-98.5855109797636,
179.985485069079));
#22718=CARTESIAN_POINT('Ctrl Pts',(-55.8086156886338,-98.6679257140499,
179.985484999752));
#22719=CARTESIAN_POINT('Ctrl Pts',(-54.633706038692,-98.6988977036234,178.813912075476));
#22720=CARTESIAN_POINT('Ctrl Pts',(-56.1707931031902,-113.117197303651,
178.813912075476));
#22721=CARTESIAN_POINT('Ctrl Pts',(-54.9958834532485,-113.148169293224,
177.6423391512));
#22722=CARTESIAN_POINT('Ctrl Pts',(-54.9859454592686,-113.05494752122,175.985484901707));
#22723=CARTESIAN_POINT('Ctrl Pts',(-54.9760074652888,-112.961725749215,
174.328630652215));
#22724=CARTESIAN_POINT('Ctrl Pts',(-56.1310410868884,-112.744310219938,
173.157057825983));
#22725=CARTESIAN_POINT('Ctrl Pts',(-57.286074708488,-112.52689469066,171.985484999752));
#22726=CARTESIAN_POINT('Ctrl Pts',(-58.9236553326578,-112.258036427063,
171.985485069079));
#22727=CARTESIAN_POINT('Ctrl Pts',(-60.5612359568277,-111.989178163466,
171.985485138407));
#22728=CARTESIAN_POINT('Ctrl Pts',(-61.7162694809355,-111.771762644582,
173.157058062683));
#22729=CARTESIAN_POINT('Ctrl Pts',(-62.8713030050432,-111.554347125698,
174.328630986959));
#22730=CARTESIAN_POINT('Ctrl Pts',(-62.861364873189,-111.461125368392,175.985485236451));
#22731=CARTESIAN_POINT('Ctrl Pts',(-62.8514267413349,-111.367903611086,
177.642339485944));
#22732=CARTESIAN_POINT('Ctrl Pts',(-61.6765169939012,-111.398875611052,
178.813912312176));
#22733=CARTESIAN_POINT('Ctrl Pts',(-60.5016072464676,-111.429847611019,
179.985485138407));
#22734=CARTESIAN_POINT('Ctrl Pts',(-58.8441504964637,-111.512262345305,
179.985485069079));
#22735=CARTESIAN_POINT('Ctrl Pts',(-57.1866937464598,-111.594677079592,
179.985484999752));
#22736=CARTESIAN_POINT('Ctrl Pts',(-56.011784096518,-111.625649069165,178.813912075476));
#22737=CARTESIAN_POINT('Ctrl Pts',(-54.8368744465763,-111.656621058739,
177.6423391512));
#22738=CARTESIAN_POINT('Ctrl Pts',(-54.8269364525964,-111.563399286734,
175.985484901707));
#22739=CARTESIAN_POINT('Ctrl Pts',(-54.8169984586165,-111.47017751473,174.328630652215));
#22740=CARTESIAN_POINT('Ctrl Pts',(-55.9720320802161,-111.252761985452,
173.157057825983));
#22741=CARTESIAN_POINT('Ctrl Pts',(-57.1270657018158,-111.035346456175,
171.985484999752));
#22742=CARTESIAN_POINT('Ctrl Pts',(-58.7646463259856,-110.766488192578,
171.985485069079));
#22743=CARTESIAN_POINT('Ctrl Pts',(-60.4022269501555,-110.497629928981,
171.985485138407));
#22744=CARTESIAN_POINT('Ctrl Pts',(-61.5572604742632,-110.280214410097,
173.157058062683));
#22745=CARTESIAN_POINT('Ctrl Pts',(-62.712293998371,-110.062798891212,174.328630986959));
#22746=CARTESIAN_POINT('Ctrl Pts',(-62.7023558665168,-109.969577133906,
175.985485236451));
#22747=CARTESIAN_POINT('Ctrl Pts',(-62.6924177346626,-109.8763553766,177.642339485944));
#22748=CARTESIAN_POINT('Ctrl Pts',(-61.517507987229,-109.907327376567,178.813912312176));
#22749=CARTESIAN_POINT('Ctrl Pts',(-60.3425982397954,-109.938299376534,
179.985485138407));
#22750=CARTESIAN_POINT('Ctrl Pts',(-58.6851414897915,-110.02071411082,179.985485069079));
#22751=CARTESIAN_POINT('Ctrl Pts',(-57.0276847397876,-110.103128845106,
179.985484999752));
#22752=CARTESIAN_POINT('Ctrl Pts',(-55.8527750898458,-110.13410083468,178.813912075476));
#22753=CARTESIAN_POINT('Ctrl Pts',(-54.677865439904,-110.165072824253,177.6423391512));
#22754=CARTESIAN_POINT('Ctrl Pts',(-54.6679274459242,-110.071851052249,
175.985484901707));
#22755=CARTESIAN_POINT('Ctrl Pts',(-54.6579894519443,-109.978629280244,
174.328630652215));
#22756=CARTESIAN_POINT('Ctrl Pts',(-55.8130230735439,-109.761213750967,
173.157057825983));
#22757=CARTESIAN_POINT('Ctrl Pts',(-56.9680566951435,-109.543798221689,
171.985484999752));
#22758=CARTESIAN_POINT('Ctrl Pts',(-58.6056373193134,-109.274939958092,
171.985485069079));
#22759=CARTESIAN_POINT('Ctrl Pts',(-60.2432179434833,-109.006081694495,
171.985485138407));
#22760=CARTESIAN_POINT('Ctrl Pts',(-61.398251467591,-108.788666175611,173.157058062683));
#22761=CARTESIAN_POINT('Ctrl Pts',(-62.5532849916988,-108.571250656727,
174.328630986959));
#22762=CARTESIAN_POINT('Ctrl Pts',(-62.5433468598446,-108.478028899421,
175.985485236451));
#22763=CARTESIAN_POINT('Ctrl Pts',(-62.5334087279904,-108.384807142114,
177.642339485944));
#22764=CARTESIAN_POINT('Ctrl Pts',(-61.3584989805568,-108.415779142081,
178.813912312176));
#22765=CARTESIAN_POINT('Ctrl Pts',(-60.1835892331231,-108.446751142048,
179.985485138407));
#22766=CARTESIAN_POINT('Ctrl Pts',(-58.5261324831192,-108.529165876334,
179.985485069079));
#22767=CARTESIAN_POINT('Ctrl Pts',(-56.8686757331153,-108.611580610621,
179.985484999752));
#22768=CARTESIAN_POINT('Ctrl Pts',(-55.6937660831736,-108.642552600194,
178.813912075476));
#22769=CARTESIAN_POINT('Ctrl Pts',(-54.5188564332318,-108.673524589768,
177.6423391512));
#22770=CARTESIAN_POINT('Ctrl Pts',(-54.5089184392519,-108.580302817763,
175.985484901707));
#22771=CARTESIAN_POINT('Ctrl Pts',(-54.4989804452721,-108.487081045759,
174.328630652215));
#22772=CARTESIAN_POINT('Ctrl Pts',(-55.6540140668717,-108.269665516481,
173.157057825983));
#22773=CARTESIAN_POINT('Ctrl Pts',(-56.8090476884713,-108.052249987204,
171.985484999752));
#22774=CARTESIAN_POINT('Ctrl Pts',(-58.4466283126412,-107.783391723607,
171.985485069079));
#22775=CARTESIAN_POINT('Ctrl Pts',(-60.084208936811,-107.51453346001,171.985485138407));
#22776=CARTESIAN_POINT('Ctrl Pts',(-61.2392424609188,-107.297117941125,
173.157058062683));
#22777=CARTESIAN_POINT('Ctrl Pts',(-62.3942759850265,-107.079702422241,
174.328630986959));
#22778=CARTESIAN_POINT('Ctrl Pts',(-62.3843378531723,-106.986480664935,
175.985485236451));
#22779=CARTESIAN_POINT('Ctrl Pts',(-62.3743997213182,-106.893258907629,
177.642339485944));
#22780=CARTESIAN_POINT('Ctrl Pts',(-61.1994899738845,-106.924230907596,
178.813912312176));
#22781=CARTESIAN_POINT('Ctrl Pts',(-60.0245802264509,-106.955202907562,
179.985485138407));
#22782=CARTESIAN_POINT('Ctrl Pts',(-58.367123476447,-107.037617641849,179.985485069079));
#22783=CARTESIAN_POINT('Ctrl Pts',(-56.7096667264431,-107.120032376135,
179.985484999752));
#22784=CARTESIAN_POINT('Ctrl Pts',(-55.5347570765013,-107.151004365708,
178.813912075476));
#22785=CARTESIAN_POINT('Ctrl Pts',(-54.3598474265596,-107.181976355282,
177.6423391512));
#22786=CARTESIAN_POINT('Ctrl Pts',(-54.3499094325797,-107.088754583277,
175.985484901707));
#22787=CARTESIAN_POINT('Ctrl Pts',(-54.3399714385998,-106.995532811273,
174.328630652215));
#22788=CARTESIAN_POINT('Ctrl Pts',(-55.4950050601995,-106.778117281995,
173.157057825983));
#22789=CARTESIAN_POINT('Ctrl Pts',(-56.6500386817991,-106.560701752718,
171.985484999752));
#22790=CARTESIAN_POINT('Ctrl Pts',(-58.2876193059689,-106.291843489121,
171.985485069079));
#22791=CARTESIAN_POINT('Ctrl Pts',(-59.9251999301388,-106.022985225524,
171.985485138407));
#22792=CARTESIAN_POINT('Ctrl Pts',(-61.0802334542465,-105.80556970664,173.157058062683));
#22793=CARTESIAN_POINT('Ctrl Pts',(-62.2352669783543,-105.588154187756,
174.328630986959));
#22794=CARTESIAN_POINT('Ctrl Pts',(-62.2253288465001,-105.494932430449,
175.985485236451));
#22795=CARTESIAN_POINT('Ctrl Pts',(-62.2153907146459,-105.401710673143,
177.642339485944));
#22796=CARTESIAN_POINT('Ctrl Pts',(-61.0404809672123,-105.43268267311,178.813912312176));
#22797=CARTESIAN_POINT('Ctrl Pts',(-59.8655712197787,-105.463654673077,
179.985485138407));
#22798=CARTESIAN_POINT('Ctrl Pts',(-58.2081144697748,-105.546069407363,
179.985485069079));
#22799=CARTESIAN_POINT('Ctrl Pts',(-56.5506577197709,-105.628484141649,
179.985484999752));
#22800=CARTESIAN_POINT('Ctrl Pts',(-55.3757480698291,-105.659456131223,
178.813912075476));
#22801=CARTESIAN_POINT('Ctrl Pts',(-54.2008384198873,-105.690428120796,
177.6423391512));
#22802=CARTESIAN_POINT('Ctrl Pts',(-54.1909004259075,-105.597206348792,
175.985484901707));
#22803=CARTESIAN_POINT('Ctrl Pts',(-54.1809624319276,-105.503984576787,
174.328630652215));
#22804=CARTESIAN_POINT('Ctrl Pts',(-55.3359960535272,-105.28656904751,173.157057825983));
#22805=CARTESIAN_POINT('Ctrl Pts',(-56.4910296751268,-105.069153518232,
171.985484999752));
#22806=CARTESIAN_POINT('Ctrl Pts',(-58.1286102992967,-104.800295254635,
171.985485069079));
#22807=CARTESIAN_POINT('Ctrl Pts',(-59.7661909234666,-104.531436991038,
171.985485138407));
#22808=CARTESIAN_POINT('Ctrl Pts',(-60.9212244475743,-104.314021472154,
173.157058062683));
#22809=CARTESIAN_POINT('Ctrl Pts',(-62.0762579716821,-104.09660595327,174.328630986959));
#22810=CARTESIAN_POINT('Ctrl Pts',(-62.0663198398279,-104.003384195964,
175.985485236451));
#22811=CARTESIAN_POINT('Ctrl Pts',(-62.0563817079737,-103.910162438658,
177.642339485944));
#22812=CARTESIAN_POINT('Ctrl Pts',(-60.8814719605401,-103.941134438624,
178.813912312176));
#22813=CARTESIAN_POINT('Ctrl Pts',(-59.7065622131064,-103.972106438591,
179.985485138407));
#22814=CARTESIAN_POINT('Ctrl Pts',(-58.0491054631025,-104.054521172878,
179.985485069079));
#22815=CARTESIAN_POINT('Ctrl Pts',(-56.3916487130987,-104.136935907164,
179.985484999752));
#22816=CARTESIAN_POINT('Ctrl Pts',(-55.2167390631569,-104.167907896737,
178.813912075476));
#22817=CARTESIAN_POINT('Ctrl Pts',(-54.0418294132151,-104.198879886311,
177.6423391512));
#22818=CARTESIAN_POINT('Ctrl Pts',(-54.0318914192353,-104.105658114306,
175.985484901707));
#22819=CARTESIAN_POINT('Ctrl Pts',(-54.0219534252554,-104.012436342302,
174.328630652215));
#22820=CARTESIAN_POINT('Ctrl Pts',(-55.176987046855,-103.795020813024,173.157057825983));
#22821=CARTESIAN_POINT('Ctrl Pts',(-56.3320206684546,-103.577605283747,
171.985484999752));
#22822=CARTESIAN_POINT('Ctrl Pts',(-57.9696012926245,-103.30874702015,171.985485069079));
#22823=CARTESIAN_POINT('Ctrl Pts',(-59.6071819167943,-103.039888756553,
171.985485138407));
#22824=CARTESIAN_POINT('Ctrl Pts',(-60.7622154409021,-102.822473237669,
173.157058062683));
#22825=CARTESIAN_POINT('Ctrl Pts',(-61.9172489650099,-102.605057718784,
174.328630986959));
#22826=CARTESIAN_POINT('Ctrl Pts',(-61.9073108331557,-102.511835961478,
175.985485236451));
#22827=CARTESIAN_POINT('Ctrl Pts',(-61.8973727013015,-102.418614204172,
177.642339485944));
#22828=CARTESIAN_POINT('Ctrl Pts',(-60.7224629538678,-102.449586204139,
178.813912312176));
#22829=CARTESIAN_POINT('Ctrl Pts',(-59.5475532064342,-102.480558204106,
179.985485138407));
#22830=CARTESIAN_POINT('Ctrl Pts',(-57.8900964564303,-102.562972938392,
179.985485069079));
#22831=CARTESIAN_POINT('Ctrl Pts',(-56.2326397064264,-102.645387672678,
179.985484999752));
#22832=CARTESIAN_POINT('Ctrl Pts',(-55.0577300564847,-102.676359662252,
178.813912075476));
#22833=CARTESIAN_POINT('Ctrl Pts',(-53.8828204065429,-102.707331651825,
177.6423391512));
#22834=CARTESIAN_POINT('Ctrl Pts',(-53.872882412563,-102.614109879821,175.985484901707));
#22835=CARTESIAN_POINT('Ctrl Pts',(-53.8629444185832,-102.520888107816,
174.328630652215));
#22836=CARTESIAN_POINT('Ctrl Pts',(-55.0179780401828,-102.303472578539,
173.157057825983));
#22837=CARTESIAN_POINT('Ctrl Pts',(-56.1730116617824,-102.086057049261,
171.985484999752));
#22838=CARTESIAN_POINT('Ctrl Pts',(-57.8105922859523,-101.817198785664,
171.985485069079));
#22839=CARTESIAN_POINT('Ctrl Pts',(-59.4481729101221,-101.548340522067,
171.985485138407));
#22840=CARTESIAN_POINT('Ctrl Pts',(-60.6032064342299,-101.330925003183,
173.157058062683));
#22841=CARTESIAN_POINT('Ctrl Pts',(-61.7582399583376,-101.113509484299,
174.328630986959));
#22842=CARTESIAN_POINT('Ctrl Pts',(-61.7483018264834,-101.020287726993,
175.985485236451));
#22843=CARTESIAN_POINT('Ctrl Pts',(-61.7383636946293,-100.927065969686,
177.642339485944));
#22844=CARTESIAN_POINT('Ctrl Pts',(-60.5634539471956,-100.958037969653,
178.813912312176));
#22845=CARTESIAN_POINT('Ctrl Pts',(-59.388544199762,-100.98900996962,179.985485138407));
#22846=CARTESIAN_POINT('Ctrl Pts',(-57.7310874497581,-101.071424703906,
179.985485069079));
#22847=CARTESIAN_POINT('Ctrl Pts',(-56.0736306997542,-101.153839438193,
179.985484999752));
#22848=CARTESIAN_POINT('Ctrl Pts',(-54.8987210498124,-101.184811427766,
178.813912075476));
#22849=CARTESIAN_POINT('Ctrl Pts',(-53.7238113998707,-101.21578341734,177.6423391512));
#22850=CARTESIAN_POINT('Ctrl Pts',(-53.7138734058908,-101.122561645335,
175.985484901707));
#22851=CARTESIAN_POINT('Ctrl Pts',(-53.7039354119109,-101.029339873331,
174.328630652215));
#22852=CARTESIAN_POINT('Ctrl Pts',(-54.8589690335105,-100.811924344053,
173.157057825983));
#22853=CARTESIAN_POINT('Ctrl Pts',(-56.0140026551102,-100.594508814776,
171.985484999752));
#22854=CARTESIAN_POINT('Ctrl Pts',(-57.65158327928,-100.325650551179,171.985485069079));
#22855=CARTESIAN_POINT('Ctrl Pts',(-59.2891639034499,-100.056792287582,
171.985485138407));
#22856=CARTESIAN_POINT('Ctrl Pts',(-60.4441974275576,-99.8393767686974,
173.157058062683));
#22857=CARTESIAN_POINT('Ctrl Pts',(-61.5992309516654,-99.6219612498133,
174.328630986959));
#22858=CARTESIAN_POINT('Ctrl Pts',(-61.5892928198112,-99.528739492507,175.985485236451));
#22859=CARTESIAN_POINT('Ctrl Pts',(-61.579354687957,-99.4355177352008,177.642339485944));
#22860=CARTESIAN_POINT('Ctrl Pts',(-60.4044449405234,-99.4664897351676,
178.813912312176));
#22861=CARTESIAN_POINT('Ctrl Pts',(-59.2295351930898,-99.4974617351344,
179.985485138407));
#22862=CARTESIAN_POINT('Ctrl Pts',(-57.5720784430859,-99.5798764694207,
179.985485069079));
#22863=CARTESIAN_POINT('Ctrl Pts',(-55.914621693082,-99.662291203707,179.985484999752));
#22864=CARTESIAN_POINT('Ctrl Pts',(-54.7397120431402,-99.6932631932805,
178.813912075476));
#22865=CARTESIAN_POINT('Ctrl Pts',(-53.5648023931984,-99.724235182854,177.6423391512));
#22866=CARTESIAN_POINT('Ctrl Pts',(-53.5548643992186,-99.6310134108495,
175.985484901707));
#22867=CARTESIAN_POINT('Ctrl Pts',(-53.5449264052387,-99.5377916388449,
174.328630652215));
#22868=CARTESIAN_POINT('Ctrl Pts',(-54.6999600268383,-99.3203761095675,
173.157057825983));
#22869=CARTESIAN_POINT('Ctrl Pts',(-55.8549936484379,-99.10296058029,171.985484999752));
#22870=CARTESIAN_POINT('Ctrl Pts',(-57.4925742726078,-98.834102316693,171.985485069079));
#22871=CARTESIAN_POINT('Ctrl Pts',(-59.1301548967777,-98.5652440530961,
171.985485138407));
#22872=CARTESIAN_POINT('Ctrl Pts',(-60.2851884208854,-98.3478285342118,
173.157058062683));
#22873=CARTESIAN_POINT('Ctrl Pts',(-61.4402219449932,-98.1304130153276,
174.328630986959));
#22874=CARTESIAN_POINT('Ctrl Pts',(-61.430283813139,-98.0371912580215,175.985485236451));
#22875=CARTESIAN_POINT('Ctrl Pts',(-61.4203456812848,-97.9439695007152,
177.642339485944));
#22876=CARTESIAN_POINT('Ctrl Pts',(-60.2454359338512,-97.974941500682,178.813912312176));
#22877=CARTESIAN_POINT('Ctrl Pts',(-59.0705261864175,-98.0059135006488,
179.985485138407));
#22878=CARTESIAN_POINT('Ctrl Pts',(-57.4130694364136,-98.0883282349351,
179.985485069079));
#22879=CARTESIAN_POINT('Ctrl Pts',(-55.7556126864097,-98.1707429692214,
179.985484999752));
#22880=CARTESIAN_POINT('Ctrl Pts',(-54.580703036468,-98.2017149587949,178.813912075476));
#22881=CARTESIAN_POINT('Ctrl Pts',(-56.181115489574,-113.283598570176,178.821287383467));
#22882=CARTESIAN_POINT('Ctrl Pts',(-55.0031681001975,-113.314894403068,
177.646659506339));
#22883=CARTESIAN_POINT('Ctrl Pts',(-54.9932301063974,-113.221672631044,
175.985484901271));
#22884=CARTESIAN_POINT('Ctrl Pts',(-54.9832921125973,-113.12845085902,174.324310296203));
#22885=CARTESIAN_POINT('Ctrl Pts',(-56.1413634738858,-112.910711486397,
173.149682517375));
#22886=CARTESIAN_POINT('Ctrl Pts',(-57.2994348351743,-112.692972113774,
171.975054738546));
#22887=CARTESIAN_POINT('Ctrl Pts',(-58.9413114718314,-112.423655866545,
171.975054808055));
#22888=CARTESIAN_POINT('Ctrl Pts',(-60.5831881084886,-112.154339619316,
171.975054877564));
#22889=CARTESIAN_POINT('Ctrl Pts',(-61.741259372031,-111.936600257113,173.149682754692));
#22890=CARTESIAN_POINT('Ctrl Pts',(-62.8993306355734,-111.71886089491,174.32431063182));
#22891=CARTESIAN_POINT('Ctrl Pts',(-62.8893925035395,-111.625639137623,
175.985485236888));
#22892=CARTESIAN_POINT('Ctrl Pts',(-62.8794543715055,-111.532417380336,
177.646659841956));
#22893=CARTESIAN_POINT('Ctrl Pts',(-61.701506884383,-111.563713223648,178.821287620784));
#22894=CARTESIAN_POINT('Ctrl Pts',(-60.5235593972605,-111.595009066961,
179.995915399612));
#22895=CARTESIAN_POINT('Ctrl Pts',(-58.8618066347693,-111.677881784879,
179.995915330104));
#22896=CARTESIAN_POINT('Ctrl Pts',(-57.2000538722782,-111.760754502798,
179.995915260595));
#22897=CARTESIAN_POINT('Ctrl Pts',(-56.0221064829017,-111.79205033569,178.821287383467));
#22898=CARTESIAN_POINT('Ctrl Pts',(-54.8441590935253,-111.823346168582,
177.646659506339));
#22899=CARTESIAN_POINT('Ctrl Pts',(-54.8342210997252,-111.730124396559,
175.985484901271));
#22900=CARTESIAN_POINT('Ctrl Pts',(-54.8242831059251,-111.636902624535,
174.324310296203));
#22901=CARTESIAN_POINT('Ctrl Pts',(-55.9823544672136,-111.419163251912,
173.149682517375));
#22902=CARTESIAN_POINT('Ctrl Pts',(-57.1404258285021,-111.201423879289,
171.975054738546));
#22903=CARTESIAN_POINT('Ctrl Pts',(-58.7823024651592,-110.932107632059,
171.975054808055));
#22904=CARTESIAN_POINT('Ctrl Pts',(-60.4241791018163,-110.66279138483,171.975054877564));
#22905=CARTESIAN_POINT('Ctrl Pts',(-61.5822503653587,-110.445052022627,
173.149682754692));
#22906=CARTESIAN_POINT('Ctrl Pts',(-62.7403216289012,-110.227312660424,
174.32431063182));
#22907=CARTESIAN_POINT('Ctrl Pts',(-62.7303834968672,-110.134090903137,
175.985485236888));
#22908=CARTESIAN_POINT('Ctrl Pts',(-62.7204453648333,-110.04086914585,177.646659841956));
#22909=CARTESIAN_POINT('Ctrl Pts',(-61.5424978777108,-110.072164989163,
178.821287620784));
#22910=CARTESIAN_POINT('Ctrl Pts',(-60.3645503905882,-110.103460832475,
179.995915399612));
#22911=CARTESIAN_POINT('Ctrl Pts',(-58.7027976280971,-110.186333550394,
179.995915330104));
#22912=CARTESIAN_POINT('Ctrl Pts',(-57.041044865606,-110.269206268313,179.995915260595));
#22913=CARTESIAN_POINT('Ctrl Pts',(-55.8630974762295,-110.300502101205,
178.821287383467));
#22914=CARTESIAN_POINT('Ctrl Pts',(-54.6851500868531,-110.331797934097,
177.646659506339));
#22915=CARTESIAN_POINT('Ctrl Pts',(-54.675212093053,-110.238576162073,175.985484901271));
#22916=CARTESIAN_POINT('Ctrl Pts',(-54.6652740992529,-110.145354390049,
174.324310296203));
#22917=CARTESIAN_POINT('Ctrl Pts',(-55.8233454605414,-109.927615017426,
173.149682517375));
#22918=CARTESIAN_POINT('Ctrl Pts',(-56.9814168218299,-109.709875644803,
171.975054738546));
#22919=CARTESIAN_POINT('Ctrl Pts',(-58.623293458487,-109.440559397574,171.975054808055));
#22920=CARTESIAN_POINT('Ctrl Pts',(-60.2651700951441,-109.171243150344,
171.975054877564));
#22921=CARTESIAN_POINT('Ctrl Pts',(-61.4232413586865,-108.953503788142,
173.149682754692));
#22922=CARTESIAN_POINT('Ctrl Pts',(-62.581312622229,-108.735764425939,174.32431063182));
#22923=CARTESIAN_POINT('Ctrl Pts',(-62.571374490195,-108.642542668652,175.985485236888));
#22924=CARTESIAN_POINT('Ctrl Pts',(-62.5614363581611,-108.549320911365,
177.646659841956));
#22925=CARTESIAN_POINT('Ctrl Pts',(-61.3834888710385,-108.580616754677,
178.821287620784));
#22926=CARTESIAN_POINT('Ctrl Pts',(-60.205541383916,-108.61191259799,179.995915399612));
#22927=CARTESIAN_POINT('Ctrl Pts',(-58.5437886214249,-108.694785315908,
179.995915330104));
#22928=CARTESIAN_POINT('Ctrl Pts',(-56.8820358589338,-108.777658033827,
179.995915260595));
#22929=CARTESIAN_POINT('Ctrl Pts',(-55.7040884695573,-108.808953866719,
178.821287383467));
#22930=CARTESIAN_POINT('Ctrl Pts',(-54.5261410801808,-108.840249699611,
177.646659506339));
#22931=CARTESIAN_POINT('Ctrl Pts',(-54.5162030863807,-108.747027927587,
175.985484901271));
#22932=CARTESIAN_POINT('Ctrl Pts',(-54.5062650925806,-108.653806155564,
174.324310296203));
#22933=CARTESIAN_POINT('Ctrl Pts',(-55.6643364538691,-108.436066782941,
173.149682517375));
#22934=CARTESIAN_POINT('Ctrl Pts',(-56.8224078151577,-108.218327410317,
171.975054738546));
#22935=CARTESIAN_POINT('Ctrl Pts',(-58.4642844518147,-107.949011163088,
171.975054808055));
#22936=CARTESIAN_POINT('Ctrl Pts',(-60.1061610884719,-107.679694915859,
171.975054877564));
#22937=CARTESIAN_POINT('Ctrl Pts',(-61.2642323520143,-107.461955553656,
173.149682754692));
#22938=CARTESIAN_POINT('Ctrl Pts',(-62.4223036155567,-107.244216191453,
174.32431063182));
#22939=CARTESIAN_POINT('Ctrl Pts',(-62.4123654835228,-107.150994434166,
175.985485236888));
#22940=CARTESIAN_POINT('Ctrl Pts',(-62.4024273514889,-107.057772676879,
177.646659841956));
#22941=CARTESIAN_POINT('Ctrl Pts',(-61.2244798643663,-107.089068520192,
178.821287620784));
#22942=CARTESIAN_POINT('Ctrl Pts',(-60.0465323772438,-107.120364363504,
179.995915399612));
#22943=CARTESIAN_POINT('Ctrl Pts',(-58.3847796147526,-107.203237081423,
179.995915330104));
#22944=CARTESIAN_POINT('Ctrl Pts',(-56.7230268522615,-107.286109799341,
179.995915260595));
#22945=CARTESIAN_POINT('Ctrl Pts',(-55.5450794628851,-107.317405632233,
178.821287383467));
#22946=CARTESIAN_POINT('Ctrl Pts',(-54.3671320735086,-107.348701465125,
177.646659506339));
#22947=CARTESIAN_POINT('Ctrl Pts',(-54.3571940797085,-107.255479693102,
175.985484901271));
#22948=CARTESIAN_POINT('Ctrl Pts',(-54.3472560859084,-107.162257921078,
174.324310296203));
#22949=CARTESIAN_POINT('Ctrl Pts',(-55.5053274471969,-106.944518548455,
173.149682517375));
#22950=CARTESIAN_POINT('Ctrl Pts',(-56.6633988084854,-106.726779175832,
171.975054738546));
#22951=CARTESIAN_POINT('Ctrl Pts',(-58.3052754451425,-106.457462928602,
171.975054808055));
#22952=CARTESIAN_POINT('Ctrl Pts',(-59.9471520817997,-106.188146681373,
171.975054877564));
#22953=CARTESIAN_POINT('Ctrl Pts',(-61.1052233453421,-105.97040731917,173.149682754692));
#22954=CARTESIAN_POINT('Ctrl Pts',(-62.2632946088845,-105.752667956968,
174.32431063182));
#22955=CARTESIAN_POINT('Ctrl Pts',(-62.2533564768505,-105.659446199681,
175.985485236888));
#22956=CARTESIAN_POINT('Ctrl Pts',(-62.2434183448166,-105.566224442394,
177.646659841956));
#22957=CARTESIAN_POINT('Ctrl Pts',(-61.0654708576941,-105.597520285706,
178.821287620784));
#22958=CARTESIAN_POINT('Ctrl Pts',(-59.8875233705716,-105.628816129018,
179.995915399612));
#22959=CARTESIAN_POINT('Ctrl Pts',(-58.2257706080804,-105.711688846937,
179.995915330104));
#22960=CARTESIAN_POINT('Ctrl Pts',(-56.5640178455893,-105.794561564856,
179.995915260595));
#22961=CARTESIAN_POINT('Ctrl Pts',(-55.3860704562128,-105.825857397748,
178.821287383467));
#22962=CARTESIAN_POINT('Ctrl Pts',(-54.2081230668364,-105.85715323064,177.646659506339));
#22963=CARTESIAN_POINT('Ctrl Pts',(-54.1981850730363,-105.763931458616,
175.985484901271));
#22964=CARTESIAN_POINT('Ctrl Pts',(-54.1882470792362,-105.670709686593,
174.324310296203));
#22965=CARTESIAN_POINT('Ctrl Pts',(-55.3463184405247,-105.452970313969,
173.149682517375));
#22966=CARTESIAN_POINT('Ctrl Pts',(-56.5043898018132,-105.235230941346,
171.975054738546));
#22967=CARTESIAN_POINT('Ctrl Pts',(-58.1462664384703,-104.965914694117,
171.975054808055));
#22968=CARTESIAN_POINT('Ctrl Pts',(-59.7881430751274,-104.696598446888,
171.975054877564));
#22969=CARTESIAN_POINT('Ctrl Pts',(-60.9462143386698,-104.478859084685,
173.149682754692));
#22970=CARTESIAN_POINT('Ctrl Pts',(-62.1042856022123,-104.261119722482,
174.32431063182));
#22971=CARTESIAN_POINT('Ctrl Pts',(-62.0943474701783,-104.167897965195,
175.985485236888));
#22972=CARTESIAN_POINT('Ctrl Pts',(-62.0844093381444,-104.074676207908,
177.646659841956));
#22973=CARTESIAN_POINT('Ctrl Pts',(-60.9064618510219,-104.10597205122,178.821287620784));
#22974=CARTESIAN_POINT('Ctrl Pts',(-59.7285143638993,-104.137267894533,
179.995915399612));
#22975=CARTESIAN_POINT('Ctrl Pts',(-58.0667616014082,-104.220140612451,
179.995915330104));
#22976=CARTESIAN_POINT('Ctrl Pts',(-56.4050088389171,-104.30301333037,179.995915260595));
#22977=CARTESIAN_POINT('Ctrl Pts',(-55.2270614495406,-104.334309163262,
178.821287383467));
#22978=CARTESIAN_POINT('Ctrl Pts',(-54.0491140601642,-104.365604996154,
177.646659506339));
#22979=CARTESIAN_POINT('Ctrl Pts',(-54.039176066364,-104.272383224131,175.985484901271));
#22980=CARTESIAN_POINT('Ctrl Pts',(-54.029238072564,-104.179161452107,174.324310296203));
#22981=CARTESIAN_POINT('Ctrl Pts',(-55.1873094338524,-103.961422079484,
173.149682517375));
#22982=CARTESIAN_POINT('Ctrl Pts',(-56.345380795141,-103.743682706861,171.975054738546));
#22983=CARTESIAN_POINT('Ctrl Pts',(-57.9872574317981,-103.474366459631,
171.975054808055));
#22984=CARTESIAN_POINT('Ctrl Pts',(-59.6291340684552,-103.205050212402,
171.975054877564));
#22985=CARTESIAN_POINT('Ctrl Pts',(-60.7872053319976,-102.987310850199,
173.149682754692));
#22986=CARTESIAN_POINT('Ctrl Pts',(-61.94527659554,-102.769571487996,174.32431063182));
#22987=CARTESIAN_POINT('Ctrl Pts',(-61.9353384635061,-102.676349730709,
175.985485236888));
#22988=CARTESIAN_POINT('Ctrl Pts',(-61.9254003314722,-102.583127973422,
177.646659841956));
#22989=CARTESIAN_POINT('Ctrl Pts',(-60.7474528443496,-102.614423816735,
178.821287620784));
#22990=CARTESIAN_POINT('Ctrl Pts',(-59.5695053572271,-102.645719660047,
179.995915399612));
#22991=CARTESIAN_POINT('Ctrl Pts',(-57.907752594736,-102.728592377966,179.995915330104));
#22992=CARTESIAN_POINT('Ctrl Pts',(-56.2459998322448,-102.811465095885,
179.995915260595));
#22993=CARTESIAN_POINT('Ctrl Pts',(-55.0680524428684,-102.842760928777,
178.821287383467));
#22994=CARTESIAN_POINT('Ctrl Pts',(-53.8901050534919,-102.874056761669,
177.646659506339));
#22995=CARTESIAN_POINT('Ctrl Pts',(-53.8801670596918,-102.780834989645,
175.985484901271));
#22996=CARTESIAN_POINT('Ctrl Pts',(-53.8702290658917,-102.687613217621,
174.324310296203));
#22997=CARTESIAN_POINT('Ctrl Pts',(-55.0283004271802,-102.469873844998,
173.149682517375));
#22998=CARTESIAN_POINT('Ctrl Pts',(-56.1863717884687,-102.252134472375,
171.975054738546));
#22999=CARTESIAN_POINT('Ctrl Pts',(-57.8282484251258,-101.982818225146,
171.975054808055));
#23000=CARTESIAN_POINT('Ctrl Pts',(-59.470125061783,-101.713501977916,171.975054877564));
#23001=CARTESIAN_POINT('Ctrl Pts',(-60.6281963253254,-101.495762615714,
173.149682754692));
#23002=CARTESIAN_POINT('Ctrl Pts',(-61.7862675888678,-101.278023253511,
174.32431063182));
#23003=CARTESIAN_POINT('Ctrl Pts',(-61.7763294568339,-101.184801496224,
175.985485236888));
#23004=CARTESIAN_POINT('Ctrl Pts',(-61.7663913247999,-101.091579738937,
177.646659841956));
#23005=CARTESIAN_POINT('Ctrl Pts',(-60.5884438376774,-101.122875582249,
178.821287620784));
#23006=CARTESIAN_POINT('Ctrl Pts',(-59.4104963505549,-101.154171425562,
179.995915399612));
#23007=CARTESIAN_POINT('Ctrl Pts',(-57.7487435880637,-101.23704414348,179.995915330104));
#23008=CARTESIAN_POINT('Ctrl Pts',(-56.0869908255726,-101.319916861399,
179.995915260595));
#23009=CARTESIAN_POINT('Ctrl Pts',(-54.9090434361961,-101.351212694291,
178.821287383467));
#23010=CARTESIAN_POINT('Ctrl Pts',(-53.7310960468197,-101.382508527183,
177.646659506339));
#23011=CARTESIAN_POINT('Ctrl Pts',(-53.7211580530196,-101.289286755159,
175.985484901271));
#23012=CARTESIAN_POINT('Ctrl Pts',(-53.7112200592195,-101.196064983136,
174.324310296203));
#23013=CARTESIAN_POINT('Ctrl Pts',(-54.869291420508,-100.978325610513,173.149682517375));
#23014=CARTESIAN_POINT('Ctrl Pts',(-56.0273627817965,-100.760586237889,
171.975054738546));
#23015=CARTESIAN_POINT('Ctrl Pts',(-57.6692394184536,-100.49126999066,171.975054808055));
#23016=CARTESIAN_POINT('Ctrl Pts',(-59.3111160551107,-100.221953743431,
171.975054877564));
#23017=CARTESIAN_POINT('Ctrl Pts',(-60.4691873186531,-100.004214381228,
173.149682754692));
#23018=CARTESIAN_POINT('Ctrl Pts',(-61.6272585821956,-99.7864750190253,
174.32431063182));
#23019=CARTESIAN_POINT('Ctrl Pts',(-61.6173204501616,-99.6932532617382,
175.985485236888));
#23020=CARTESIAN_POINT('Ctrl Pts',(-61.6073823181277,-99.6000315044512,
177.646659841956));
#23021=CARTESIAN_POINT('Ctrl Pts',(-60.4294348310052,-99.6313273477637,
178.821287620784));
#23022=CARTESIAN_POINT('Ctrl Pts',(-59.2514873438827,-99.6626231910761,
179.995915399612));
#23023=CARTESIAN_POINT('Ctrl Pts',(-57.5897345813915,-99.7454959089947,
179.995915330104));
#23024=CARTESIAN_POINT('Ctrl Pts',(-55.9279818189004,-99.8283686269133,
179.995915260595));
#23025=CARTESIAN_POINT('Ctrl Pts',(-54.7500344295239,-99.8596644598054,
178.821287383467));
#23026=CARTESIAN_POINT('Ctrl Pts',(-53.5720870401475,-99.8909602926975,
177.646659506339));
#23027=CARTESIAN_POINT('Ctrl Pts',(-53.5621490463474,-99.7977385206737,
175.985484901271));
#23028=CARTESIAN_POINT('Ctrl Pts',(-53.5522110525473,-99.7045167486501,
174.324310296203));
#23029=CARTESIAN_POINT('Ctrl Pts',(-54.7102824138358,-99.4867773760269,
173.149682517375));
#23030=CARTESIAN_POINT('Ctrl Pts',(-55.8683537751243,-99.2690380034038,
171.975054738546));
#23031=CARTESIAN_POINT('Ctrl Pts',(-57.5102304117814,-98.9997217561745,
171.975054808055));
#23032=CARTESIAN_POINT('Ctrl Pts',(-59.1521070484385,-98.7304055089452,
171.975054877564));
#23033=CARTESIAN_POINT('Ctrl Pts',(-60.3101783119809,-98.5126661467424,
173.149682754692));
#23034=CARTESIAN_POINT('Ctrl Pts',(-61.4682495755234,-98.2949267845397,
174.32431063182));
#23035=CARTESIAN_POINT('Ctrl Pts',(-61.4583114434894,-98.2017050272526,
175.985485236888));
#23036=CARTESIAN_POINT('Ctrl Pts',(-61.4483733114555,-98.1084832699656,
177.646659841956));
#23037=CARTESIAN_POINT('Ctrl Pts',(-60.2704258243329,-98.139779113278,178.821287620784));
#23038=CARTESIAN_POINT('Ctrl Pts',(-59.0924783372104,-98.1710749565905,
179.995915399612));
#23039=CARTESIAN_POINT('Ctrl Pts',(-57.4307255747193,-98.2539476745091,
179.995915330104));
#23040=CARTESIAN_POINT('Ctrl Pts',(-55.7689728122282,-98.3368203924277,
179.995915260595));
#23041=CARTESIAN_POINT('Ctrl Pts',(-54.5910254228517,-98.3681162253198,
178.821287383467));
#23042=CARTESIAN_POINT('Ctrl Pts',(-56.1988062143188,-113.449542435949,
178.821287383467));
#23043=CARTESIAN_POINT('Ctrl Pts',(-55.0208588249424,-113.480838268841,
177.646659506339));
#23044=CARTESIAN_POINT('Ctrl Pts',(-55.0109208311422,-113.387616496817,
175.985484901271));
#23045=CARTESIAN_POINT('Ctrl Pts',(-55.0009828373422,-113.294394724794,
174.324310296203));
#23046=CARTESIAN_POINT('Ctrl Pts',(-56.1590541986307,-113.07665535217,173.149682517375));
#23047=CARTESIAN_POINT('Ctrl Pts',(-57.3171255599192,-112.858915979547,
171.975054738546));
#23048=CARTESIAN_POINT('Ctrl Pts',(-58.9590021965763,-112.589599732318,
171.975054808055));
#23049=CARTESIAN_POINT('Ctrl Pts',(-60.6008788332334,-112.320283485089,
171.975054877564));
#23050=CARTESIAN_POINT('Ctrl Pts',(-61.7589500967758,-112.102544122886,
173.149682754692));
#23051=CARTESIAN_POINT('Ctrl Pts',(-62.9170213603182,-111.884804760683,
174.32431063182));
#23052=CARTESIAN_POINT('Ctrl Pts',(-62.9070832282843,-111.791583003396,
175.985485236888));
#23053=CARTESIAN_POINT('Ctrl Pts',(-62.8971450962504,-111.698361246109,
177.646659841956));
#23054=CARTESIAN_POINT('Ctrl Pts',(-61.7191976091278,-111.729657089422,
178.821287620784));
#23055=CARTESIAN_POINT('Ctrl Pts',(-60.5412501220053,-111.760952932734,
179.995915399612));
#23056=CARTESIAN_POINT('Ctrl Pts',(-58.8794973595142,-111.843825650653,
179.995915330104));
#23057=CARTESIAN_POINT('Ctrl Pts',(-57.217744597023,-111.926698368571,179.995915260595));
#23058=CARTESIAN_POINT('Ctrl Pts',(-56.0397972076466,-111.957994201463,
178.821287383467));
#23059=CARTESIAN_POINT('Ctrl Pts',(-54.8618498182701,-111.989290034355,
177.646659506339));
#23060=CARTESIAN_POINT('Ctrl Pts',(-54.85191182447,-111.896068262332,175.985484901271));
#23061=CARTESIAN_POINT('Ctrl Pts',(-54.8419738306699,-111.802846490308,
174.324310296203));
#23062=CARTESIAN_POINT('Ctrl Pts',(-56.0000451919584,-111.585107117685,
173.149682517375));
#23063=CARTESIAN_POINT('Ctrl Pts',(-57.158116553247,-111.367367745062,171.975054738546));
#23064=CARTESIAN_POINT('Ctrl Pts',(-58.799993189904,-111.098051497832,171.975054808055));
#23065=CARTESIAN_POINT('Ctrl Pts',(-60.4418698265612,-110.828735250603,
171.975054877564));
#23066=CARTESIAN_POINT('Ctrl Pts',(-61.5999410901036,-110.6109958884,173.149682754692));
#23067=CARTESIAN_POINT('Ctrl Pts',(-62.758012353646,-110.393256526198,174.32431063182));
#23068=CARTESIAN_POINT('Ctrl Pts',(-62.7480742216121,-110.30003476891,175.985485236888));
#23069=CARTESIAN_POINT('Ctrl Pts',(-62.7381360895782,-110.206813011623,
177.646659841956));
#23070=CARTESIAN_POINT('Ctrl Pts',(-61.5601886024556,-110.238108854936,
178.821287620784));
#23071=CARTESIAN_POINT('Ctrl Pts',(-60.3822411153331,-110.269404698248,
179.995915399612));
#23072=CARTESIAN_POINT('Ctrl Pts',(-58.7204883528419,-110.352277416167,
179.995915330104));
#23073=CARTESIAN_POINT('Ctrl Pts',(-57.0587355903508,-110.435150134086,
179.995915260595));
#23074=CARTESIAN_POINT('Ctrl Pts',(-55.8807882009743,-110.466445966978,
178.821287383467));
#23075=CARTESIAN_POINT('Ctrl Pts',(-54.7028408115979,-110.49774179987,177.646659506339));
#23076=CARTESIAN_POINT('Ctrl Pts',(-54.6929028177978,-110.404520027846,
175.985484901271));
#23077=CARTESIAN_POINT('Ctrl Pts',(-54.6829648239977,-110.311298255822,
174.324310296203));
#23078=CARTESIAN_POINT('Ctrl Pts',(-55.8410361852862,-110.093558883199,
173.149682517375));
#23079=CARTESIAN_POINT('Ctrl Pts',(-56.9991075465747,-109.875819510576,
171.975054738546));
#23080=CARTESIAN_POINT('Ctrl Pts',(-58.6409841832318,-109.606503263347,
171.975054808055));
#23081=CARTESIAN_POINT('Ctrl Pts',(-60.2828608198889,-109.337187016117,
171.975054877564));
#23082=CARTESIAN_POINT('Ctrl Pts',(-61.4409320834313,-109.119447653915,
173.149682754692));
#23083=CARTESIAN_POINT('Ctrl Pts',(-62.5990033469738,-108.901708291712,
174.32431063182));
#23084=CARTESIAN_POINT('Ctrl Pts',(-62.5890652149398,-108.808486534425,
175.985485236888));
#23085=CARTESIAN_POINT('Ctrl Pts',(-62.5791270829059,-108.715264777138,
177.646659841956));
#23086=CARTESIAN_POINT('Ctrl Pts',(-61.4011795957834,-108.74656062045,178.821287620784));
#23087=CARTESIAN_POINT('Ctrl Pts',(-60.2232321086609,-108.777856463763,
179.995915399612));
#23088=CARTESIAN_POINT('Ctrl Pts',(-58.5614793461697,-108.860729181681,
179.995915330104));
#23089=CARTESIAN_POINT('Ctrl Pts',(-56.8997265836786,-108.9436018996,179.995915260595));
#23090=CARTESIAN_POINT('Ctrl Pts',(-55.7217791943021,-108.974897732492,
178.821287383467));
#23091=CARTESIAN_POINT('Ctrl Pts',(-54.5438318049257,-109.006193565384,
177.646659506339));
#23092=CARTESIAN_POINT('Ctrl Pts',(-54.5338938111256,-108.91297179336,175.985484901271));
#23093=CARTESIAN_POINT('Ctrl Pts',(-54.5239558173255,-108.819750021337,
174.324310296203));
#23094=CARTESIAN_POINT('Ctrl Pts',(-55.682027178614,-108.602010648714,173.149682517375));
#23095=CARTESIAN_POINT('Ctrl Pts',(-56.8400985399025,-108.384271276091,
171.975054738546));
#23096=CARTESIAN_POINT('Ctrl Pts',(-58.4819751765596,-108.114955028861,
171.975054808055));
#23097=CARTESIAN_POINT('Ctrl Pts',(-60.1238518132167,-107.845638781632,
171.975054877564));
#23098=CARTESIAN_POINT('Ctrl Pts',(-61.2819230767591,-107.627899419429,
173.149682754692));
#23099=CARTESIAN_POINT('Ctrl Pts',(-62.4399943403016,-107.410160057226,
174.32431063182));
#23100=CARTESIAN_POINT('Ctrl Pts',(-62.4300562082676,-107.316938299939,
175.985485236888));
#23101=CARTESIAN_POINT('Ctrl Pts',(-62.4201180762337,-107.223716542652,
177.646659841956));
#23102=CARTESIAN_POINT('Ctrl Pts',(-61.2421705891111,-107.255012385965,
178.821287620784));
#23103=CARTESIAN_POINT('Ctrl Pts',(-60.0642231019886,-107.286308229277,
179.995915399612));
#23104=CARTESIAN_POINT('Ctrl Pts',(-58.4024703394975,-107.369180947196,
179.995915330104));
#23105=CARTESIAN_POINT('Ctrl Pts',(-56.7407175770064,-107.452053665114,
179.995915260595));
#23106=CARTESIAN_POINT('Ctrl Pts',(-55.5627701876299,-107.483349498006,
178.821287383467));
#23107=CARTESIAN_POINT('Ctrl Pts',(-54.3848227982534,-107.514645330899,
177.646659506339));
#23108=CARTESIAN_POINT('Ctrl Pts',(-54.3748848044533,-107.421423558875,
175.985484901271));
#23109=CARTESIAN_POINT('Ctrl Pts',(-54.3649468106533,-107.328201786851,
174.324310296203));
#23110=CARTESIAN_POINT('Ctrl Pts',(-55.5230181719417,-107.110462414228,
173.149682517375));
#23111=CARTESIAN_POINT('Ctrl Pts',(-56.6810895332303,-106.892723041605,
171.975054738546));
#23112=CARTESIAN_POINT('Ctrl Pts',(-58.3229661698874,-106.623406794376,
171.975054808055));
#23113=CARTESIAN_POINT('Ctrl Pts',(-59.9648428065445,-106.354090547146,
171.975054877564));
#23114=CARTESIAN_POINT('Ctrl Pts',(-61.1229140700869,-106.136351184943,
173.149682754692));
#23115=CARTESIAN_POINT('Ctrl Pts',(-62.2809853336293,-105.918611822741,
174.32431063182));
#23116=CARTESIAN_POINT('Ctrl Pts',(-62.2710472015954,-105.825390065454,
175.985485236888));
#23117=CARTESIAN_POINT('Ctrl Pts',(-62.2611090695615,-105.732168308167,
177.646659841956));
#23118=CARTESIAN_POINT('Ctrl Pts',(-61.0831615824389,-105.763464151479,
178.821287620784));
#23119=CARTESIAN_POINT('Ctrl Pts',(-59.9052140953164,-105.794759994792,
179.995915399612));
#23120=CARTESIAN_POINT('Ctrl Pts',(-58.2434613328252,-105.87763271271,179.995915330104));
#23121=CARTESIAN_POINT('Ctrl Pts',(-56.5817085703341,-105.960505430629,
179.995915260595));
#23122=CARTESIAN_POINT('Ctrl Pts',(-55.4037611809577,-105.991801263521,
178.821287383467));
#23123=CARTESIAN_POINT('Ctrl Pts',(-54.2258137915812,-106.023097096413,
177.646659506339));
#23124=CARTESIAN_POINT('Ctrl Pts',(-54.2158757977811,-105.929875324389,
175.985484901271));
#23125=CARTESIAN_POINT('Ctrl Pts',(-54.205937803981,-105.836653552366,174.324310296203));
#23126=CARTESIAN_POINT('Ctrl Pts',(-55.3640091652695,-105.618914179742,
173.149682517375));
#23127=CARTESIAN_POINT('Ctrl Pts',(-56.522080526558,-105.401174807119,171.975054738546));
#23128=CARTESIAN_POINT('Ctrl Pts',(-58.1639571632151,-105.13185855989,171.975054808055));
#23129=CARTESIAN_POINT('Ctrl Pts',(-59.8058337998722,-104.862542312661,
171.975054877564));
#23130=CARTESIAN_POINT('Ctrl Pts',(-60.9639050634147,-104.644802950458,
173.149682754692));
#23131=CARTESIAN_POINT('Ctrl Pts',(-62.1219763269571,-104.427063588255,
174.32431063182));
#23132=CARTESIAN_POINT('Ctrl Pts',(-62.1120381949232,-104.333841830968,
175.985485236888));
#23133=CARTESIAN_POINT('Ctrl Pts',(-62.1021000628892,-104.240620073681,
177.646659841956));
#23134=CARTESIAN_POINT('Ctrl Pts',(-60.9241525757667,-104.271915916993,
178.821287620784));
#23135=CARTESIAN_POINT('Ctrl Pts',(-59.7462050886442,-104.303211760306,
179.995915399612));
#23136=CARTESIAN_POINT('Ctrl Pts',(-58.084452326153,-104.386084478225,179.995915330104));
#23137=CARTESIAN_POINT('Ctrl Pts',(-56.4226995636619,-104.468957196143,
179.995915260595));
#23138=CARTESIAN_POINT('Ctrl Pts',(-55.2447521742854,-104.500253029035,
178.821287383467));
#23139=CARTESIAN_POINT('Ctrl Pts',(-54.066804784909,-104.531548861927,177.646659506339));
#23140=CARTESIAN_POINT('Ctrl Pts',(-54.0568667911089,-104.438327089904,
175.985484901271));
#23141=CARTESIAN_POINT('Ctrl Pts',(-54.0469287973088,-104.34510531788,174.324310296203));
#23142=CARTESIAN_POINT('Ctrl Pts',(-55.2050001585973,-104.127365945257,
173.149682517375));
#23143=CARTESIAN_POINT('Ctrl Pts',(-56.3630715198858,-103.909626572634,
171.975054738546));
#23144=CARTESIAN_POINT('Ctrl Pts',(-58.0049481565429,-103.640310325404,
171.975054808055));
#23145=CARTESIAN_POINT('Ctrl Pts',(-59.6468247932,-103.370994078175,171.975054877564));
#23146=CARTESIAN_POINT('Ctrl Pts',(-60.8048960567424,-103.153254715972,
173.149682754692));
#23147=CARTESIAN_POINT('Ctrl Pts',(-61.9629673202849,-102.93551535377,174.32431063182));
#23148=CARTESIAN_POINT('Ctrl Pts',(-61.9530291882509,-102.842293596483,
175.985485236888));
#23149=CARTESIAN_POINT('Ctrl Pts',(-61.943091056217,-102.749071839196,177.646659841956));
#23150=CARTESIAN_POINT('Ctrl Pts',(-60.7651435690945,-102.780367682508,
178.821287620784));
#23151=CARTESIAN_POINT('Ctrl Pts',(-59.587196081972,-102.81166352582,179.995915399612));
#23152=CARTESIAN_POINT('Ctrl Pts',(-57.9254433194808,-102.894536243739,
179.995915330104));
#23153=CARTESIAN_POINT('Ctrl Pts',(-56.2636905569897,-102.977408961658,
179.995915260595));
#23154=CARTESIAN_POINT('Ctrl Pts',(-55.0857431676132,-103.00870479455,178.821287383467));
#23155=CARTESIAN_POINT('Ctrl Pts',(-53.9077957782368,-103.040000627442,
177.646659506339));
#23156=CARTESIAN_POINT('Ctrl Pts',(-53.8978577844367,-102.946778855418,
175.985484901271));
#23157=CARTESIAN_POINT('Ctrl Pts',(-53.8879197906366,-102.853557083394,
174.324310296203));
#23158=CARTESIAN_POINT('Ctrl Pts',(-55.0459911519251,-102.635817710771,
173.149682517375));
#23159=CARTESIAN_POINT('Ctrl Pts',(-56.2040625132136,-102.418078338148,
171.975054738546));
#23160=CARTESIAN_POINT('Ctrl Pts',(-57.8459391498707,-102.148762090919,
171.975054808055));
#23161=CARTESIAN_POINT('Ctrl Pts',(-59.4878157865278,-101.879445843689,
171.975054877564));
#23162=CARTESIAN_POINT('Ctrl Pts',(-60.6458870500702,-101.661706481487,
173.149682754692));
#23163=CARTESIAN_POINT('Ctrl Pts',(-61.8039583136126,-101.443967119284,
174.32431063182));
#23164=CARTESIAN_POINT('Ctrl Pts',(-61.7940201815787,-101.350745361997,
175.985485236888));
#23165=CARTESIAN_POINT('Ctrl Pts',(-61.7840820495448,-101.25752360471,177.646659841956));
#23166=CARTESIAN_POINT('Ctrl Pts',(-60.6061345624222,-101.288819448022,
178.821287620784));
#23167=CARTESIAN_POINT('Ctrl Pts',(-59.4281870752997,-101.320115291335,
179.995915399612));
#23168=CARTESIAN_POINT('Ctrl Pts',(-57.7664343128086,-101.402988009253,
179.995915330104));
#23169=CARTESIAN_POINT('Ctrl Pts',(-56.1046815503175,-101.485860727172,
179.995915260595));
#23170=CARTESIAN_POINT('Ctrl Pts',(-54.926734160941,-101.517156560064,178.821287383467));
#23171=CARTESIAN_POINT('Ctrl Pts',(-53.7487867715645,-101.548452392956,
177.646659506339));
#23172=CARTESIAN_POINT('Ctrl Pts',(-53.7388487777644,-101.455230620932,
175.985484901271));
#23173=CARTESIAN_POINT('Ctrl Pts',(-53.7289107839643,-101.362008848909,
174.324310296203));
#23174=CARTESIAN_POINT('Ctrl Pts',(-54.8869821452528,-101.144269476286,
173.149682517375));
#23175=CARTESIAN_POINT('Ctrl Pts',(-56.0450535065414,-100.926530103662,
171.975054738546));
#23176=CARTESIAN_POINT('Ctrl Pts',(-57.6869301431984,-100.657213856433,
171.975054808055));
#23177=CARTESIAN_POINT('Ctrl Pts',(-59.3288067798556,-100.387897609204,
171.975054877564));
#23178=CARTESIAN_POINT('Ctrl Pts',(-60.486878043398,-100.170158247001,173.149682754692));
#23179=CARTESIAN_POINT('Ctrl Pts',(-61.6449493069404,-99.9524188847983,
174.32431063182));
#23180=CARTESIAN_POINT('Ctrl Pts',(-61.6350111749065,-99.8591971275113,
175.985485236888));
#23181=CARTESIAN_POINT('Ctrl Pts',(-61.6250730428726,-99.7659753702243,
177.646659841956));
#23182=CARTESIAN_POINT('Ctrl Pts',(-60.44712555575,-99.7972712135367,178.821287620784));
#23183=CARTESIAN_POINT('Ctrl Pts',(-59.2691780686275,-99.8285670568492,
179.995915399612));
#23184=CARTESIAN_POINT('Ctrl Pts',(-57.6074253061363,-99.9114397747677,
179.995915330104));
#23185=CARTESIAN_POINT('Ctrl Pts',(-55.9456725436452,-99.9943124926864,
179.995915260595));
#23186=CARTESIAN_POINT('Ctrl Pts',(-54.7677251542687,-100.025608325578,
178.821287383467));
#23187=CARTESIAN_POINT('Ctrl Pts',(-53.5897777648923,-100.05690415847,177.646659506339));
#23188=CARTESIAN_POINT('Ctrl Pts',(-53.5798397710922,-99.9636823864468,
175.985484901271));
#23189=CARTESIAN_POINT('Ctrl Pts',(-53.5699017772921,-99.8704606144232,
174.324310296203));
#23190=CARTESIAN_POINT('Ctrl Pts',(-54.7279731385806,-99.6527212418,173.149682517375));
#23191=CARTESIAN_POINT('Ctrl Pts',(-55.8860444998691,-99.4349818691769,
171.975054738546));
#23192=CARTESIAN_POINT('Ctrl Pts',(-57.5279211365262,-99.1656656219475,
171.975054808055));
#23193=CARTESIAN_POINT('Ctrl Pts',(-59.1697977731833,-98.8963493747183,
171.975054877564));
#23194=CARTESIAN_POINT('Ctrl Pts',(-60.3278690367257,-98.6786100125155,
173.149682754692));
#23195=CARTESIAN_POINT('Ctrl Pts',(-61.4859403002682,-98.4608706503128,
174.32431063182));
#23196=CARTESIAN_POINT('Ctrl Pts',(-61.4760021682342,-98.3676488930257,
175.985485236888));
#23197=CARTESIAN_POINT('Ctrl Pts',(-61.4660640362003,-98.2744271357387,
177.646659841956));
#23198=CARTESIAN_POINT('Ctrl Pts',(-60.2881165490778,-98.3057229790511,
178.821287620784));
#23199=CARTESIAN_POINT('Ctrl Pts',(-59.1101690619552,-98.3370188223636,
179.995915399612));
#23200=CARTESIAN_POINT('Ctrl Pts',(-57.4484162994641,-98.4198915402821,
179.995915330104));
#23201=CARTESIAN_POINT('Ctrl Pts',(-55.786663536973,-98.5027642582008,179.995915260595));
#23202=CARTESIAN_POINT('Ctrl Pts',(-54.6087161475965,-98.5340600910929,
178.821287383467));
#23203=CARTESIAN_POINT('Ctrl Pts',(-56.2237961054143,-113.614380048479,
178.813912075476));
#23204=CARTESIAN_POINT('Ctrl Pts',(-55.0488864554725,-113.645352038053,
177.6423391512));
#23205=CARTESIAN_POINT('Ctrl Pts',(-55.0389484614927,-113.552130266048,
175.985484901707));
#23206=CARTESIAN_POINT('Ctrl Pts',(-55.0290104675128,-113.458908494044,
174.328630652215));
#23207=CARTESIAN_POINT('Ctrl Pts',(-56.1840440891124,-113.241492964766,
173.157057825983));
#23208=CARTESIAN_POINT('Ctrl Pts',(-57.3390777107121,-113.024077435489,
171.985484999752));
#23209=CARTESIAN_POINT('Ctrl Pts',(-58.9766583348819,-112.755219171892,
171.985485069079));
#23210=CARTESIAN_POINT('Ctrl Pts',(-60.6142389590518,-112.486360908295,
171.985485138407));
#23211=CARTESIAN_POINT('Ctrl Pts',(-61.7692724831595,-112.268945389411,
173.157058062683));
#23212=CARTESIAN_POINT('Ctrl Pts',(-62.9243060072673,-112.051529870527,
174.328630986959));
#23213=CARTESIAN_POINT('Ctrl Pts',(-62.9143678754131,-111.95830811322,175.985485236451));
#23214=CARTESIAN_POINT('Ctrl Pts',(-62.9044297435589,-111.865086355914,
177.642339485944));
#23215=CARTESIAN_POINT('Ctrl Pts',(-61.7295199961253,-111.896058355881,
178.813912312176));
#23216=CARTESIAN_POINT('Ctrl Pts',(-60.5546102486917,-111.927030355848,
179.985485138407));
#23217=CARTESIAN_POINT('Ctrl Pts',(-58.8971534986878,-112.009445090134,
179.985485069079));
#23218=CARTESIAN_POINT('Ctrl Pts',(-57.2396967486839,-112.09185982442,179.985484999752));
#23219=CARTESIAN_POINT('Ctrl Pts',(-56.0647870987421,-112.122831813994,
178.813912075476));
#23220=CARTESIAN_POINT('Ctrl Pts',(-54.8898774488003,-112.153803803567,
177.6423391512));
#23221=CARTESIAN_POINT('Ctrl Pts',(-54.8799394548205,-112.060582031563,
175.985484901707));
#23222=CARTESIAN_POINT('Ctrl Pts',(-54.8700014608406,-111.967360259558,
174.328630652215));
#23223=CARTESIAN_POINT('Ctrl Pts',(-56.0250350824402,-111.749944730281,
173.157057825983));
#23224=CARTESIAN_POINT('Ctrl Pts',(-57.1800687040398,-111.532529201003,
171.985484999752));
#23225=CARTESIAN_POINT('Ctrl Pts',(-58.8176493282097,-111.263670937406,
171.985485069079));
#23226=CARTESIAN_POINT('Ctrl Pts',(-60.4552299523796,-110.994812673809,
171.985485138407));
#23227=CARTESIAN_POINT('Ctrl Pts',(-61.6102634764873,-110.777397154925,
173.157058062683));
#23228=CARTESIAN_POINT('Ctrl Pts',(-62.7652970005951,-110.559981636041,
174.328630986959));
#23229=CARTESIAN_POINT('Ctrl Pts',(-62.7553588687409,-110.466759878735,
175.985485236451));
#23230=CARTESIAN_POINT('Ctrl Pts',(-62.7454207368867,-110.373538121429,
177.642339485944));
#23231=CARTESIAN_POINT('Ctrl Pts',(-61.5705109894531,-110.404510121395,
178.813912312176));
#23232=CARTESIAN_POINT('Ctrl Pts',(-60.3956012420194,-110.435482121362,
179.985485138407));
#23233=CARTESIAN_POINT('Ctrl Pts',(-58.7381444920155,-110.517896855648,
179.985485069079));
#23234=CARTESIAN_POINT('Ctrl Pts',(-57.0806877420116,-110.600311589935,
179.985484999752));
#23235=CARTESIAN_POINT('Ctrl Pts',(-55.9057780920699,-110.631283579508,
178.813912075476));
#23236=CARTESIAN_POINT('Ctrl Pts',(-54.7308684421281,-110.662255569082,
177.6423391512));
#23237=CARTESIAN_POINT('Ctrl Pts',(-54.7209304481482,-110.569033797077,
175.985484901707));
#23238=CARTESIAN_POINT('Ctrl Pts',(-54.7109924541684,-110.475812025073,
174.328630652215));
#23239=CARTESIAN_POINT('Ctrl Pts',(-55.866026075768,-110.258396495795,173.157057825983));
#23240=CARTESIAN_POINT('Ctrl Pts',(-57.0210596973676,-110.040980966518,
171.985484999752));
#23241=CARTESIAN_POINT('Ctrl Pts',(-58.6586403215375,-109.772122702921,
171.985485069079));
#23242=CARTESIAN_POINT('Ctrl Pts',(-60.2962209457073,-109.503264439324,
171.985485138407));
#23243=CARTESIAN_POINT('Ctrl Pts',(-61.4512544698151,-109.28584892044,173.157058062683));
#23244=CARTESIAN_POINT('Ctrl Pts',(-62.6062879939228,-109.068433401555,
174.328630986959));
#23245=CARTESIAN_POINT('Ctrl Pts',(-62.5963498620687,-108.975211644249,
175.985485236451));
#23246=CARTESIAN_POINT('Ctrl Pts',(-62.5864117302145,-108.881989886943,
177.642339485944));
#23247=CARTESIAN_POINT('Ctrl Pts',(-61.4115019827808,-108.91296188691,178.813912312176));
#23248=CARTESIAN_POINT('Ctrl Pts',(-60.2365922353472,-108.943933886877,
179.985485138407));
#23249=CARTESIAN_POINT('Ctrl Pts',(-58.5791354853433,-109.026348621163,
179.985485069079));
#23250=CARTESIAN_POINT('Ctrl Pts',(-56.9216787353394,-109.108763355449,
179.985484999752));
#23251=CARTESIAN_POINT('Ctrl Pts',(-55.7467690853976,-109.139735345023,
178.813912075476));
#23252=CARTESIAN_POINT('Ctrl Pts',(-54.5718594354559,-109.170707334596,
177.6423391512));
#23253=CARTESIAN_POINT('Ctrl Pts',(-54.561921441476,-109.077485562592,175.985484901707));
#23254=CARTESIAN_POINT('Ctrl Pts',(-54.5519834474962,-108.984263790587,
174.328630652215));
#23255=CARTESIAN_POINT('Ctrl Pts',(-55.7070170690958,-108.76684826131,173.157057825983));
#23256=CARTESIAN_POINT('Ctrl Pts',(-56.8620506906954,-108.549432732032,
171.985484999752));
#23257=CARTESIAN_POINT('Ctrl Pts',(-58.4996313148652,-108.280574468435,
171.985485069079));
#23258=CARTESIAN_POINT('Ctrl Pts',(-60.1372119390351,-108.011716204838,
171.985485138407));
#23259=CARTESIAN_POINT('Ctrl Pts',(-61.2922454631428,-107.794300685954,
173.157058062683));
#23260=CARTESIAN_POINT('Ctrl Pts',(-62.4472789872506,-107.57688516707,174.328630986959));
#23261=CARTESIAN_POINT('Ctrl Pts',(-62.4373408553964,-107.483663409764,
175.985485236451));
#23262=CARTESIAN_POINT('Ctrl Pts',(-62.4274027235423,-107.390441652457,
177.642339485944));
#23263=CARTESIAN_POINT('Ctrl Pts',(-61.2524929761086,-107.421413652424,
178.813912312176));
#23264=CARTESIAN_POINT('Ctrl Pts',(-60.077583228675,-107.452385652391,179.985485138407));
#23265=CARTESIAN_POINT('Ctrl Pts',(-58.4201264786711,-107.534800386677,
179.985485069079));
#23266=CARTESIAN_POINT('Ctrl Pts',(-56.7626697286672,-107.617215120964,
179.985484999752));
#23267=CARTESIAN_POINT('Ctrl Pts',(-55.5877600787254,-107.648187110537,
178.813912075476));
#23268=CARTESIAN_POINT('Ctrl Pts',(-54.4128504287836,-107.67915910011,177.6423391512));
#23269=CARTESIAN_POINT('Ctrl Pts',(-54.4029124348038,-107.585937328106,
175.985484901707));
#23270=CARTESIAN_POINT('Ctrl Pts',(-54.3929744408239,-107.492715556102,
174.328630652215));
#23271=CARTESIAN_POINT('Ctrl Pts',(-55.5480080624235,-107.275300026824,
173.157057825983));
#23272=CARTESIAN_POINT('Ctrl Pts',(-56.7030416840231,-107.057884497547,
171.985484999752));
#23273=CARTESIAN_POINT('Ctrl Pts',(-58.340622308193,-106.78902623395,171.985485069079));
#23274=CARTESIAN_POINT('Ctrl Pts',(-59.9782029323629,-106.520167970353,
171.985485138407));
#23275=CARTESIAN_POINT('Ctrl Pts',(-61.1332364564706,-106.302752451468,
173.157058062683));
#23276=CARTESIAN_POINT('Ctrl Pts',(-62.2882699805784,-106.085336932584,
174.328630986959));
#23277=CARTESIAN_POINT('Ctrl Pts',(-62.2783318487242,-105.992115175278,
175.985485236451));
#23278=CARTESIAN_POINT('Ctrl Pts',(-62.26839371687,-105.898893417972,177.642339485944));
#23279=CARTESIAN_POINT('Ctrl Pts',(-61.0934839694364,-105.929865417939,
178.813912312176));
#23280=CARTESIAN_POINT('Ctrl Pts',(-59.9185742220028,-105.960837417905,
179.985485138407));
#23281=CARTESIAN_POINT('Ctrl Pts',(-58.2611174719989,-106.043252152192,
179.985485069079));
#23282=CARTESIAN_POINT('Ctrl Pts',(-56.603660721995,-106.125666886478,179.985484999752));
#23283=CARTESIAN_POINT('Ctrl Pts',(-55.4287510720532,-106.156638876051,
178.813912075476));
#23284=CARTESIAN_POINT('Ctrl Pts',(-54.2538414221114,-106.187610865625,
177.6423391512));
#23285=CARTESIAN_POINT('Ctrl Pts',(-54.2439034281315,-106.09438909362,175.985484901707));
#23286=CARTESIAN_POINT('Ctrl Pts',(-54.2339654341517,-106.001167321616,
174.328630652215));
#23287=CARTESIAN_POINT('Ctrl Pts',(-55.3889990557513,-105.783751792338,
173.157057825983));
#23288=CARTESIAN_POINT('Ctrl Pts',(-56.5440326773509,-105.566336263061,
171.985484999752));
#23289=CARTESIAN_POINT('Ctrl Pts',(-58.1816133015208,-105.297477999464,
171.985485069079));
#23290=CARTESIAN_POINT('Ctrl Pts',(-59.8191939256906,-105.028619735867,
171.985485138407));
#23291=CARTESIAN_POINT('Ctrl Pts',(-60.9742274497984,-104.811204216983,
173.157058062683));
#23292=CARTESIAN_POINT('Ctrl Pts',(-62.1292609739061,-104.593788698099,
174.328630986959));
#23293=CARTESIAN_POINT('Ctrl Pts',(-62.119322842052,-104.500566940792,175.985485236451));
#23294=CARTESIAN_POINT('Ctrl Pts',(-62.1093847101978,-104.407345183486,
177.642339485944));
#23295=CARTESIAN_POINT('Ctrl Pts',(-60.9344749627642,-104.438317183453,
178.813912312176));
#23296=CARTESIAN_POINT('Ctrl Pts',(-59.7595652153305,-104.46928918342,179.985485138407));
#23297=CARTESIAN_POINT('Ctrl Pts',(-58.1021084653266,-104.551703917706,
179.985485069079));
#23298=CARTESIAN_POINT('Ctrl Pts',(-56.4446517153227,-104.634118651992,
179.985484999752));
#23299=CARTESIAN_POINT('Ctrl Pts',(-55.269742065381,-104.665090641566,178.813912075476));
#23300=CARTESIAN_POINT('Ctrl Pts',(-54.0948324154392,-104.696062631139,
177.6423391512));
#23301=CARTESIAN_POINT('Ctrl Pts',(-54.0848944214593,-104.602840859135,
175.985484901707));
#23302=CARTESIAN_POINT('Ctrl Pts',(-54.0749564274795,-104.50961908713,174.328630652215));
#23303=CARTESIAN_POINT('Ctrl Pts',(-55.2299900490791,-104.292203557853,
173.157057825983));
#23304=CARTESIAN_POINT('Ctrl Pts',(-56.3850236706787,-104.074788028575,
171.985484999752));
#23305=CARTESIAN_POINT('Ctrl Pts',(-58.0226042948486,-103.805929764978,
171.985485069079));
#23306=CARTESIAN_POINT('Ctrl Pts',(-59.6601849190184,-103.537071501381,
171.985485138407));
#23307=CARTESIAN_POINT('Ctrl Pts',(-60.8152184431262,-103.319655982497,
173.157058062683));
#23308=CARTESIAN_POINT('Ctrl Pts',(-61.9702519672339,-103.102240463613,
174.328630986959));
#23309=CARTESIAN_POINT('Ctrl Pts',(-61.9603138353797,-103.009018706307,
175.985485236451));
#23310=CARTESIAN_POINT('Ctrl Pts',(-61.9503757035256,-102.915796949001,
177.642339485944));
#23311=CARTESIAN_POINT('Ctrl Pts',(-60.7754659560919,-102.946768948967,
178.813912312176));
#23312=CARTESIAN_POINT('Ctrl Pts',(-59.6005562086583,-102.977740948934,
179.985485138407));
#23313=CARTESIAN_POINT('Ctrl Pts',(-57.9430994586544,-103.06015568322,179.985485069079));
#23314=CARTESIAN_POINT('Ctrl Pts',(-56.2856427086505,-103.142570417507,
179.985484999752));
#23315=CARTESIAN_POINT('Ctrl Pts',(-55.1107330587087,-103.17354240708,178.813912075476));
#23316=CARTESIAN_POINT('Ctrl Pts',(-53.935823408767,-103.204514396654,177.6423391512));
#23317=CARTESIAN_POINT('Ctrl Pts',(-53.9258854147871,-103.111292624649,
175.985484901707));
#23318=CARTESIAN_POINT('Ctrl Pts',(-53.9159474208072,-103.018070852645,
174.328630652215));
#23319=CARTESIAN_POINT('Ctrl Pts',(-55.0709810424069,-102.800655323367,
173.157057825983));
#23320=CARTESIAN_POINT('Ctrl Pts',(-56.2260146640065,-102.58323979409,171.985484999752));
#23321=CARTESIAN_POINT('Ctrl Pts',(-57.8635952881763,-102.314381530493,
171.985485069079));
#23322=CARTESIAN_POINT('Ctrl Pts',(-59.5011759123462,-102.045523266896,
171.985485138407));
#23323=CARTESIAN_POINT('Ctrl Pts',(-60.6562094364539,-101.828107748012,
173.157058062683));
#23324=CARTESIAN_POINT('Ctrl Pts',(-61.8112429605617,-101.610692229127,
174.328630986959));
#23325=CARTESIAN_POINT('Ctrl Pts',(-61.8013048287075,-101.517470471821,
175.985485236451));
#23326=CARTESIAN_POINT('Ctrl Pts',(-61.7913666968533,-101.424248714515,
177.642339485944));
#23327=CARTESIAN_POINT('Ctrl Pts',(-60.6164569494197,-101.455220714482,
178.813912312176));
#23328=CARTESIAN_POINT('Ctrl Pts',(-59.4415472019861,-101.486192714449,
179.985485138407));
#23329=CARTESIAN_POINT('Ctrl Pts',(-57.7840904519822,-101.568607448735,
179.985485069079));
#23330=CARTESIAN_POINT('Ctrl Pts',(-56.1266337019783,-101.651022183021,
179.985484999752));
#23331=CARTESIAN_POINT('Ctrl Pts',(-54.9517240520365,-101.681994172595,
178.813912075476));
#23332=CARTESIAN_POINT('Ctrl Pts',(-53.7768144020947,-101.712966162168,
177.6423391512));
#23333=CARTESIAN_POINT('Ctrl Pts',(-53.7668764081149,-101.619744390164,
175.985484901707));
#23334=CARTESIAN_POINT('Ctrl Pts',(-53.756938414135,-101.526522618159,174.328630652215));
#23335=CARTESIAN_POINT('Ctrl Pts',(-54.9119720357346,-101.309107088882,
173.157057825983));
#23336=CARTESIAN_POINT('Ctrl Pts',(-56.0670056573342,-101.091691559604,
171.985484999752));
#23337=CARTESIAN_POINT('Ctrl Pts',(-57.7045862815041,-100.822833296007,
171.985485069079));
#23338=CARTESIAN_POINT('Ctrl Pts',(-59.342166905674,-100.55397503241,171.985485138407));
#23339=CARTESIAN_POINT('Ctrl Pts',(-60.4972004297817,-100.336559513526,
173.157058062683));
#23340=CARTESIAN_POINT('Ctrl Pts',(-61.6522339538895,-100.119143994642,
174.328630986959));
#23341=CARTESIAN_POINT('Ctrl Pts',(-61.6422958220353,-100.025922237336,
175.985485236451));
#23342=CARTESIAN_POINT('Ctrl Pts',(-61.6323576901811,-99.9327004800294,
177.642339485944));
#23343=CARTESIAN_POINT('Ctrl Pts',(-60.4574479427475,-99.9636724799962,
178.813912312176));
#23344=CARTESIAN_POINT('Ctrl Pts',(-59.2825381953138,-99.994644479963,179.985485138407));
#23345=CARTESIAN_POINT('Ctrl Pts',(-57.6250814453099,-100.077059214249,
179.985485069079));
#23346=CARTESIAN_POINT('Ctrl Pts',(-55.9676246953061,-100.159473948536,
179.985484999752));
#23347=CARTESIAN_POINT('Ctrl Pts',(-54.7927150453643,-100.190445938109,
178.813912075476));
#23348=CARTESIAN_POINT('Ctrl Pts',(-53.6178053954225,-100.221417927683,
177.6423391512));
#23349=CARTESIAN_POINT('Ctrl Pts',(-53.6078674014426,-100.128196155678,
175.985484901707));
#23350=CARTESIAN_POINT('Ctrl Pts',(-53.5979294074628,-100.034974383673,
174.328630652215));
#23351=CARTESIAN_POINT('Ctrl Pts',(-54.7529630290624,-99.817558854396,173.157057825983));
#23352=CARTESIAN_POINT('Ctrl Pts',(-55.907996650662,-99.6001433251185,171.985484999752));
#23353=CARTESIAN_POINT('Ctrl Pts',(-57.5455772748319,-99.3312850615215,
171.985485069079));
#23354=CARTESIAN_POINT('Ctrl Pts',(-59.1831578990017,-99.0624267979246,
171.985485138407));
#23355=CARTESIAN_POINT('Ctrl Pts',(-60.3381914231095,-98.8450112790404,
173.157058062683));
#23356=CARTESIAN_POINT('Ctrl Pts',(-61.4932249472172,-98.6275957601562,
174.328630986959));
#23357=CARTESIAN_POINT('Ctrl Pts',(-61.4832868153631,-98.53437400285,175.985485236451));
#23358=CARTESIAN_POINT('Ctrl Pts',(-61.4733486835089,-98.4411522455438,
177.642339485944));
#23359=CARTESIAN_POINT('Ctrl Pts',(-60.2984389360752,-98.4721242455106,
178.813912312176));
#23360=CARTESIAN_POINT('Ctrl Pts',(-59.1235291886416,-98.5030962454774,
179.985485138407));
#23361=CARTESIAN_POINT('Ctrl Pts',(-57.4660724386377,-98.5855109797636,
179.985485069079));
#23362=CARTESIAN_POINT('Ctrl Pts',(-55.8086156886338,-98.6679257140499,
179.985484999752));
#23363=CARTESIAN_POINT('Ctrl Pts',(-54.633706038692,-98.6988977036234,178.813912075476));
#23364=CARTESIAN_POINT('Ctrl Pts',(-56.8733667677527,-112.709647553905,
178.072094410988));
#23365=CARTESIAN_POINT('Ctrl Pts',(-56.0039967339745,-112.708046979118,
177.207792449865));
#23366=CARTESIAN_POINT('Ctrl Pts',(-55.9940587219143,-112.614825209041,
175.985484945604));
#23367=CARTESIAN_POINT('Ctrl Pts',(-55.9841207098542,-112.521603438964,
174.763177441344));
#23368=CARTESIAN_POINT('Ctrl Pts',(-56.8336146897208,-112.336760476773,
173.89887555255));
#23369=CARTESIAN_POINT('Ctrl Pts',(-57.6831086695875,-112.151917514582,
173.034573663757));
#23370=CARTESIAN_POINT('Ctrl Pts',(-58.8885910066563,-111.929123815193,
173.034573714903));
#23371=CARTESIAN_POINT('Ctrl Pts',(-60.0940733437252,-111.706330115804,
173.034573766048));
#23372=CARTESIAN_POINT('Ctrl Pts',(-60.9435672516694,-111.521487161281,
173.898875727171));
#23373=CARTESIAN_POINT('Ctrl Pts',(-61.7930611596136,-111.336644206758,
174.763177688294));
#23374=CARTESIAN_POINT('Ctrl Pts',(-61.7831230458397,-111.243422447524,
175.985485192554));
#23375=CARTESIAN_POINT('Ctrl Pts',(-61.7731849320658,-111.15020068829,177.207792696815));
#23376=CARTESIAN_POINT('Ctrl Pts',(-60.9038148263651,-111.14860012117,178.072094585608));
#23377=CARTESIAN_POINT('Ctrl Pts',(-60.0344447206644,-111.14699955405,178.936396474401));
#23378=CARTESIAN_POINT('Ctrl Pts',(-58.8090862577616,-111.183349724129,
178.936396423256));
#23379=CARTESIAN_POINT('Ctrl Pts',(-57.5837277948587,-111.219699894207,
178.936396372111));
#23380=CARTESIAN_POINT('Ctrl Pts',(-56.7143577610805,-111.21809931942,178.072094410988));
#23381=CARTESIAN_POINT('Ctrl Pts',(-55.8449877273022,-111.216498744632,
177.207792449865));
#23382=CARTESIAN_POINT('Ctrl Pts',(-55.8350497152421,-111.123276974555,
175.985484945604));
#23383=CARTESIAN_POINT('Ctrl Pts',(-55.8251117031819,-111.030055204478,
174.763177441344));
#23384=CARTESIAN_POINT('Ctrl Pts',(-56.6746056830486,-110.845212242287,
173.89887555255));
#23385=CARTESIAN_POINT('Ctrl Pts',(-57.5240996629153,-110.660369280097,
173.034573663757));
#23386=CARTESIAN_POINT('Ctrl Pts',(-58.7295819999841,-110.437575580708,
173.034573714903));
#23387=CARTESIAN_POINT('Ctrl Pts',(-59.9350643370529,-110.214781881319,
173.034573766048));
#23388=CARTESIAN_POINT('Ctrl Pts',(-60.7845582449971,-110.029938926795,
173.898875727171));
#23389=CARTESIAN_POINT('Ctrl Pts',(-61.6340521529414,-109.845095972272,
174.763177688294));
#23390=CARTESIAN_POINT('Ctrl Pts',(-61.6241140391675,-109.751874213038,
175.985485192554));
#23391=CARTESIAN_POINT('Ctrl Pts',(-61.6141759253936,-109.658652453805,
177.207792696815));
#23392=CARTESIAN_POINT('Ctrl Pts',(-60.7448058196929,-109.657051886685,
178.072094585608));
#23393=CARTESIAN_POINT('Ctrl Pts',(-59.8754357139922,-109.655451319565,
178.936396474401));
#23394=CARTESIAN_POINT('Ctrl Pts',(-58.6500772510893,-109.691801489643,
178.936396423256));
#23395=CARTESIAN_POINT('Ctrl Pts',(-57.4247187881865,-109.728151659721,
178.936396372111));
#23396=CARTESIAN_POINT('Ctrl Pts',(-56.5553487544082,-109.726551084934,
178.072094410988));
#23397=CARTESIAN_POINT('Ctrl Pts',(-55.68597872063,-109.724950510147,177.207792449865));
#23398=CARTESIAN_POINT('Ctrl Pts',(-55.6760407085698,-109.63172874007,175.985484945604));
#23399=CARTESIAN_POINT('Ctrl Pts',(-55.6661026965097,-109.538506969993,
174.763177441344));
#23400=CARTESIAN_POINT('Ctrl Pts',(-56.5155966763764,-109.353664007802,
173.89887555255));
#23401=CARTESIAN_POINT('Ctrl Pts',(-57.365090656243,-109.168821045611,173.034573663757));
#23402=CARTESIAN_POINT('Ctrl Pts',(-58.5705729933119,-108.946027346222,
173.034573714903));
#23403=CARTESIAN_POINT('Ctrl Pts',(-59.7760553303807,-108.723233646833,
173.034573766048));
#23404=CARTESIAN_POINT('Ctrl Pts',(-60.6255492383249,-108.53839069231,173.898875727171));
#23405=CARTESIAN_POINT('Ctrl Pts',(-61.4750431462691,-108.353547737786,
174.763177688294));
#23406=CARTESIAN_POINT('Ctrl Pts',(-61.4651050324952,-108.260325978553,
175.985485192554));
#23407=CARTESIAN_POINT('Ctrl Pts',(-61.4551669187214,-108.167104219319,
177.207792696815));
#23408=CARTESIAN_POINT('Ctrl Pts',(-60.5857968130207,-108.165503652199,
178.072094585608));
#23409=CARTESIAN_POINT('Ctrl Pts',(-59.71642670732,-108.163903085079,178.936396474401));
#23410=CARTESIAN_POINT('Ctrl Pts',(-58.4910682444171,-108.200253255158,
178.936396423256));
#23411=CARTESIAN_POINT('Ctrl Pts',(-57.2657097815143,-108.236603425236,
178.936396372111));
#23412=CARTESIAN_POINT('Ctrl Pts',(-56.396339747736,-108.235002850448,178.072094410988));
#23413=CARTESIAN_POINT('Ctrl Pts',(-55.5269697139578,-108.233402275661,
177.207792449865));
#23414=CARTESIAN_POINT('Ctrl Pts',(-55.5170317018976,-108.140180505584,
175.985484945604));
#23415=CARTESIAN_POINT('Ctrl Pts',(-55.5070936898375,-108.046958735507,
174.763177441344));
#23416=CARTESIAN_POINT('Ctrl Pts',(-56.3565876697041,-107.862115773316,
173.89887555255));
#23417=CARTESIAN_POINT('Ctrl Pts',(-57.2060816495708,-107.677272811126,
173.034573663757));
#23418=CARTESIAN_POINT('Ctrl Pts',(-58.4115639866396,-107.454479111736,
173.034573714903));
#23419=CARTESIAN_POINT('Ctrl Pts',(-59.6170463237085,-107.231685412347,
173.034573766048));
#23420=CARTESIAN_POINT('Ctrl Pts',(-60.4665402316527,-107.046842457824,
173.898875727171));
#23421=CARTESIAN_POINT('Ctrl Pts',(-61.3160341395969,-106.861999503301,
174.763177688294));
#23422=CARTESIAN_POINT('Ctrl Pts',(-61.306096025823,-106.768777744067,175.985485192554));
#23423=CARTESIAN_POINT('Ctrl Pts',(-61.2961579120492,-106.675555984834,
177.207792696815));
#23424=CARTESIAN_POINT('Ctrl Pts',(-60.4267878063484,-106.673955417714,
178.072094585608));
#23425=CARTESIAN_POINT('Ctrl Pts',(-59.5574177006478,-106.672354850594,
178.936396474401));
#23426=CARTESIAN_POINT('Ctrl Pts',(-58.3320592377449,-106.708705020672,
178.936396423256));
#23427=CARTESIAN_POINT('Ctrl Pts',(-57.106700774842,-106.74505519075,178.936396372111));
#23428=CARTESIAN_POINT('Ctrl Pts',(-56.2373307410638,-106.743454615963,
178.072094410988));
#23429=CARTESIAN_POINT('Ctrl Pts',(-55.3679607072856,-106.741854041175,
177.207792449865));
#23430=CARTESIAN_POINT('Ctrl Pts',(-55.3580226952254,-106.648632271098,
175.985484945604));
#23431=CARTESIAN_POINT('Ctrl Pts',(-55.3480846831652,-106.555410501021,
174.763177441344));
#23432=CARTESIAN_POINT('Ctrl Pts',(-56.1975786630319,-106.370567538831,
173.89887555255));
#23433=CARTESIAN_POINT('Ctrl Pts',(-57.0470726428986,-106.18572457664,173.034573663757));
#23434=CARTESIAN_POINT('Ctrl Pts',(-58.2525549799674,-105.962930877251,
173.034573714903));
#23435=CARTESIAN_POINT('Ctrl Pts',(-59.4580373170363,-105.740137177862,
173.034573766048));
#23436=CARTESIAN_POINT('Ctrl Pts',(-60.3075312249805,-105.555294223339,
173.898875727171));
#23437=CARTESIAN_POINT('Ctrl Pts',(-61.1570251329247,-105.370451268815,
174.763177688294));
#23438=CARTESIAN_POINT('Ctrl Pts',(-61.1470870191508,-105.277229509582,
175.985485192554));
#23439=CARTESIAN_POINT('Ctrl Pts',(-61.1371489053769,-105.184007750348,
177.207792696815));
#23440=CARTESIAN_POINT('Ctrl Pts',(-60.2677787996762,-105.182407183228,
178.072094585608));
#23441=CARTESIAN_POINT('Ctrl Pts',(-59.3984086939755,-105.180806616108,
178.936396474401));
#23442=CARTESIAN_POINT('Ctrl Pts',(-58.1730502310727,-105.217156786186,
178.936396423256));
#23443=CARTESIAN_POINT('Ctrl Pts',(-56.9476917681698,-105.253506956265,
178.936396372111));
#23444=CARTESIAN_POINT('Ctrl Pts',(-56.0783217343916,-105.251906381477,
178.072094410988));
#23445=CARTESIAN_POINT('Ctrl Pts',(-55.2089517006133,-105.25030580669,177.207792449865));
#23446=CARTESIAN_POINT('Ctrl Pts',(-55.1990136885532,-105.157084036613,
175.985484945604));
#23447=CARTESIAN_POINT('Ctrl Pts',(-55.189075676493,-105.063862266536,174.763177441344));
#23448=CARTESIAN_POINT('Ctrl Pts',(-56.0385696563597,-104.879019304345,
173.89887555255));
#23449=CARTESIAN_POINT('Ctrl Pts',(-56.8880636362264,-104.694176342154,
173.034573663757));
#23450=CARTESIAN_POINT('Ctrl Pts',(-58.0935459732952,-104.471382642765,
173.034573714903));
#23451=CARTESIAN_POINT('Ctrl Pts',(-59.299028310364,-104.248588943376,173.034573766048));
#23452=CARTESIAN_POINT('Ctrl Pts',(-60.1485222183082,-104.063745988853,
173.898875727171));
#23453=CARTESIAN_POINT('Ctrl Pts',(-60.9980161262524,-103.87890303433,174.763177688294));
#23454=CARTESIAN_POINT('Ctrl Pts',(-60.9880780124786,-103.785681275096,
175.985485192554));
#23455=CARTESIAN_POINT('Ctrl Pts',(-60.9781398987047,-103.692459515862,
177.207792696815));
#23456=CARTESIAN_POINT('Ctrl Pts',(-60.108769793004,-103.690858948742,178.072094585608));
#23457=CARTESIAN_POINT('Ctrl Pts',(-59.2393996873033,-103.689258381622,
178.936396474401));
#23458=CARTESIAN_POINT('Ctrl Pts',(-58.0140412244004,-103.725608551701,
178.936396423256));
#23459=CARTESIAN_POINT('Ctrl Pts',(-56.7886827614976,-103.761958721779,
178.936396372111));
#23460=CARTESIAN_POINT('Ctrl Pts',(-55.9193127277193,-103.760358146992,
178.072094410988));
#23461=CARTESIAN_POINT('Ctrl Pts',(-55.0499426939411,-103.758757572204,
177.207792449865));
#23462=CARTESIAN_POINT('Ctrl Pts',(-55.0400046818809,-103.665535802127,
175.985484945604));
#23463=CARTESIAN_POINT('Ctrl Pts',(-55.0300666698208,-103.57231403205,174.763177441344));
#23464=CARTESIAN_POINT('Ctrl Pts',(-55.8795606496874,-103.387471069859,
173.89887555255));
#23465=CARTESIAN_POINT('Ctrl Pts',(-56.7290546295541,-103.202628107669,
173.034573663757));
#23466=CARTESIAN_POINT('Ctrl Pts',(-57.934536966623,-102.97983440828,173.034573714903));
#23467=CARTESIAN_POINT('Ctrl Pts',(-59.1400193036918,-102.757040708891,
173.034573766048));
#23468=CARTESIAN_POINT('Ctrl Pts',(-59.989513211636,-102.572197754367,173.898875727171));
#23469=CARTESIAN_POINT('Ctrl Pts',(-60.8390071195802,-102.387354799844,
174.763177688294));
#23470=CARTESIAN_POINT('Ctrl Pts',(-60.8290690058063,-102.29413304061,175.985485192554));
#23471=CARTESIAN_POINT('Ctrl Pts',(-60.8191308920325,-102.200911281377,
177.207792696815));
#23472=CARTESIAN_POINT('Ctrl Pts',(-59.9497607863318,-102.199310714257,
178.072094585608));
#23473=CARTESIAN_POINT('Ctrl Pts',(-59.0803906806311,-102.197710147137,
178.936396474401));
#23474=CARTESIAN_POINT('Ctrl Pts',(-57.8550322177282,-102.234060317215,
178.936396423256));
#23475=CARTESIAN_POINT('Ctrl Pts',(-56.6296737548253,-102.270410487293,
178.936396372111));
#23476=CARTESIAN_POINT('Ctrl Pts',(-55.7603037210471,-102.268809912506,
178.072094410988));
#23477=CARTESIAN_POINT('Ctrl Pts',(-54.8909336872689,-102.267209337719,
177.207792449865));
#23478=CARTESIAN_POINT('Ctrl Pts',(-54.8809956752087,-102.173987567642,
175.985484945604));
#23479=CARTESIAN_POINT('Ctrl Pts',(-54.8710576631486,-102.080765797565,
174.763177441344));
#23480=CARTESIAN_POINT('Ctrl Pts',(-55.7205516430152,-101.895922835374,
173.89887555255));
#23481=CARTESIAN_POINT('Ctrl Pts',(-56.5700456228819,-101.711079873183,
173.034573663757));
#23482=CARTESIAN_POINT('Ctrl Pts',(-57.7755279599507,-101.488286173794,
173.034573714903));
#23483=CARTESIAN_POINT('Ctrl Pts',(-58.9810102970196,-101.265492474405,
173.034573766048));
#23484=CARTESIAN_POINT('Ctrl Pts',(-59.8305042049638,-101.080649519882,
173.898875727171));
#23485=CARTESIAN_POINT('Ctrl Pts',(-60.679998112908,-100.895806565358,174.763177688294));
#23486=CARTESIAN_POINT('Ctrl Pts',(-60.6700599991341,-100.802584806125,
175.985485192554));
#23487=CARTESIAN_POINT('Ctrl Pts',(-60.6601218853602,-100.709363046891,
177.207792696815));
#23488=CARTESIAN_POINT('Ctrl Pts',(-59.7907517796595,-100.707762479771,
178.072094585608));
#23489=CARTESIAN_POINT('Ctrl Pts',(-58.9213816739588,-100.706161912651,
178.936396474401));
#23490=CARTESIAN_POINT('Ctrl Pts',(-57.696023211056,-100.742512082729,178.936396423256));
#23491=CARTESIAN_POINT('Ctrl Pts',(-56.4706647481531,-100.778862252808,
178.936396372111));
#23492=CARTESIAN_POINT('Ctrl Pts',(-55.6012947143749,-100.77726167802,178.072094410988));
#23493=CARTESIAN_POINT('Ctrl Pts',(-54.7319246805966,-100.775661103233,
177.207792449865));
#23494=CARTESIAN_POINT('Ctrl Pts',(-54.7219866685365,-100.682439333156,
175.985484945604));
#23495=CARTESIAN_POINT('Ctrl Pts',(-54.7120486564763,-100.589217563079,
174.763177441344));
#23496=CARTESIAN_POINT('Ctrl Pts',(-55.561542636343,-100.404374600888,173.89887555255));
#23497=CARTESIAN_POINT('Ctrl Pts',(-56.4110366162097,-100.219531638698,
173.034573663757));
#23498=CARTESIAN_POINT('Ctrl Pts',(-57.6165189532785,-99.9967379393085,
173.034573714903));
#23499=CARTESIAN_POINT('Ctrl Pts',(-58.8220012903473,-99.7739442399195,
173.034573766048));
#23500=CARTESIAN_POINT('Ctrl Pts',(-59.6714951982915,-99.5891012853962,
173.898875727171));
#23501=CARTESIAN_POINT('Ctrl Pts',(-60.5209891062358,-99.4042583308729,
174.763177688294));
#23502=CARTESIAN_POINT('Ctrl Pts',(-60.5110509924619,-99.3110365716392,
175.985485192554));
#23503=CARTESIAN_POINT('Ctrl Pts',(-60.501112878688,-99.2178148124055,177.207792696815));
#23504=CARTESIAN_POINT('Ctrl Pts',(-59.6317427729873,-99.2162142452855,
178.072094585608));
#23505=CARTESIAN_POINT('Ctrl Pts',(-58.7623726672866,-99.2146136781656,
178.936396474401));
#23506=CARTESIAN_POINT('Ctrl Pts',(-57.5370142043838,-99.2509638482439,
178.936396423256));
#23507=CARTESIAN_POINT('Ctrl Pts',(-56.3116557414809,-99.2873140183222,
178.936396372111));
#23508=CARTESIAN_POINT('Ctrl Pts',(-55.4422857077027,-99.2857134435348,
178.072094410988));
#23509=CARTESIAN_POINT('Ctrl Pts',(-54.5729156739244,-99.2841128687474,
177.207792449865));
#23510=CARTESIAN_POINT('Ctrl Pts',(-54.5629776618643,-99.1908910986704,
175.985484945604));
#23511=CARTESIAN_POINT('Ctrl Pts',(-54.5530396498041,-99.0976693285933,
174.763177441344));
#23512=CARTESIAN_POINT('Ctrl Pts',(-55.4025336296708,-98.9128263664026,
173.89887555255));
#23513=CARTESIAN_POINT('Ctrl Pts',(-56.2520276095374,-98.727983404212,173.034573663757));
#23514=CARTESIAN_POINT('Ctrl Pts',(-57.4575099466063,-98.5051897048229,
173.034573714903));
#23515=CARTESIAN_POINT('Ctrl Pts',(-58.6629922836751,-98.2823960054338,
173.034573766048));
#23516=CARTESIAN_POINT('Ctrl Pts',(-59.5124861916193,-98.0975530509106,
173.898875727171));
#23517=CARTESIAN_POINT('Ctrl Pts',(-60.3619800995635,-97.9127100963873,
174.763177688294));
#23518=CARTESIAN_POINT('Ctrl Pts',(-60.3520419857897,-97.8194883371536,
175.985485192554));
#23519=CARTESIAN_POINT('Ctrl Pts',(-60.3421038720158,-97.7262665779199,
177.207792696815));
#23520=CARTESIAN_POINT('Ctrl Pts',(-59.4727337663151,-97.7246660108,178.072094585608));
#23521=CARTESIAN_POINT('Ctrl Pts',(-58.6033636606144,-97.72306544368,178.936396474401));
#23522=CARTESIAN_POINT('Ctrl Pts',(-57.3780051977115,-97.7594156137583,
178.936396423256));
#23523=CARTESIAN_POINT('Ctrl Pts',(-56.1526467348087,-97.7957657838366,
178.936396372111));
#23524=CARTESIAN_POINT('Ctrl Pts',(-55.2832767010304,-97.7941652090492,
178.072094410988));
#23525=CARTESIAN_POINT('Ctrl Pts',(-56.1707931031902,-113.117197303651,
178.813912075476));
#23526=CARTESIAN_POINT('Ctrl Pts',(-54.9958834532485,-113.148169293224,
177.6423391512));
#23527=CARTESIAN_POINT('Ctrl Pts',(-54.9859454592686,-113.05494752122,175.985484901707));
#23528=CARTESIAN_POINT('Ctrl Pts',(-54.9760074652888,-112.961725749215,
174.328630652215));
#23529=CARTESIAN_POINT('Ctrl Pts',(-56.1310410868884,-112.744310219938,
173.157057825983));
#23530=CARTESIAN_POINT('Ctrl Pts',(-57.286074708488,-112.52689469066,171.985484999752));
#23531=CARTESIAN_POINT('Ctrl Pts',(-58.9236553326579,-112.258036427063,
171.985485069079));
#23532=CARTESIAN_POINT('Ctrl Pts',(-60.5612359568277,-111.989178163466,
171.985485138407));
#23533=CARTESIAN_POINT('Ctrl Pts',(-61.7162694809355,-111.771762644582,
173.157058062683));
#23534=CARTESIAN_POINT('Ctrl Pts',(-62.8713030050432,-111.554347125698,
174.328630986959));
#23535=CARTESIAN_POINT('Ctrl Pts',(-62.861364873189,-111.461125368392,175.985485236451));
#23536=CARTESIAN_POINT('Ctrl Pts',(-62.8514267413349,-111.367903611086,
177.642339485944));
#23537=CARTESIAN_POINT('Ctrl Pts',(-61.6765169939012,-111.398875611052,
178.813912312176));
#23538=CARTESIAN_POINT('Ctrl Pts',(-60.5016072464676,-111.429847611019,
179.985485138407));
#23539=CARTESIAN_POINT('Ctrl Pts',(-58.8441504964637,-111.512262345305,
179.985485069079));
#23540=CARTESIAN_POINT('Ctrl Pts',(-57.1866937464598,-111.594677079592,
179.985484999752));
#23541=CARTESIAN_POINT('Ctrl Pts',(-56.011784096518,-111.625649069165,178.813912075476));
#23542=CARTESIAN_POINT('Ctrl Pts',(-54.8368744465762,-111.656621058739,
177.6423391512));
#23543=CARTESIAN_POINT('Ctrl Pts',(-54.8269364525964,-111.563399286734,
175.985484901707));
#23544=CARTESIAN_POINT('Ctrl Pts',(-54.8169984586165,-111.47017751473,174.328630652215));
#23545=CARTESIAN_POINT('Ctrl Pts',(-55.9720320802161,-111.252761985452,
173.157057825983));
#23546=CARTESIAN_POINT('Ctrl Pts',(-57.1270657018158,-111.035346456175,
171.985484999752));
#23547=CARTESIAN_POINT('Ctrl Pts',(-58.7646463259856,-110.766488192578,
171.985485069079));
#23548=CARTESIAN_POINT('Ctrl Pts',(-60.4022269501555,-110.497629928981,
171.985485138407));
#23549=CARTESIAN_POINT('Ctrl Pts',(-61.5572604742632,-110.280214410097,
173.157058062683));
#23550=CARTESIAN_POINT('Ctrl Pts',(-62.712293998371,-110.062798891212,174.328630986959));
#23551=CARTESIAN_POINT('Ctrl Pts',(-62.7023558665168,-109.969577133906,
175.985485236451));
#23552=CARTESIAN_POINT('Ctrl Pts',(-62.6924177346626,-109.8763553766,177.642339485944));
#23553=CARTESIAN_POINT('Ctrl Pts',(-61.517507987229,-109.907327376567,178.813912312176));
#23554=CARTESIAN_POINT('Ctrl Pts',(-60.3425982397954,-109.938299376534,
179.985485138407));
#23555=CARTESIAN_POINT('Ctrl Pts',(-58.6851414897915,-110.02071411082,179.985485069079));
#23556=CARTESIAN_POINT('Ctrl Pts',(-57.0276847397876,-110.103128845106,
179.985484999752));
#23557=CARTESIAN_POINT('Ctrl Pts',(-55.8527750898458,-110.13410083468,178.813912075476));
#23558=CARTESIAN_POINT('Ctrl Pts',(-54.677865439904,-110.165072824253,177.6423391512));
#23559=CARTESIAN_POINT('Ctrl Pts',(-54.6679274459242,-110.071851052249,
175.985484901707));
#23560=CARTESIAN_POINT('Ctrl Pts',(-54.6579894519443,-109.978629280244,
174.328630652215));
#23561=CARTESIAN_POINT('Ctrl Pts',(-55.8130230735439,-109.761213750967,
173.157057825983));
#23562=CARTESIAN_POINT('Ctrl Pts',(-56.9680566951435,-109.543798221689,
171.985484999752));
#23563=CARTESIAN_POINT('Ctrl Pts',(-58.6056373193134,-109.274939958092,
171.985485069079));
#23564=CARTESIAN_POINT('Ctrl Pts',(-60.2432179434833,-109.006081694495,
171.985485138407));
#23565=CARTESIAN_POINT('Ctrl Pts',(-61.398251467591,-108.788666175611,173.157058062683));
#23566=CARTESIAN_POINT('Ctrl Pts',(-62.5532849916988,-108.571250656727,
174.328630986959));
#23567=CARTESIAN_POINT('Ctrl Pts',(-62.5433468598446,-108.478028899421,
175.985485236451));
#23568=CARTESIAN_POINT('Ctrl Pts',(-62.5334087279904,-108.384807142114,
177.642339485944));
#23569=CARTESIAN_POINT('Ctrl Pts',(-61.3584989805568,-108.415779142081,
178.813912312176));
#23570=CARTESIAN_POINT('Ctrl Pts',(-60.1835892331231,-108.446751142048,
179.985485138407));
#23571=CARTESIAN_POINT('Ctrl Pts',(-58.5261324831192,-108.529165876334,
179.985485069079));
#23572=CARTESIAN_POINT('Ctrl Pts',(-56.8686757331153,-108.611580610621,
179.985484999752));
#23573=CARTESIAN_POINT('Ctrl Pts',(-55.6937660831736,-108.642552600194,
178.813912075476));
#23574=CARTESIAN_POINT('Ctrl Pts',(-54.5188564332318,-108.673524589768,
177.6423391512));
#23575=CARTESIAN_POINT('Ctrl Pts',(-54.5089184392519,-108.580302817763,
175.985484901707));
#23576=CARTESIAN_POINT('Ctrl Pts',(-54.4989804452721,-108.487081045759,
174.328630652215));
#23577=CARTESIAN_POINT('Ctrl Pts',(-55.6540140668717,-108.269665516481,
173.157057825983));
#23578=CARTESIAN_POINT('Ctrl Pts',(-56.8090476884713,-108.052249987204,
171.985484999752));
#23579=CARTESIAN_POINT('Ctrl Pts',(-58.4466283126412,-107.783391723607,
171.985485069079));
#23580=CARTESIAN_POINT('Ctrl Pts',(-60.084208936811,-107.51453346001,171.985485138407));
#23581=CARTESIAN_POINT('Ctrl Pts',(-61.2392424609188,-107.297117941125,
173.157058062683));
#23582=CARTESIAN_POINT('Ctrl Pts',(-62.3942759850265,-107.079702422241,
174.328630986959));
#23583=CARTESIAN_POINT('Ctrl Pts',(-62.3843378531723,-106.986480664935,
175.985485236451));
#23584=CARTESIAN_POINT('Ctrl Pts',(-62.3743997213182,-106.893258907629,
177.642339485944));
#23585=CARTESIAN_POINT('Ctrl Pts',(-61.1994899738845,-106.924230907596,
178.813912312176));
#23586=CARTESIAN_POINT('Ctrl Pts',(-60.0245802264509,-106.955202907562,
179.985485138407));
#23587=CARTESIAN_POINT('Ctrl Pts',(-58.367123476447,-107.037617641849,179.985485069079));
#23588=CARTESIAN_POINT('Ctrl Pts',(-56.7096667264431,-107.120032376135,
179.985484999752));
#23589=CARTESIAN_POINT('Ctrl Pts',(-55.5347570765013,-107.151004365708,
178.813912075476));
#23590=CARTESIAN_POINT('Ctrl Pts',(-54.3598474265596,-107.181976355282,
177.6423391512));
#23591=CARTESIAN_POINT('Ctrl Pts',(-54.3499094325797,-107.088754583277,
175.985484901707));
#23592=CARTESIAN_POINT('Ctrl Pts',(-54.3399714385998,-106.995532811273,
174.328630652215));
#23593=CARTESIAN_POINT('Ctrl Pts',(-55.4950050601995,-106.778117281995,
173.157057825983));
#23594=CARTESIAN_POINT('Ctrl Pts',(-56.6500386817991,-106.560701752718,
171.985484999752));
#23595=CARTESIAN_POINT('Ctrl Pts',(-58.2876193059689,-106.291843489121,
171.985485069079));
#23596=CARTESIAN_POINT('Ctrl Pts',(-59.9251999301388,-106.022985225524,
171.985485138407));
#23597=CARTESIAN_POINT('Ctrl Pts',(-61.0802334542465,-105.80556970664,173.157058062683));
#23598=CARTESIAN_POINT('Ctrl Pts',(-62.2352669783543,-105.588154187756,
174.328630986959));
#23599=CARTESIAN_POINT('Ctrl Pts',(-62.2253288465001,-105.494932430449,
175.985485236451));
#23600=CARTESIAN_POINT('Ctrl Pts',(-62.2153907146459,-105.401710673143,
177.642339485944));
#23601=CARTESIAN_POINT('Ctrl Pts',(-61.0404809672123,-105.43268267311,178.813912312176));
#23602=CARTESIAN_POINT('Ctrl Pts',(-59.8655712197787,-105.463654673077,
179.985485138407));
#23603=CARTESIAN_POINT('Ctrl Pts',(-58.2081144697748,-105.546069407363,
179.985485069079));
#23604=CARTESIAN_POINT('Ctrl Pts',(-56.5506577197709,-105.628484141649,
179.985484999752));
#23605=CARTESIAN_POINT('Ctrl Pts',(-55.3757480698291,-105.659456131223,
178.813912075476));
#23606=CARTESIAN_POINT('Ctrl Pts',(-54.2008384198873,-105.690428120796,
177.6423391512));
#23607=CARTESIAN_POINT('Ctrl Pts',(-54.1909004259075,-105.597206348792,
175.985484901707));
#23608=CARTESIAN_POINT('Ctrl Pts',(-54.1809624319276,-105.503984576787,
174.328630652215));
#23609=CARTESIAN_POINT('Ctrl Pts',(-55.3359960535272,-105.28656904751,173.157057825983));
#23610=CARTESIAN_POINT('Ctrl Pts',(-56.4910296751268,-105.069153518232,
171.985484999752));
#23611=CARTESIAN_POINT('Ctrl Pts',(-58.1286102992967,-104.800295254635,
171.985485069079));
#23612=CARTESIAN_POINT('Ctrl Pts',(-59.7661909234666,-104.531436991038,
171.985485138407));
#23613=CARTESIAN_POINT('Ctrl Pts',(-60.9212244475743,-104.314021472154,
173.157058062683));
#23614=CARTESIAN_POINT('Ctrl Pts',(-62.0762579716821,-104.09660595327,174.328630986959));
#23615=CARTESIAN_POINT('Ctrl Pts',(-62.0663198398279,-104.003384195964,
175.985485236451));
#23616=CARTESIAN_POINT('Ctrl Pts',(-62.0563817079737,-103.910162438658,
177.642339485944));
#23617=CARTESIAN_POINT('Ctrl Pts',(-60.8814719605401,-103.941134438624,
178.813912312176));
#23618=CARTESIAN_POINT('Ctrl Pts',(-59.7065622131064,-103.972106438591,
179.985485138407));
#23619=CARTESIAN_POINT('Ctrl Pts',(-58.0491054631025,-104.054521172878,
179.985485069079));
#23620=CARTESIAN_POINT('Ctrl Pts',(-56.3916487130987,-104.136935907164,
179.985484999752));
#23621=CARTESIAN_POINT('Ctrl Pts',(-55.2167390631569,-104.167907896737,
178.813912075476));
#23622=CARTESIAN_POINT('Ctrl Pts',(-54.0418294132151,-104.198879886311,
177.6423391512));
#23623=CARTESIAN_POINT('Ctrl Pts',(-54.0318914192353,-104.105658114306,
175.985484901707));
#23624=CARTESIAN_POINT('Ctrl Pts',(-54.0219534252554,-104.012436342302,
174.328630652215));
#23625=CARTESIAN_POINT('Ctrl Pts',(-55.176987046855,-103.795020813024,173.157057825983));
#23626=CARTESIAN_POINT('Ctrl Pts',(-56.3320206684546,-103.577605283747,
171.985484999752));
#23627=CARTESIAN_POINT('Ctrl Pts',(-57.9696012926245,-103.30874702015,171.985485069079));
#23628=CARTESIAN_POINT('Ctrl Pts',(-59.6071819167943,-103.039888756553,
171.985485138407));
#23629=CARTESIAN_POINT('Ctrl Pts',(-60.7622154409021,-102.822473237669,
173.157058062683));
#23630=CARTESIAN_POINT('Ctrl Pts',(-61.9172489650099,-102.605057718784,
174.328630986959));
#23631=CARTESIAN_POINT('Ctrl Pts',(-61.9073108331557,-102.511835961478,
175.985485236451));
#23632=CARTESIAN_POINT('Ctrl Pts',(-61.8973727013015,-102.418614204172,
177.642339485944));
#23633=CARTESIAN_POINT('Ctrl Pts',(-60.7224629538678,-102.449586204139,
178.813912312176));
#23634=CARTESIAN_POINT('Ctrl Pts',(-59.5475532064342,-102.480558204106,
179.985485138407));
#23635=CARTESIAN_POINT('Ctrl Pts',(-57.8900964564303,-102.562972938392,
179.985485069079));
#23636=CARTESIAN_POINT('Ctrl Pts',(-56.2326397064264,-102.645387672678,
179.985484999752));
#23637=CARTESIAN_POINT('Ctrl Pts',(-55.0577300564847,-102.676359662252,
178.813912075476));
#23638=CARTESIAN_POINT('Ctrl Pts',(-53.8828204065429,-102.707331651825,
177.6423391512));
#23639=CARTESIAN_POINT('Ctrl Pts',(-53.872882412563,-102.614109879821,175.985484901707));
#23640=CARTESIAN_POINT('Ctrl Pts',(-53.8629444185832,-102.520888107816,
174.328630652215));
#23641=CARTESIAN_POINT('Ctrl Pts',(-55.0179780401828,-102.303472578539,
173.157057825983));
#23642=CARTESIAN_POINT('Ctrl Pts',(-56.1730116617824,-102.086057049261,
171.985484999752));
#23643=CARTESIAN_POINT('Ctrl Pts',(-57.8105922859523,-101.817198785664,
171.985485069079));
#23644=CARTESIAN_POINT('Ctrl Pts',(-59.4481729101221,-101.548340522067,
171.985485138407));
#23645=CARTESIAN_POINT('Ctrl Pts',(-60.6032064342299,-101.330925003183,
173.157058062683));
#23646=CARTESIAN_POINT('Ctrl Pts',(-61.7582399583376,-101.113509484299,
174.328630986959));
#23647=CARTESIAN_POINT('Ctrl Pts',(-61.7483018264834,-101.020287726993,
175.985485236451));
#23648=CARTESIAN_POINT('Ctrl Pts',(-61.7383636946293,-100.927065969686,
177.642339485944));
#23649=CARTESIAN_POINT('Ctrl Pts',(-60.5634539471956,-100.958037969653,
178.813912312176));
#23650=CARTESIAN_POINT('Ctrl Pts',(-59.388544199762,-100.98900996962,179.985485138407));
#23651=CARTESIAN_POINT('Ctrl Pts',(-57.7310874497581,-101.071424703906,
179.985485069079));
#23652=CARTESIAN_POINT('Ctrl Pts',(-56.0736306997542,-101.153839438193,
179.985484999752));
#23653=CARTESIAN_POINT('Ctrl Pts',(-54.8987210498124,-101.184811427766,
178.813912075476));
#23654=CARTESIAN_POINT('Ctrl Pts',(-53.7238113998707,-101.21578341734,177.6423391512));
#23655=CARTESIAN_POINT('Ctrl Pts',(-53.7138734058908,-101.122561645335,
175.985484901707));
#23656=CARTESIAN_POINT('Ctrl Pts',(-53.7039354119109,-101.029339873331,
174.328630652215));
#23657=CARTESIAN_POINT('Ctrl Pts',(-54.8589690335105,-100.811924344053,
173.157057825983));
#23658=CARTESIAN_POINT('Ctrl Pts',(-56.0140026551102,-100.594508814776,
171.985484999752));
#23659=CARTESIAN_POINT('Ctrl Pts',(-57.65158327928,-100.325650551179,171.985485069079));
#23660=CARTESIAN_POINT('Ctrl Pts',(-59.2891639034499,-100.056792287582,
171.985485138407));
#23661=CARTESIAN_POINT('Ctrl Pts',(-60.4441974275576,-99.8393767686974,
173.157058062683));
#23662=CARTESIAN_POINT('Ctrl Pts',(-61.5992309516654,-99.6219612498133,
174.328630986959));
#23663=CARTESIAN_POINT('Ctrl Pts',(-61.5892928198112,-99.528739492507,175.985485236451));
#23664=CARTESIAN_POINT('Ctrl Pts',(-61.579354687957,-99.4355177352008,177.642339485944));
#23665=CARTESIAN_POINT('Ctrl Pts',(-60.4044449405234,-99.4664897351676,
178.813912312176));
#23666=CARTESIAN_POINT('Ctrl Pts',(-59.2295351930898,-99.4974617351344,
179.985485138407));
#23667=CARTESIAN_POINT('Ctrl Pts',(-57.5720784430859,-99.5798764694207,
179.985485069079));
#23668=CARTESIAN_POINT('Ctrl Pts',(-55.914621693082,-99.662291203707,179.985484999752));
#23669=CARTESIAN_POINT('Ctrl Pts',(-54.7397120431402,-99.6932631932805,
178.813912075476));
#23670=CARTESIAN_POINT('Ctrl Pts',(-53.5648023931984,-99.724235182854,177.6423391512));
#23671=CARTESIAN_POINT('Ctrl Pts',(-53.5548643992186,-99.6310134108495,
175.985484901707));
#23672=CARTESIAN_POINT('Ctrl Pts',(-53.5449264052387,-99.5377916388449,
174.328630652215));
#23673=CARTESIAN_POINT('Ctrl Pts',(-54.6999600268383,-99.3203761095675,
173.157057825983));
#23674=CARTESIAN_POINT('Ctrl Pts',(-55.8549936484379,-99.10296058029,171.985484999752));
#23675=CARTESIAN_POINT('Ctrl Pts',(-57.4925742726078,-98.834102316693,171.985485069079));
#23676=CARTESIAN_POINT('Ctrl Pts',(-59.1301548967777,-98.565244053096,171.985485138407));
#23677=CARTESIAN_POINT('Ctrl Pts',(-60.2851884208854,-98.3478285342118,
173.157058062683));
#23678=CARTESIAN_POINT('Ctrl Pts',(-61.4402219449932,-98.1304130153276,
174.328630986959));
#23679=CARTESIAN_POINT('Ctrl Pts',(-61.430283813139,-98.0371912580215,175.985485236451));
#23680=CARTESIAN_POINT('Ctrl Pts',(-61.4203456812848,-97.9439695007152,
177.642339485944));
#23681=CARTESIAN_POINT('Ctrl Pts',(-60.2454359338512,-97.974941500682,178.813912312176));
#23682=CARTESIAN_POINT('Ctrl Pts',(-59.0705261864175,-98.0059135006488,
179.985485138407));
#23683=CARTESIAN_POINT('Ctrl Pts',(-57.4130694364136,-98.0883282349351,
179.985485069079));
#23684=CARTESIAN_POINT('Ctrl Pts',(-55.7556126864097,-98.1707429692214,
179.985484999752));
#23685=CARTESIAN_POINT('Ctrl Pts',(-54.580703036468,-98.2017149587949,178.813912075476));
#23686=CARTESIAN_POINT('Ctrl Pts',(-61.9716326179341,-111.393034424893,
178.485485069079));
#23687=CARTESIAN_POINT('Ctrl Pts',(-61.8330604135774,-111.39474894277,178.657813499464));
#23688=CARTESIAN_POINT('Ctrl Pts',(-61.6765169939012,-111.398875611052,
178.813912312176));
#23689=CARTESIAN_POINT('Ctrl Pts',(-60.5016072464676,-111.429847611019,
179.985485138407));
#23690=CARTESIAN_POINT('Ctrl Pts',(-58.8441504964637,-111.512262345305,
179.985485069079));
#23691=CARTESIAN_POINT('Ctrl Pts',(-57.1866937464598,-111.594677079592,
179.985484999752));
#23692=CARTESIAN_POINT('Ctrl Pts',(-56.011784096518,-111.625649069165,178.813912075476));
#23693=CARTESIAN_POINT('Ctrl Pts',(-54.8368744465762,-111.656621058739,
177.6423391512));
#23694=CARTESIAN_POINT('Ctrl Pts',(-54.8269364525964,-111.563399286734,
175.985484901707));
#23695=CARTESIAN_POINT('Ctrl Pts',(-54.8169984586165,-111.47017751473,174.328630652215));
#23696=CARTESIAN_POINT('Ctrl Pts',(-55.9720320802161,-111.252761985452,
173.157057825983));
#23697=CARTESIAN_POINT('Ctrl Pts',(-57.1270657018158,-111.035346456175,
171.985484999752));
#23698=CARTESIAN_POINT('Ctrl Pts',(-58.7646463259856,-110.766488192578,
171.985485069079));
#23699=CARTESIAN_POINT('Ctrl Pts',(-60.4022269501555,-110.497629928981,
171.985485138407));
#23700=CARTESIAN_POINT('Ctrl Pts',(-61.5572604742632,-110.280214410097,
173.157058062683));
#23701=CARTESIAN_POINT('Ctrl Pts',(-61.7111554952164,-110.251246276154,
173.313156769748));
#23702=CARTESIAN_POINT('Ctrl Pts',(-61.8469746991872,-110.223708846972,
173.485485069079));
#23703=CARTESIAN_POINT('Ctrl Pts',(-56.2237961054143,-113.614380048479,
178.813912075476));
#23704=CARTESIAN_POINT('Ctrl Pts',(-55.0488864554725,-113.645352038053,
177.6423391512));
#23705=CARTESIAN_POINT('Ctrl Pts',(-55.0389484614927,-113.552130266048,
175.985484901707));
#23706=CARTESIAN_POINT('Ctrl Pts',(-55.0290104675128,-113.458908494044,
174.328630652215));
#23707=CARTESIAN_POINT('Ctrl Pts',(-56.1840440891124,-113.241492964766,
173.157057825983));
#23708=CARTESIAN_POINT('Ctrl Pts',(-57.3390777107121,-113.024077435489,
171.985484999752));
#23709=CARTESIAN_POINT('Ctrl Pts',(-58.9766583348819,-112.755219171892,
171.985485069079));
#23710=CARTESIAN_POINT('Ctrl Pts',(-60.6142389590518,-112.486360908295,
171.985485138407));
#23711=CARTESIAN_POINT('Ctrl Pts',(-61.7692724831595,-112.268945389411,
173.157058062683));
#23712=CARTESIAN_POINT('Ctrl Pts',(-62.9243060072673,-112.051529870527,
174.328630986959));
#23713=CARTESIAN_POINT('Ctrl Pts',(-62.9143678754131,-111.95830811322,175.985485236451));
#23714=CARTESIAN_POINT('Ctrl Pts',(-62.9044297435589,-111.865086355914,
177.642339485944));
#23715=CARTESIAN_POINT('Ctrl Pts',(-61.7295199961253,-111.896058355881,
178.813912312176));
#23716=CARTESIAN_POINT('Ctrl Pts',(-60.5546102486917,-111.927030355848,
179.985485138407));
#23717=CARTESIAN_POINT('Ctrl Pts',(-58.8971534986878,-112.009445090134,
179.985485069079));
#23718=CARTESIAN_POINT('Ctrl Pts',(-57.2396967486839,-112.09185982442,179.985484999752));
#23719=CARTESIAN_POINT('Ctrl Pts',(-56.0647870987421,-112.122831813994,
178.813912075476));
#23720=CARTESIAN_POINT('Ctrl Pts',(-54.8898774488003,-112.153803803567,
177.6423391512));
#23721=CARTESIAN_POINT('Ctrl Pts',(-54.8799394548205,-112.060582031563,
175.985484901707));
#23722=CARTESIAN_POINT('Ctrl Pts',(-54.8700014608406,-111.967360259558,
174.328630652215));
#23723=CARTESIAN_POINT('Ctrl Pts',(-56.0250350824402,-111.749944730281,
173.157057825983));
#23724=CARTESIAN_POINT('Ctrl Pts',(-57.1800687040398,-111.532529201003,
171.985484999752));
#23725=CARTESIAN_POINT('Ctrl Pts',(-58.8176493282097,-111.263670937406,
171.985485069079));
#23726=CARTESIAN_POINT('Ctrl Pts',(-60.4552299523796,-110.994812673809,
171.985485138407));
#23727=CARTESIAN_POINT('Ctrl Pts',(-61.6102634764873,-110.777397154925,
173.157058062683));
#23728=CARTESIAN_POINT('Ctrl Pts',(-62.7652970005951,-110.559981636041,
174.328630986959));
#23729=CARTESIAN_POINT('Ctrl Pts',(-62.7553588687409,-110.466759878735,
175.985485236451));
#23730=CARTESIAN_POINT('Ctrl Pts',(-62.7454207368867,-110.373538121429,
177.642339485944));
#23731=CARTESIAN_POINT('Ctrl Pts',(-61.5705109894531,-110.404510121395,
178.813912312176));
#23732=CARTESIAN_POINT('Ctrl Pts',(-60.3956012420194,-110.435482121362,
179.985485138407));
#23733=CARTESIAN_POINT('Ctrl Pts',(-58.7381444920155,-110.517896855648,
179.985485069079));
#23734=CARTESIAN_POINT('Ctrl Pts',(-57.0806877420116,-110.600311589935,
179.985484999752));
#23735=CARTESIAN_POINT('Ctrl Pts',(-55.9057780920699,-110.631283579508,
178.813912075476));
#23736=CARTESIAN_POINT('Ctrl Pts',(-54.7308684421281,-110.662255569082,
177.6423391512));
#23737=CARTESIAN_POINT('Ctrl Pts',(-54.7209304481482,-110.569033797077,
175.985484901707));
#23738=CARTESIAN_POINT('Ctrl Pts',(-54.7109924541684,-110.475812025073,
174.328630652215));
#23739=CARTESIAN_POINT('Ctrl Pts',(-55.866026075768,-110.258396495795,173.157057825983));
#23740=CARTESIAN_POINT('Ctrl Pts',(-57.0210596973676,-110.040980966518,
171.985484999752));
#23741=CARTESIAN_POINT('Ctrl Pts',(-58.6586403215375,-109.772122702921,
171.985485069079));
#23742=CARTESIAN_POINT('Ctrl Pts',(-60.2962209457073,-109.503264439324,
171.985485138407));
#23743=CARTESIAN_POINT('Ctrl Pts',(-61.4512544698151,-109.28584892044,173.157058062683));
#23744=CARTESIAN_POINT('Ctrl Pts',(-62.6062879939228,-109.068433401555,
174.328630986959));
#23745=CARTESIAN_POINT('Ctrl Pts',(-62.5963498620687,-108.975211644249,
175.985485236451));
#23746=CARTESIAN_POINT('Ctrl Pts',(-62.5864117302145,-108.881989886943,
177.642339485944));
#23747=CARTESIAN_POINT('Ctrl Pts',(-61.4115019827808,-108.91296188691,178.813912312176));
#23748=CARTESIAN_POINT('Ctrl Pts',(-60.2365922353472,-108.943933886877,
179.985485138407));
#23749=CARTESIAN_POINT('Ctrl Pts',(-58.5791354853433,-109.026348621163,
179.985485069079));
#23750=CARTESIAN_POINT('Ctrl Pts',(-56.9216787353394,-109.108763355449,
179.985484999752));
#23751=CARTESIAN_POINT('Ctrl Pts',(-55.7467690853976,-109.139735345023,
178.813912075476));
#23752=CARTESIAN_POINT('Ctrl Pts',(-54.5718594354559,-109.170707334596,
177.6423391512));
#23753=CARTESIAN_POINT('Ctrl Pts',(-54.561921441476,-109.077485562592,175.985484901707));
#23754=CARTESIAN_POINT('Ctrl Pts',(-54.5519834474962,-108.984263790587,
174.328630652215));
#23755=CARTESIAN_POINT('Ctrl Pts',(-55.7070170690958,-108.76684826131,173.157057825983));
#23756=CARTESIAN_POINT('Ctrl Pts',(-56.8620506906954,-108.549432732032,
171.985484999752));
#23757=CARTESIAN_POINT('Ctrl Pts',(-58.4996313148652,-108.280574468435,
171.985485069079));
#23758=CARTESIAN_POINT('Ctrl Pts',(-60.1372119390351,-108.011716204838,
171.985485138407));
#23759=CARTESIAN_POINT('Ctrl Pts',(-61.2922454631428,-107.794300685954,
173.157058062683));
#23760=CARTESIAN_POINT('Ctrl Pts',(-62.4472789872506,-107.57688516707,174.328630986959));
#23761=CARTESIAN_POINT('Ctrl Pts',(-62.4373408553964,-107.483663409764,
175.985485236451));
#23762=CARTESIAN_POINT('Ctrl Pts',(-62.4274027235423,-107.390441652457,
177.642339485944));
#23763=CARTESIAN_POINT('Ctrl Pts',(-61.2524929761086,-107.421413652424,
178.813912312176));
#23764=CARTESIAN_POINT('Ctrl Pts',(-60.077583228675,-107.452385652391,179.985485138407));
#23765=CARTESIAN_POINT('Ctrl Pts',(-58.4201264786711,-107.534800386677,
179.985485069079));
#23766=CARTESIAN_POINT('Ctrl Pts',(-56.7626697286672,-107.617215120964,
179.985484999752));
#23767=CARTESIAN_POINT('Ctrl Pts',(-55.5877600787254,-107.648187110537,
178.813912075476));
#23768=CARTESIAN_POINT('Ctrl Pts',(-54.4128504287836,-107.67915910011,177.6423391512));
#23769=CARTESIAN_POINT('Ctrl Pts',(-54.4029124348038,-107.585937328106,
175.985484901707));
#23770=CARTESIAN_POINT('Ctrl Pts',(-54.3929744408239,-107.492715556102,
174.328630652215));
#23771=CARTESIAN_POINT('Ctrl Pts',(-55.5480080624235,-107.275300026824,
173.157057825983));
#23772=CARTESIAN_POINT('Ctrl Pts',(-56.7030416840231,-107.057884497547,
171.985484999752));
#23773=CARTESIAN_POINT('Ctrl Pts',(-58.340622308193,-106.78902623395,171.985485069079));
#23774=CARTESIAN_POINT('Ctrl Pts',(-59.9782029323629,-106.520167970353,
171.985485138407));
#23775=CARTESIAN_POINT('Ctrl Pts',(-61.1332364564706,-106.302752451468,
173.157058062683));
#23776=CARTESIAN_POINT('Ctrl Pts',(-62.2882699805784,-106.085336932584,
174.328630986959));
#23777=CARTESIAN_POINT('Ctrl Pts',(-62.2783318487242,-105.992115175278,
175.985485236451));
#23778=CARTESIAN_POINT('Ctrl Pts',(-62.26839371687,-105.898893417972,177.642339485944));
#23779=CARTESIAN_POINT('Ctrl Pts',(-61.0934839694364,-105.929865417939,
178.813912312176));
#23780=CARTESIAN_POINT('Ctrl Pts',(-59.9185742220028,-105.960837417905,
179.985485138407));
#23781=CARTESIAN_POINT('Ctrl Pts',(-58.2611174719989,-106.043252152192,
179.985485069079));
#23782=CARTESIAN_POINT('Ctrl Pts',(-56.603660721995,-106.125666886478,179.985484999752));
#23783=CARTESIAN_POINT('Ctrl Pts',(-55.4287510720532,-106.156638876051,
178.813912075476));
#23784=CARTESIAN_POINT('Ctrl Pts',(-54.2538414221114,-106.187610865625,
177.6423391512));
#23785=CARTESIAN_POINT('Ctrl Pts',(-54.2439034281315,-106.09438909362,175.985484901707));
#23786=CARTESIAN_POINT('Ctrl Pts',(-54.2339654341517,-106.001167321616,
174.328630652215));
#23787=CARTESIAN_POINT('Ctrl Pts',(-55.3889990557513,-105.783751792338,
173.157057825983));
#23788=CARTESIAN_POINT('Ctrl Pts',(-56.5440326773509,-105.566336263061,
171.985484999752));
#23789=CARTESIAN_POINT('Ctrl Pts',(-58.1816133015208,-105.297477999464,
171.985485069079));
#23790=CARTESIAN_POINT('Ctrl Pts',(-59.8191939256906,-105.028619735867,
171.985485138407));
#23791=CARTESIAN_POINT('Ctrl Pts',(-60.9742274497984,-104.811204216983,
173.157058062683));
#23792=CARTESIAN_POINT('Ctrl Pts',(-62.1292609739061,-104.593788698099,
174.328630986959));
#23793=CARTESIAN_POINT('Ctrl Pts',(-62.119322842052,-104.500566940792,175.985485236451));
#23794=CARTESIAN_POINT('Ctrl Pts',(-62.1093847101978,-104.407345183486,
177.642339485944));
#23795=CARTESIAN_POINT('Ctrl Pts',(-60.9344749627642,-104.438317183453,
178.813912312176));
#23796=CARTESIAN_POINT('Ctrl Pts',(-59.7595652153305,-104.46928918342,179.985485138407));
#23797=CARTESIAN_POINT('Ctrl Pts',(-58.1021084653266,-104.551703917706,
179.985485069079));
#23798=CARTESIAN_POINT('Ctrl Pts',(-56.4446517153227,-104.634118651992,
179.985484999752));
#23799=CARTESIAN_POINT('Ctrl Pts',(-55.269742065381,-104.665090641566,178.813912075476));
#23800=CARTESIAN_POINT('Ctrl Pts',(-54.0948324154392,-104.696062631139,
177.6423391512));
#23801=CARTESIAN_POINT('Ctrl Pts',(-54.0848944214593,-104.602840859135,
175.985484901707));
#23802=CARTESIAN_POINT('Ctrl Pts',(-54.0749564274795,-104.50961908713,174.328630652215));
#23803=CARTESIAN_POINT('Ctrl Pts',(-55.2299900490791,-104.292203557853,
173.157057825983));
#23804=CARTESIAN_POINT('Ctrl Pts',(-56.3850236706787,-104.074788028575,
171.985484999752));
#23805=CARTESIAN_POINT('Ctrl Pts',(-58.0226042948486,-103.805929764978,
171.985485069079));
#23806=CARTESIAN_POINT('Ctrl Pts',(-59.6601849190184,-103.537071501381,
171.985485138407));
#23807=CARTESIAN_POINT('Ctrl Pts',(-60.8152184431262,-103.319655982497,
173.157058062683));
#23808=CARTESIAN_POINT('Ctrl Pts',(-61.9702519672339,-103.102240463613,
174.328630986959));
#23809=CARTESIAN_POINT('Ctrl Pts',(-61.9603138353797,-103.009018706307,
175.985485236451));
#23810=CARTESIAN_POINT('Ctrl Pts',(-61.9503757035256,-102.915796949001,
177.642339485944));
#23811=CARTESIAN_POINT('Ctrl Pts',(-60.7754659560919,-102.946768948967,
178.813912312176));
#23812=CARTESIAN_POINT('Ctrl Pts',(-59.6005562086583,-102.977740948934,
179.985485138407));
#23813=CARTESIAN_POINT('Ctrl Pts',(-57.9430994586544,-103.06015568322,179.985485069079));
#23814=CARTESIAN_POINT('Ctrl Pts',(-56.2856427086505,-103.142570417507,
179.985484999752));
#23815=CARTESIAN_POINT('Ctrl Pts',(-55.1107330587087,-103.17354240708,178.813912075476));
#23816=CARTESIAN_POINT('Ctrl Pts',(-53.935823408767,-103.204514396654,177.6423391512));
#23817=CARTESIAN_POINT('Ctrl Pts',(-53.9258854147871,-103.111292624649,
175.985484901707));
#23818=CARTESIAN_POINT('Ctrl Pts',(-53.9159474208072,-103.018070852645,
174.328630652215));
#23819=CARTESIAN_POINT('Ctrl Pts',(-55.0709810424069,-102.800655323367,
173.157057825983));
#23820=CARTESIAN_POINT('Ctrl Pts',(-56.2260146640065,-102.58323979409,171.985484999752));
#23821=CARTESIAN_POINT('Ctrl Pts',(-57.8635952881763,-102.314381530493,
171.985485069079));
#23822=CARTESIAN_POINT('Ctrl Pts',(-59.5011759123462,-102.045523266896,
171.985485138407));
#23823=CARTESIAN_POINT('Ctrl Pts',(-60.6562094364539,-101.828107748012,
173.157058062683));
#23824=CARTESIAN_POINT('Ctrl Pts',(-61.8112429605617,-101.610692229127,
174.328630986959));
#23825=CARTESIAN_POINT('Ctrl Pts',(-61.8013048287075,-101.517470471821,
175.985485236451));
#23826=CARTESIAN_POINT('Ctrl Pts',(-61.7913666968533,-101.424248714515,
177.642339485944));
#23827=CARTESIAN_POINT('Ctrl Pts',(-60.6164569494197,-101.455220714482,
178.813912312176));
#23828=CARTESIAN_POINT('Ctrl Pts',(-59.4415472019861,-101.486192714449,
179.985485138407));
#23829=CARTESIAN_POINT('Ctrl Pts',(-57.7840904519822,-101.568607448735,
179.985485069079));
#23830=CARTESIAN_POINT('Ctrl Pts',(-56.1266337019783,-101.651022183021,
179.985484999752));
#23831=CARTESIAN_POINT('Ctrl Pts',(-54.9517240520365,-101.681994172595,
178.813912075476));
#23832=CARTESIAN_POINT('Ctrl Pts',(-53.7768144020947,-101.712966162168,
177.6423391512));
#23833=CARTESIAN_POINT('Ctrl Pts',(-53.7668764081149,-101.619744390164,
175.985484901707));
#23834=CARTESIAN_POINT('Ctrl Pts',(-53.756938414135,-101.526522618159,174.328630652215));
#23835=CARTESIAN_POINT('Ctrl Pts',(-54.9119720357346,-101.309107088882,
173.157057825983));
#23836=CARTESIAN_POINT('Ctrl Pts',(-56.0670056573342,-101.091691559604,
171.985484999752));
#23837=CARTESIAN_POINT('Ctrl Pts',(-57.7045862815041,-100.822833296007,
171.985485069079));
#23838=CARTESIAN_POINT('Ctrl Pts',(-59.342166905674,-100.55397503241,171.985485138407));
#23839=CARTESIAN_POINT('Ctrl Pts',(-60.4972004297817,-100.336559513526,
173.157058062683));
#23840=CARTESIAN_POINT('Ctrl Pts',(-61.6522339538895,-100.119143994642,
174.328630986959));
#23841=CARTESIAN_POINT('Ctrl Pts',(-61.6422958220353,-100.025922237336,
175.985485236451));
#23842=CARTESIAN_POINT('Ctrl Pts',(-61.6323576901811,-99.9327004800294,
177.642339485944));
#23843=CARTESIAN_POINT('Ctrl Pts',(-60.4574479427475,-99.9636724799962,
178.813912312176));
#23844=CARTESIAN_POINT('Ctrl Pts',(-59.2825381953138,-99.994644479963,179.985485138407));
#23845=CARTESIAN_POINT('Ctrl Pts',(-57.6250814453099,-100.077059214249,
179.985485069079));
#23846=CARTESIAN_POINT('Ctrl Pts',(-55.9676246953061,-100.159473948536,
179.985484999752));
#23847=CARTESIAN_POINT('Ctrl Pts',(-54.7927150453643,-100.190445938109,
178.813912075476));
#23848=CARTESIAN_POINT('Ctrl Pts',(-53.6178053954225,-100.221417927683,
177.6423391512));
#23849=CARTESIAN_POINT('Ctrl Pts',(-53.6078674014426,-100.128196155678,
175.985484901707));
#23850=CARTESIAN_POINT('Ctrl Pts',(-53.5979294074628,-100.034974383673,
174.328630652215));
#23851=CARTESIAN_POINT('Ctrl Pts',(-54.7529630290624,-99.817558854396,173.157057825983));
#23852=CARTESIAN_POINT('Ctrl Pts',(-55.907996650662,-99.6001433251185,171.985484999752));
#23853=CARTESIAN_POINT('Ctrl Pts',(-57.5455772748319,-99.3312850615215,
171.985485069079));
#23854=CARTESIAN_POINT('Ctrl Pts',(-59.1831578990017,-99.0624267979246,
171.985485138407));
#23855=CARTESIAN_POINT('Ctrl Pts',(-60.3381914231095,-98.8450112790404,
173.157058062683));
#23856=CARTESIAN_POINT('Ctrl Pts',(-61.4932249472172,-98.6275957601562,
174.328630986959));
#23857=CARTESIAN_POINT('Ctrl Pts',(-61.4832868153631,-98.53437400285,175.985485236451));
#23858=CARTESIAN_POINT('Ctrl Pts',(-61.4733486835089,-98.4411522455438,
177.642339485944));
#23859=CARTESIAN_POINT('Ctrl Pts',(-60.2984389360752,-98.4721242455106,
178.813912312176));
#23860=CARTESIAN_POINT('Ctrl Pts',(-59.1235291886416,-98.5030962454774,
179.985485138407));
#23861=CARTESIAN_POINT('Ctrl Pts',(-57.4660724386377,-98.5855109797636,
179.985485069079));
#23862=CARTESIAN_POINT('Ctrl Pts',(-55.8086156886338,-98.6679257140499,
179.985484999752));
#23863=CARTESIAN_POINT('Ctrl Pts',(-54.633706038692,-98.6988977036234,178.813912075476));
#23864=CARTESIAN_POINT('Ctrl Pts',(-56.9964983346804,-113.864655531781,
178.072094410988));
#23865=CARTESIAN_POINT('Ctrl Pts',(-56.1271283009022,-113.863054956993,
177.207792449865));
#23866=CARTESIAN_POINT('Ctrl Pts',(-56.117190288842,-113.769833186916,175.985484945604));
#23867=CARTESIAN_POINT('Ctrl Pts',(-56.1072522767819,-113.676611416839,
174.763177441344));
#23868=CARTESIAN_POINT('Ctrl Pts',(-56.9567462566485,-113.491768454648,
173.89887555255));
#23869=CARTESIAN_POINT('Ctrl Pts',(-57.8062402365152,-113.306925492458,
173.034573663757));
#23870=CARTESIAN_POINT('Ctrl Pts',(-59.011722573584,-113.084131793069,173.034573714903));
#23871=CARTESIAN_POINT('Ctrl Pts',(-60.2172049106529,-112.86133809368,173.034573766048));
#23872=CARTESIAN_POINT('Ctrl Pts',(-61.0666988185971,-112.676495139156,
173.898875727171));
#23873=CARTESIAN_POINT('Ctrl Pts',(-61.9161927265413,-112.491652184633,
174.763177688294));
#23874=CARTESIAN_POINT('Ctrl Pts',(-61.9062546127674,-112.398430425399,
175.985485192554));
#23875=CARTESIAN_POINT('Ctrl Pts',(-61.8963164989935,-112.305208666166,
177.207792696815));
#23876=CARTESIAN_POINT('Ctrl Pts',(-61.0269463932928,-112.303608099046,
178.072094585608));
#23877=CARTESIAN_POINT('Ctrl Pts',(-60.1575762875921,-112.302007531926,
178.936396474401));
#23878=CARTESIAN_POINT('Ctrl Pts',(-58.9322178246893,-112.338357702004,
178.936396423256));
#23879=CARTESIAN_POINT('Ctrl Pts',(-57.7068593617864,-112.374707872082,
178.936396372111));
#23880=CARTESIAN_POINT('Ctrl Pts',(-56.8374893280082,-112.373107297295,
178.072094410988));
#23881=CARTESIAN_POINT('Ctrl Pts',(-55.9681192942299,-112.371506722508,
177.207792449865));
#23882=CARTESIAN_POINT('Ctrl Pts',(-55.9581812821698,-112.278284952431,
175.985484945604));
#23883=CARTESIAN_POINT('Ctrl Pts',(-55.9482432701096,-112.185063182354,
174.763177441344));
#23884=CARTESIAN_POINT('Ctrl Pts',(-56.7977372499763,-112.000220220163,
173.89887555255));
#23885=CARTESIAN_POINT('Ctrl Pts',(-57.647231229843,-111.815377257972,173.034573663757));
#23886=CARTESIAN_POINT('Ctrl Pts',(-58.8527135669118,-111.592583558583,
173.034573714903));
#23887=CARTESIAN_POINT('Ctrl Pts',(-60.0581959039807,-111.369789859194,
173.034573766048));
#23888=CARTESIAN_POINT('Ctrl Pts',(-60.9076898119249,-111.184946904671,
173.898875727171));
#23889=CARTESIAN_POINT('Ctrl Pts',(-61.7571837198691,-111.000103950148,
174.763177688294));
#23890=CARTESIAN_POINT('Ctrl Pts',(-61.7472456060952,-110.906882190914,
175.985485192554));
#23891=CARTESIAN_POINT('Ctrl Pts',(-61.7373074923213,-110.81366043168,177.207792696815));
#23892=CARTESIAN_POINT('Ctrl Pts',(-60.8679373866206,-110.81205986456,178.072094585608));
#23893=CARTESIAN_POINT('Ctrl Pts',(-59.9985672809199,-110.81045929744,178.936396474401));
#23894=CARTESIAN_POINT('Ctrl Pts',(-58.7732088180171,-110.846809467519,
178.936396423256));
#23895=CARTESIAN_POINT('Ctrl Pts',(-57.5478503551142,-110.883159637597,
178.936396372111));
#23896=CARTESIAN_POINT('Ctrl Pts',(-56.6784803213359,-110.881559062809,
178.072094410988));
#23897=CARTESIAN_POINT('Ctrl Pts',(-55.8091102875577,-110.879958488022,
177.207792449865));
#23898=CARTESIAN_POINT('Ctrl Pts',(-55.7991722754976,-110.786736717945,
175.985484945604));
#23899=CARTESIAN_POINT('Ctrl Pts',(-55.7892342634374,-110.693514947868,
174.763177441344));
#23900=CARTESIAN_POINT('Ctrl Pts',(-56.6387282433041,-110.508671985677,
173.89887555255));
#23901=CARTESIAN_POINT('Ctrl Pts',(-57.4882222231708,-110.323829023487,
173.034573663757));
#23902=CARTESIAN_POINT('Ctrl Pts',(-58.6937045602396,-110.101035324098,
173.034573714903));
#23903=CARTESIAN_POINT('Ctrl Pts',(-59.8991868973084,-109.878241624709,
173.034573766048));
#23904=CARTESIAN_POINT('Ctrl Pts',(-60.7486808052526,-109.693398670185,
173.898875727171));
#23905=CARTESIAN_POINT('Ctrl Pts',(-61.5981747131968,-109.508555715662,
174.763177688294));
#23906=CARTESIAN_POINT('Ctrl Pts',(-61.588236599423,-109.415333956428,175.985485192554));
#23907=CARTESIAN_POINT('Ctrl Pts',(-61.5782984856491,-109.322112197195,
177.207792696815));
#23908=CARTESIAN_POINT('Ctrl Pts',(-60.7089283799484,-109.320511630075,
178.072094585608));
#23909=CARTESIAN_POINT('Ctrl Pts',(-59.8395582742477,-109.318911062955,
178.936396474401));
#23910=CARTESIAN_POINT('Ctrl Pts',(-58.6141998113448,-109.355261233033,
178.936396423256));
#23911=CARTESIAN_POINT('Ctrl Pts',(-57.388841348442,-109.391611403111,178.936396372111));
#23912=CARTESIAN_POINT('Ctrl Pts',(-56.5194713146637,-109.390010828324,
178.072094410988));
#23913=CARTESIAN_POINT('Ctrl Pts',(-55.6501012808855,-109.388410253536,
177.207792449865));
#23914=CARTESIAN_POINT('Ctrl Pts',(-55.6401632688253,-109.295188483459,
175.985484945604));
#23915=CARTESIAN_POINT('Ctrl Pts',(-55.6302252567652,-109.201966713382,
174.763177441344));
#23916=CARTESIAN_POINT('Ctrl Pts',(-56.4797192366319,-109.017123751192,
173.89887555255));
#23917=CARTESIAN_POINT('Ctrl Pts',(-57.3292132164985,-108.832280789001,
173.034573663757));
#23918=CARTESIAN_POINT('Ctrl Pts',(-58.5346955535674,-108.609487089612,
173.034573714903));
#23919=CARTESIAN_POINT('Ctrl Pts',(-59.7401778906362,-108.386693390223,
173.034573766048));
#23920=CARTESIAN_POINT('Ctrl Pts',(-60.5896717985804,-108.2018504357,173.898875727171));
#23921=CARTESIAN_POINT('Ctrl Pts',(-61.4391657065246,-108.017007481176,
174.763177688294));
#23922=CARTESIAN_POINT('Ctrl Pts',(-61.4292275927507,-107.923785721943,
175.985485192554));
#23923=CARTESIAN_POINT('Ctrl Pts',(-61.4192894789769,-107.830563962709,
177.207792696815));
#23924=CARTESIAN_POINT('Ctrl Pts',(-60.5499193732762,-107.828963395589,
178.072094585608));
#23925=CARTESIAN_POINT('Ctrl Pts',(-59.6805492675755,-107.827362828469,
178.936396474401));
#23926=CARTESIAN_POINT('Ctrl Pts',(-58.4551908046726,-107.863712998547,
178.936396423256));
#23927=CARTESIAN_POINT('Ctrl Pts',(-57.2298323417698,-107.900063168626,
178.936396372111));
#23928=CARTESIAN_POINT('Ctrl Pts',(-56.3604623079915,-107.898462593838,
178.072094410988));
#23929=CARTESIAN_POINT('Ctrl Pts',(-55.4910922742133,-107.896862019051,
177.207792449865));
#23930=CARTESIAN_POINT('Ctrl Pts',(-55.4811542621531,-107.803640248974,
175.985484945604));
#23931=CARTESIAN_POINT('Ctrl Pts',(-55.471216250093,-107.710418478897,174.763177441344));
#23932=CARTESIAN_POINT('Ctrl Pts',(-56.3207102299596,-107.525575516706,
173.89887555255));
#23933=CARTESIAN_POINT('Ctrl Pts',(-57.1702042098263,-107.340732554515,
173.034573663757));
#23934=CARTESIAN_POINT('Ctrl Pts',(-58.3756865468951,-107.117938855126,
173.034573714903));
#23935=CARTESIAN_POINT('Ctrl Pts',(-59.581168883964,-106.895145155737,173.034573766048));
#23936=CARTESIAN_POINT('Ctrl Pts',(-60.4306627919082,-106.710302201214,
173.898875727171));
#23937=CARTESIAN_POINT('Ctrl Pts',(-61.2801566998524,-106.525459246691,
174.763177688294));
#23938=CARTESIAN_POINT('Ctrl Pts',(-61.2702185860785,-106.432237487457,
175.985485192554));
#23939=CARTESIAN_POINT('Ctrl Pts',(-61.2602804723046,-106.339015728223,
177.207792696815));
#23940=CARTESIAN_POINT('Ctrl Pts',(-60.3909103666039,-106.337415161103,
178.072094585608));
#23941=CARTESIAN_POINT('Ctrl Pts',(-59.5215402609032,-106.335814593983,
178.936396474401));
#23942=CARTESIAN_POINT('Ctrl Pts',(-58.2961817980004,-106.372164764062,
178.936396423256));
#23943=CARTESIAN_POINT('Ctrl Pts',(-57.0708233350975,-106.40851493414,178.936396372111));
#23944=CARTESIAN_POINT('Ctrl Pts',(-56.2014533013193,-106.406914359353,
178.072094410988));
#23945=CARTESIAN_POINT('Ctrl Pts',(-55.332083267541,-106.405313784565,177.207792449865));
#23946=CARTESIAN_POINT('Ctrl Pts',(-55.3221452554809,-106.312092014488,
175.985484945604));
#23947=CARTESIAN_POINT('Ctrl Pts',(-55.3122072434207,-106.218870244411,
174.763177441344));
#23948=CARTESIAN_POINT('Ctrl Pts',(-56.1617012232874,-106.034027282221,
173.89887555255));
#23949=CARTESIAN_POINT('Ctrl Pts',(-57.0111952031541,-105.84918432003,173.034573663757));
#23950=CARTESIAN_POINT('Ctrl Pts',(-58.2166775402229,-105.626390620641,
173.034573714903));
#23951=CARTESIAN_POINT('Ctrl Pts',(-59.4221598772917,-105.403596921252,
173.034573766048));
#23952=CARTESIAN_POINT('Ctrl Pts',(-60.2716537852359,-105.218753966728,
173.898875727171));
#23953=CARTESIAN_POINT('Ctrl Pts',(-61.1211476931802,-105.033911012205,
174.763177688294));
#23954=CARTESIAN_POINT('Ctrl Pts',(-61.1112095794063,-104.940689252971,
175.985485192554));
#23955=CARTESIAN_POINT('Ctrl Pts',(-61.1012714656324,-104.847467493738,
177.207792696815));
#23956=CARTESIAN_POINT('Ctrl Pts',(-60.2319013599317,-104.845866926618,
178.072094585608));
#23957=CARTESIAN_POINT('Ctrl Pts',(-59.362531254231,-104.844266359498,178.936396474401));
#23958=CARTESIAN_POINT('Ctrl Pts',(-58.1371727913281,-104.880616529576,
178.936396423256));
#23959=CARTESIAN_POINT('Ctrl Pts',(-56.9118143284253,-104.916966699654,
178.936396372111));
#23960=CARTESIAN_POINT('Ctrl Pts',(-56.042444294647,-104.915366124867,178.072094410988));
#23961=CARTESIAN_POINT('Ctrl Pts',(-55.1730742608688,-104.91376555008,177.207792449865));
#23962=CARTESIAN_POINT('Ctrl Pts',(-55.1631362488087,-104.820543780003,
175.985484945604));
#23963=CARTESIAN_POINT('Ctrl Pts',(-55.1531982367485,-104.727322009926,
174.763177441344));
#23964=CARTESIAN_POINT('Ctrl Pts',(-56.0026922166152,-104.542479047735,
173.89887555255));
#23965=CARTESIAN_POINT('Ctrl Pts',(-56.8521861964818,-104.357636085544,
173.034573663757));
#23966=CARTESIAN_POINT('Ctrl Pts',(-58.0576685335507,-104.134842386155,
173.034573714903));
#23967=CARTESIAN_POINT('Ctrl Pts',(-59.2631508706195,-103.912048686766,
173.034573766048));
#23968=CARTESIAN_POINT('Ctrl Pts',(-60.1126447785637,-103.727205732243,
173.898875727171));
#23969=CARTESIAN_POINT('Ctrl Pts',(-60.9621386865079,-103.54236277772,174.763177688294));
#23970=CARTESIAN_POINT('Ctrl Pts',(-60.952200572734,-103.449141018486,175.985485192554));
#23971=CARTESIAN_POINT('Ctrl Pts',(-60.9422624589602,-103.355919259252,
177.207792696815));
#23972=CARTESIAN_POINT('Ctrl Pts',(-60.0728923532595,-103.354318692132,
178.072094585608));
#23973=CARTESIAN_POINT('Ctrl Pts',(-59.2035222475588,-103.352718125012,
178.936396474401));
#23974=CARTESIAN_POINT('Ctrl Pts',(-57.9781637846559,-103.389068295091,
178.936396423256));
#23975=CARTESIAN_POINT('Ctrl Pts',(-56.7528053217531,-103.425418465169,
178.936396372111));
#23976=CARTESIAN_POINT('Ctrl Pts',(-55.8834352879748,-103.423817890381,
178.072094410988));
#23977=CARTESIAN_POINT('Ctrl Pts',(-55.0140652541966,-103.422217315594,
177.207792449865));
#23978=CARTESIAN_POINT('Ctrl Pts',(-55.0041272421364,-103.328995545517,
175.985484945604));
#23979=CARTESIAN_POINT('Ctrl Pts',(-54.9941892300763,-103.23577377544,174.763177441344));
#23980=CARTESIAN_POINT('Ctrl Pts',(-55.8436832099429,-103.050930813249,
173.89887555255));
#23981=CARTESIAN_POINT('Ctrl Pts',(-56.6931771898096,-102.866087851059,
173.034573663757));
#23982=CARTESIAN_POINT('Ctrl Pts',(-57.8986595268784,-102.64329415167,173.034573714903));
#23983=CARTESIAN_POINT('Ctrl Pts',(-59.1041418639473,-102.420500452281,
173.034573766048));
#23984=CARTESIAN_POINT('Ctrl Pts',(-59.9536357718915,-102.235657497757,
173.898875727171));
#23985=CARTESIAN_POINT('Ctrl Pts',(-60.8031296798357,-102.050814543234,
174.763177688294));
#23986=CARTESIAN_POINT('Ctrl Pts',(-60.7931915660618,-101.957592784,175.985485192554));
#23987=CARTESIAN_POINT('Ctrl Pts',(-60.783253452288,-101.864371024767,177.207792696815));
#23988=CARTESIAN_POINT('Ctrl Pts',(-59.9138833465873,-101.862770457647,
178.072094585608));
#23989=CARTESIAN_POINT('Ctrl Pts',(-59.0445132408866,-101.861169890527,
178.936396474401));
#23990=CARTESIAN_POINT('Ctrl Pts',(-57.8191547779837,-101.897520060605,
178.936396423256));
#23991=CARTESIAN_POINT('Ctrl Pts',(-56.5937963150808,-101.933870230683,
178.936396372111));
#23992=CARTESIAN_POINT('Ctrl Pts',(-55.7244262813026,-101.932269655896,
178.072094410988));
#23993=CARTESIAN_POINT('Ctrl Pts',(-54.8550562475244,-101.930669081108,
177.207792449865));
#23994=CARTESIAN_POINT('Ctrl Pts',(-54.8451182354642,-101.837447311031,
175.985484945604));
#23995=CARTESIAN_POINT('Ctrl Pts',(-54.8351802234041,-101.744225540954,
174.763177441344));
#23996=CARTESIAN_POINT('Ctrl Pts',(-55.6846742032707,-101.559382578764,
173.89887555255));
#23997=CARTESIAN_POINT('Ctrl Pts',(-56.5341681831374,-101.374539616573,
173.034573663757));
#23998=CARTESIAN_POINT('Ctrl Pts',(-57.7396505202062,-101.151745917184,
173.034573714903));
#23999=CARTESIAN_POINT('Ctrl Pts',(-58.9451328572751,-100.928952217795,
173.034573766048));
#24000=CARTESIAN_POINT('Ctrl Pts',(-59.7946267652193,-100.744109263272,
173.898875727171));
#24001=CARTESIAN_POINT('Ctrl Pts',(-60.6441206731635,-100.559266308748,
174.763177688294));
#24002=CARTESIAN_POINT('Ctrl Pts',(-60.6341825593896,-100.466044549515,
175.985485192554));
#24003=CARTESIAN_POINT('Ctrl Pts',(-60.6242444456157,-100.372822790281,
177.207792696815));
#24004=CARTESIAN_POINT('Ctrl Pts',(-59.754874339915,-100.371222223161,178.072094585608));
#24005=CARTESIAN_POINT('Ctrl Pts',(-58.8855042342143,-100.369621656041,
178.936396474401));
#24006=CARTESIAN_POINT('Ctrl Pts',(-57.6601457713115,-100.405971826119,
178.936396423256));
#24007=CARTESIAN_POINT('Ctrl Pts',(-56.4347873084086,-100.442321996198,
178.936396372111));
#24008=CARTESIAN_POINT('Ctrl Pts',(-55.5654172746304,-100.44072142141,178.072094410988));
#24009=CARTESIAN_POINT('Ctrl Pts',(-54.6960472408521,-100.439120846623,
177.207792449865));
#24010=CARTESIAN_POINT('Ctrl Pts',(-54.686109228792,-100.345899076546,175.985484945604));
#24011=CARTESIAN_POINT('Ctrl Pts',(-54.6761712167318,-100.252677306469,
174.763177441344));
#24012=CARTESIAN_POINT('Ctrl Pts',(-55.5256651965985,-100.067834344278,
173.89887555255));
#24013=CARTESIAN_POINT('Ctrl Pts',(-56.3751591764652,-99.8829913820874,
173.034573663757));
#24014=CARTESIAN_POINT('Ctrl Pts',(-57.580641513534,-99.6601976826983,173.034573714903));
#24015=CARTESIAN_POINT('Ctrl Pts',(-58.7861238506028,-99.4374039833093,
173.034573766048));
#24016=CARTESIAN_POINT('Ctrl Pts',(-59.635617758547,-99.252561028786,173.898875727171));
#24017=CARTESIAN_POINT('Ctrl Pts',(-60.4851116664912,-99.0677180742627,
174.763177688294));
#24018=CARTESIAN_POINT('Ctrl Pts',(-60.4751735527174,-98.9744963150291,
175.985485192554));
#24019=CARTESIAN_POINT('Ctrl Pts',(-60.4652354389435,-98.8812745557954,
177.207792696815));
#24020=CARTESIAN_POINT('Ctrl Pts',(-59.5958653332428,-98.8796739886754,
178.072094585608));
#24021=CARTESIAN_POINT('Ctrl Pts',(-58.7264952275421,-98.8780734215554,
178.936396474401));
#24022=CARTESIAN_POINT('Ctrl Pts',(-57.5011367646392,-98.9144235916337,
178.936396423256));
#24023=CARTESIAN_POINT('Ctrl Pts',(-56.2757783017364,-98.9507737617121,
178.936396372111));
#24024=CARTESIAN_POINT('Ctrl Pts',(-55.4064082679581,-98.9491731869247,
178.072094410988));
#24025=CARTESIAN_POINT('Ctrl Pts',(-60.8888270454861,-111.922827698674,
179.455551290205));
#24026=CARTESIAN_POINT('Ctrl Pts',(-59.9629308875334,-111.956450790096,
179.985485113659));
#24027=CARTESIAN_POINT('Ctrl Pts',(-58.8971534986878,-112.009445090134,
179.985485069079));
#24028=CARTESIAN_POINT('Ctrl Pts',(-57.2396967486839,-112.09185982442,179.985484999752));
#24029=CARTESIAN_POINT('Ctrl Pts',(-56.0647870987421,-112.122831813994,
178.813912075476));
#24030=CARTESIAN_POINT('Ctrl Pts',(-54.8898774488003,-112.153803803567,
177.6423391512));
#24031=CARTESIAN_POINT('Ctrl Pts',(-54.8799394548205,-112.060582031563,
175.985484901707));
#24032=CARTESIAN_POINT('Ctrl Pts',(-54.8700014608406,-111.967360259558,
174.328630652215));
#24033=CARTESIAN_POINT('Ctrl Pts',(-56.0250350824402,-111.749944730281,
173.157057825983));
#24034=CARTESIAN_POINT('Ctrl Pts',(-57.1800687040398,-111.532529201003,
171.985484999752));
#24035=CARTESIAN_POINT('Ctrl Pts',(-58.8176493282097,-111.263670937406,
171.985485069079));
#24036=CARTESIAN_POINT('Ctrl Pts',(-60.4552299523796,-110.994812673809,
171.985485138407));
#24037=CARTESIAN_POINT('Ctrl Pts',(-61.6102634764873,-110.777397154925,
173.157058062683));
#24038=CARTESIAN_POINT('Ctrl Pts',(-61.7641584974405,-110.748429020983,
173.313156769748));
#24039=CARTESIAN_POINT('Ctrl Pts',(-61.8999777014113,-110.7208915918,173.485485069079));
#24040=CARTESIAN_POINT('Ctrl Pts',(-56.1707931031902,-113.117197303651,
178.813912075476));
#24041=CARTESIAN_POINT('Ctrl Pts',(-54.9958834532485,-113.148169293224,
177.6423391512));
#24042=CARTESIAN_POINT('Ctrl Pts',(-54.9859454592686,-113.05494752122,175.985484901707));
#24043=CARTESIAN_POINT('Ctrl Pts',(-54.9760074652888,-112.961725749215,
174.328630652215));
#24044=CARTESIAN_POINT('Ctrl Pts',(-56.1310410868884,-112.744310219938,
173.157057825983));
#24045=CARTESIAN_POINT('Ctrl Pts',(-57.286074708488,-112.52689469066,171.985484999752));
#24046=CARTESIAN_POINT('Ctrl Pts',(-58.9236553326578,-112.258036427063,
171.985485069079));
#24047=CARTESIAN_POINT('Ctrl Pts',(-60.5612359568277,-111.989178163466,
171.985485138407));
#24048=CARTESIAN_POINT('Ctrl Pts',(-61.7162694809355,-111.771762644582,
173.157058062683));
#24049=CARTESIAN_POINT('Ctrl Pts',(-62.8713030050432,-111.554347125698,
174.328630986959));
#24050=CARTESIAN_POINT('Ctrl Pts',(-62.861364873189,-111.461125368392,175.985485236451));
#24051=CARTESIAN_POINT('Ctrl Pts',(-62.8514267413349,-111.367903611086,
177.642339485944));
#24052=CARTESIAN_POINT('Ctrl Pts',(-61.6765169939012,-111.398875611052,
178.813912312176));
#24053=CARTESIAN_POINT('Ctrl Pts',(-60.5016072464676,-111.429847611019,
179.985485138407));
#24054=CARTESIAN_POINT('Ctrl Pts',(-58.8441504964637,-111.512262345305,
179.985485069079));
#24055=CARTESIAN_POINT('Ctrl Pts',(-57.1866937464598,-111.594677079592,
179.985484999752));
#24056=CARTESIAN_POINT('Ctrl Pts',(-56.011784096518,-111.625649069165,178.813912075476));
#24057=CARTESIAN_POINT('Ctrl Pts',(-54.8368744465763,-111.656621058739,
177.6423391512));
#24058=CARTESIAN_POINT('Ctrl Pts',(-54.8269364525964,-111.563399286734,
175.985484901707));
#24059=CARTESIAN_POINT('Ctrl Pts',(-54.8169984586165,-111.47017751473,174.328630652215));
#24060=CARTESIAN_POINT('Ctrl Pts',(-55.9720320802161,-111.252761985452,
173.157057825983));
#24061=CARTESIAN_POINT('Ctrl Pts',(-57.1270657018158,-111.035346456175,
171.985484999752));
#24062=CARTESIAN_POINT('Ctrl Pts',(-58.7646463259856,-110.766488192578,
171.985485069079));
#24063=CARTESIAN_POINT('Ctrl Pts',(-60.4022269501555,-110.497629928981,
171.985485138407));
#24064=CARTESIAN_POINT('Ctrl Pts',(-61.5572604742632,-110.280214410097,
173.157058062683));
#24065=CARTESIAN_POINT('Ctrl Pts',(-62.712293998371,-110.062798891212,174.328630986959));
#24066=CARTESIAN_POINT('Ctrl Pts',(-62.7023558665168,-109.969577133906,
175.985485236451));
#24067=CARTESIAN_POINT('Ctrl Pts',(-62.6924177346626,-109.8763553766,177.642339485944));
#24068=CARTESIAN_POINT('Ctrl Pts',(-61.517507987229,-109.907327376567,178.813912312176));
#24069=CARTESIAN_POINT('Ctrl Pts',(-60.3425982397954,-109.938299376534,
179.985485138407));
#24070=CARTESIAN_POINT('Ctrl Pts',(-58.6851414897915,-110.02071411082,179.985485069079));
#24071=CARTESIAN_POINT('Ctrl Pts',(-57.0276847397876,-110.103128845106,
179.985484999752));
#24072=CARTESIAN_POINT('Ctrl Pts',(-55.8527750898458,-110.13410083468,178.813912075476));
#24073=CARTESIAN_POINT('Ctrl Pts',(-54.677865439904,-110.165072824253,177.6423391512));
#24074=CARTESIAN_POINT('Ctrl Pts',(-54.6679274459242,-110.071851052249,
175.985484901707));
#24075=CARTESIAN_POINT('Ctrl Pts',(-54.6579894519443,-109.978629280244,
174.328630652215));
#24076=CARTESIAN_POINT('Ctrl Pts',(-55.8130230735439,-109.761213750967,
173.157057825983));
#24077=CARTESIAN_POINT('Ctrl Pts',(-56.9680566951435,-109.543798221689,
171.985484999752));
#24078=CARTESIAN_POINT('Ctrl Pts',(-58.6056373193134,-109.274939958092,
171.985485069079));
#24079=CARTESIAN_POINT('Ctrl Pts',(-60.2432179434833,-109.006081694495,
171.985485138407));
#24080=CARTESIAN_POINT('Ctrl Pts',(-61.398251467591,-108.788666175611,173.157058062683));
#24081=CARTESIAN_POINT('Ctrl Pts',(-62.5532849916988,-108.571250656727,
174.328630986959));
#24082=CARTESIAN_POINT('Ctrl Pts',(-62.5433468598446,-108.478028899421,
175.985485236451));
#24083=CARTESIAN_POINT('Ctrl Pts',(-62.5334087279904,-108.384807142114,
177.642339485944));
#24084=CARTESIAN_POINT('Ctrl Pts',(-61.3584989805568,-108.415779142081,
178.813912312176));
#24085=CARTESIAN_POINT('Ctrl Pts',(-60.1835892331231,-108.446751142048,
179.985485138407));
#24086=CARTESIAN_POINT('Ctrl Pts',(-58.5261324831192,-108.529165876334,
179.985485069079));
#24087=CARTESIAN_POINT('Ctrl Pts',(-56.8686757331153,-108.611580610621,
179.985484999752));
#24088=CARTESIAN_POINT('Ctrl Pts',(-55.6937660831736,-108.642552600194,
178.813912075476));
#24089=CARTESIAN_POINT('Ctrl Pts',(-54.5188564332318,-108.673524589768,
177.6423391512));
#24090=CARTESIAN_POINT('Ctrl Pts',(-54.5089184392519,-108.580302817763,
175.985484901707));
#24091=CARTESIAN_POINT('Ctrl Pts',(-54.4989804452721,-108.487081045759,
174.328630652215));
#24092=CARTESIAN_POINT('Ctrl Pts',(-55.6540140668717,-108.269665516481,
173.157057825983));
#24093=CARTESIAN_POINT('Ctrl Pts',(-56.8090476884713,-108.052249987204,
171.985484999752));
#24094=CARTESIAN_POINT('Ctrl Pts',(-58.4466283126412,-107.783391723607,
171.985485069079));
#24095=CARTESIAN_POINT('Ctrl Pts',(-60.084208936811,-107.51453346001,171.985485138407));
#24096=CARTESIAN_POINT('Ctrl Pts',(-61.2392424609188,-107.297117941125,
173.157058062683));
#24097=CARTESIAN_POINT('Ctrl Pts',(-62.3942759850265,-107.079702422241,
174.328630986959));
#24098=CARTESIAN_POINT('Ctrl Pts',(-62.3843378531723,-106.986480664935,
175.985485236451));
#24099=CARTESIAN_POINT('Ctrl Pts',(-62.3743997213182,-106.893258907629,
177.642339485944));
#24100=CARTESIAN_POINT('Ctrl Pts',(-61.1994899738845,-106.924230907596,
178.813912312176));
#24101=CARTESIAN_POINT('Ctrl Pts',(-60.0245802264509,-106.955202907562,
179.985485138407));
#24102=CARTESIAN_POINT('Ctrl Pts',(-58.367123476447,-107.037617641849,179.985485069079));
#24103=CARTESIAN_POINT('Ctrl Pts',(-56.7096667264431,-107.120032376135,
179.985484999752));
#24104=CARTESIAN_POINT('Ctrl Pts',(-55.5347570765013,-107.151004365708,
178.813912075476));
#24105=CARTESIAN_POINT('Ctrl Pts',(-54.3598474265596,-107.181976355282,
177.6423391512));
#24106=CARTESIAN_POINT('Ctrl Pts',(-54.3499094325797,-107.088754583277,
175.985484901707));
#24107=CARTESIAN_POINT('Ctrl Pts',(-54.3399714385998,-106.995532811273,
174.328630652215));
#24108=CARTESIAN_POINT('Ctrl Pts',(-55.4950050601995,-106.778117281995,
173.157057825983));
#24109=CARTESIAN_POINT('Ctrl Pts',(-56.6500386817991,-106.560701752718,
171.985484999752));
#24110=CARTESIAN_POINT('Ctrl Pts',(-58.2876193059689,-106.291843489121,
171.985485069079));
#24111=CARTESIAN_POINT('Ctrl Pts',(-59.9251999301388,-106.022985225524,
171.985485138407));
#24112=CARTESIAN_POINT('Ctrl Pts',(-61.0802334542465,-105.80556970664,173.157058062683));
#24113=CARTESIAN_POINT('Ctrl Pts',(-62.2352669783543,-105.588154187756,
174.328630986959));
#24114=CARTESIAN_POINT('Ctrl Pts',(-62.2253288465001,-105.494932430449,
175.985485236451));
#24115=CARTESIAN_POINT('Ctrl Pts',(-62.2153907146459,-105.401710673143,
177.642339485944));
#24116=CARTESIAN_POINT('Ctrl Pts',(-61.0404809672123,-105.43268267311,178.813912312176));
#24117=CARTESIAN_POINT('Ctrl Pts',(-59.8655712197787,-105.463654673077,
179.985485138407));
#24118=CARTESIAN_POINT('Ctrl Pts',(-58.2081144697748,-105.546069407363,
179.985485069079));
#24119=CARTESIAN_POINT('Ctrl Pts',(-56.5506577197709,-105.628484141649,
179.985484999752));
#24120=CARTESIAN_POINT('Ctrl Pts',(-55.3757480698291,-105.659456131223,
178.813912075476));
#24121=CARTESIAN_POINT('Ctrl Pts',(-54.2008384198873,-105.690428120796,
177.6423391512));
#24122=CARTESIAN_POINT('Ctrl Pts',(-54.1909004259075,-105.597206348792,
175.985484901707));
#24123=CARTESIAN_POINT('Ctrl Pts',(-54.1809624319276,-105.503984576787,
174.328630652215));
#24124=CARTESIAN_POINT('Ctrl Pts',(-55.3359960535272,-105.28656904751,173.157057825983));
#24125=CARTESIAN_POINT('Ctrl Pts',(-56.4910296751268,-105.069153518232,
171.985484999752));
#24126=CARTESIAN_POINT('Ctrl Pts',(-58.1286102992967,-104.800295254635,
171.985485069079));
#24127=CARTESIAN_POINT('Ctrl Pts',(-59.7661909234666,-104.531436991038,
171.985485138407));
#24128=CARTESIAN_POINT('Ctrl Pts',(-60.9212244475743,-104.314021472154,
173.157058062683));
#24129=CARTESIAN_POINT('Ctrl Pts',(-62.0762579716821,-104.09660595327,174.328630986959));
#24130=CARTESIAN_POINT('Ctrl Pts',(-62.0663198398279,-104.003384195964,
175.985485236451));
#24131=CARTESIAN_POINT('Ctrl Pts',(-62.0563817079737,-103.910162438658,
177.642339485944));
#24132=CARTESIAN_POINT('Ctrl Pts',(-60.8814719605401,-103.941134438624,
178.813912312176));
#24133=CARTESIAN_POINT('Ctrl Pts',(-59.7065622131064,-103.972106438591,
179.985485138407));
#24134=CARTESIAN_POINT('Ctrl Pts',(-58.0491054631025,-104.054521172878,
179.985485069079));
#24135=CARTESIAN_POINT('Ctrl Pts',(-56.3916487130987,-104.136935907164,
179.985484999752));
#24136=CARTESIAN_POINT('Ctrl Pts',(-55.2167390631569,-104.167907896737,
178.813912075476));
#24137=CARTESIAN_POINT('Ctrl Pts',(-54.0418294132151,-104.198879886311,
177.6423391512));
#24138=CARTESIAN_POINT('Ctrl Pts',(-54.0318914192353,-104.105658114306,
175.985484901707));
#24139=CARTESIAN_POINT('Ctrl Pts',(-54.0219534252554,-104.012436342302,
174.328630652215));
#24140=CARTESIAN_POINT('Ctrl Pts',(-55.176987046855,-103.795020813024,173.157057825983));
#24141=CARTESIAN_POINT('Ctrl Pts',(-56.3320206684546,-103.577605283747,
171.985484999752));
#24142=CARTESIAN_POINT('Ctrl Pts',(-57.9696012926245,-103.30874702015,171.985485069079));
#24143=CARTESIAN_POINT('Ctrl Pts',(-59.6071819167943,-103.039888756553,
171.985485138407));
#24144=CARTESIAN_POINT('Ctrl Pts',(-60.7622154409021,-102.822473237669,
173.157058062683));
#24145=CARTESIAN_POINT('Ctrl Pts',(-61.9172489650099,-102.605057718784,
174.328630986959));
#24146=CARTESIAN_POINT('Ctrl Pts',(-61.9073108331557,-102.511835961478,
175.985485236451));
#24147=CARTESIAN_POINT('Ctrl Pts',(-61.8973727013015,-102.418614204172,
177.642339485944));
#24148=CARTESIAN_POINT('Ctrl Pts',(-60.7224629538678,-102.449586204139,
178.813912312176));
#24149=CARTESIAN_POINT('Ctrl Pts',(-59.5475532064342,-102.480558204106,
179.985485138407));
#24150=CARTESIAN_POINT('Ctrl Pts',(-57.8900964564303,-102.562972938392,
179.985485069079));
#24151=CARTESIAN_POINT('Ctrl Pts',(-56.2326397064264,-102.645387672678,
179.985484999752));
#24152=CARTESIAN_POINT('Ctrl Pts',(-55.0577300564847,-102.676359662252,
178.813912075476));
#24153=CARTESIAN_POINT('Ctrl Pts',(-53.8828204065429,-102.707331651825,
177.6423391512));
#24154=CARTESIAN_POINT('Ctrl Pts',(-53.872882412563,-102.614109879821,175.985484901707));
#24155=CARTESIAN_POINT('Ctrl Pts',(-53.8629444185832,-102.520888107816,
174.328630652215));
#24156=CARTESIAN_POINT('Ctrl Pts',(-55.0179780401828,-102.303472578539,
173.157057825983));
#24157=CARTESIAN_POINT('Ctrl Pts',(-56.1730116617824,-102.086057049261,
171.985484999752));
#24158=CARTESIAN_POINT('Ctrl Pts',(-57.8105922859523,-101.817198785664,
171.985485069079));
#24159=CARTESIAN_POINT('Ctrl Pts',(-59.4481729101221,-101.548340522067,
171.985485138407));
#24160=CARTESIAN_POINT('Ctrl Pts',(-60.6032064342299,-101.330925003183,
173.157058062683));
#24161=CARTESIAN_POINT('Ctrl Pts',(-61.7582399583376,-101.113509484299,
174.328630986959));
#24162=CARTESIAN_POINT('Ctrl Pts',(-61.7483018264834,-101.020287726993,
175.985485236451));
#24163=CARTESIAN_POINT('Ctrl Pts',(-61.7383636946293,-100.927065969686,
177.642339485944));
#24164=CARTESIAN_POINT('Ctrl Pts',(-60.5634539471956,-100.958037969653,
178.813912312176));
#24165=CARTESIAN_POINT('Ctrl Pts',(-59.388544199762,-100.98900996962,179.985485138407));
#24166=CARTESIAN_POINT('Ctrl Pts',(-57.7310874497581,-101.071424703906,
179.985485069079));
#24167=CARTESIAN_POINT('Ctrl Pts',(-56.0736306997542,-101.153839438193,
179.985484999752));
#24168=CARTESIAN_POINT('Ctrl Pts',(-54.8987210498124,-101.184811427766,
178.813912075476));
#24169=CARTESIAN_POINT('Ctrl Pts',(-53.7238113998707,-101.21578341734,177.6423391512));
#24170=CARTESIAN_POINT('Ctrl Pts',(-53.7138734058908,-101.122561645335,
175.985484901707));
#24171=CARTESIAN_POINT('Ctrl Pts',(-53.7039354119109,-101.029339873331,
174.328630652215));
#24172=CARTESIAN_POINT('Ctrl Pts',(-54.8589690335105,-100.811924344053,
173.157057825983));
#24173=CARTESIAN_POINT('Ctrl Pts',(-56.0140026551102,-100.594508814776,
171.985484999752));
#24174=CARTESIAN_POINT('Ctrl Pts',(-57.65158327928,-100.325650551179,171.985485069079));
#24175=CARTESIAN_POINT('Ctrl Pts',(-59.2891639034499,-100.056792287582,
171.985485138407));
#24176=CARTESIAN_POINT('Ctrl Pts',(-60.4441974275576,-99.8393767686974,
173.157058062683));
#24177=CARTESIAN_POINT('Ctrl Pts',(-61.5992309516654,-99.6219612498133,
174.328630986959));
#24178=CARTESIAN_POINT('Ctrl Pts',(-61.5892928198112,-99.528739492507,175.985485236451));
#24179=CARTESIAN_POINT('Ctrl Pts',(-61.579354687957,-99.4355177352008,177.642339485944));
#24180=CARTESIAN_POINT('Ctrl Pts',(-60.4044449405234,-99.4664897351676,
178.813912312176));
#24181=CARTESIAN_POINT('Ctrl Pts',(-59.2295351930898,-99.4974617351344,
179.985485138407));
#24182=CARTESIAN_POINT('Ctrl Pts',(-57.5720784430859,-99.5798764694207,
179.985485069079));
#24183=CARTESIAN_POINT('Ctrl Pts',(-55.914621693082,-99.662291203707,179.985484999752));
#24184=CARTESIAN_POINT('Ctrl Pts',(-54.7397120431402,-99.6932631932805,
178.813912075476));
#24185=CARTESIAN_POINT('Ctrl Pts',(-53.5648023931984,-99.724235182854,177.6423391512));
#24186=CARTESIAN_POINT('Ctrl Pts',(-53.5548643992186,-99.6310134108495,
175.985484901707));
#24187=CARTESIAN_POINT('Ctrl Pts',(-53.5449264052387,-99.5377916388449,
174.328630652215));
#24188=CARTESIAN_POINT('Ctrl Pts',(-54.6999600268383,-99.3203761095675,
173.157057825983));
#24189=CARTESIAN_POINT('Ctrl Pts',(-55.8549936484379,-99.10296058029,171.985484999752));
#24190=CARTESIAN_POINT('Ctrl Pts',(-57.4925742726078,-98.834102316693,171.985485069079));
#24191=CARTESIAN_POINT('Ctrl Pts',(-59.1301548967777,-98.5652440530961,
171.985485138407));
#24192=CARTESIAN_POINT('Ctrl Pts',(-60.2851884208854,-98.3478285342118,
173.157058062683));
#24193=CARTESIAN_POINT('Ctrl Pts',(-61.4402219449932,-98.1304130153276,
174.328630986959));
#24194=CARTESIAN_POINT('Ctrl Pts',(-61.430283813139,-98.0371912580215,175.985485236451));
#24195=CARTESIAN_POINT('Ctrl Pts',(-61.4203456812848,-97.9439695007152,
177.642339485944));
#24196=CARTESIAN_POINT('Ctrl Pts',(-60.2454359338512,-97.974941500682,178.813912312176));
#24197=CARTESIAN_POINT('Ctrl Pts',(-59.0705261864175,-98.0059135006488,
179.985485138407));
#24198=CARTESIAN_POINT('Ctrl Pts',(-57.4130694364136,-98.0883282349351,
179.985485069079));
#24199=CARTESIAN_POINT('Ctrl Pts',(-55.7556126864097,-98.1707429692214,
179.985484999752));
#24200=CARTESIAN_POINT('Ctrl Pts',(-54.580703036468,-98.2017149587949,178.813912075476));
#24201=CARTESIAN_POINT('Ctrl Pts',(-56.181115489574,-113.283598570176,178.821287383467));
#24202=CARTESIAN_POINT('Ctrl Pts',(-55.0031681001975,-113.314894403068,
177.646659506339));
#24203=CARTESIAN_POINT('Ctrl Pts',(-54.9932301063974,-113.221672631044,
175.985484901271));
#24204=CARTESIAN_POINT('Ctrl Pts',(-54.9832921125973,-113.12845085902,174.324310296203));
#24205=CARTESIAN_POINT('Ctrl Pts',(-56.1413634738858,-112.910711486397,
173.149682517375));
#24206=CARTESIAN_POINT('Ctrl Pts',(-57.2994348351743,-112.692972113774,
171.975054738546));
#24207=CARTESIAN_POINT('Ctrl Pts',(-58.9413114718314,-112.423655866545,
171.975054808055));
#24208=CARTESIAN_POINT('Ctrl Pts',(-60.5831881084886,-112.154339619316,
171.975054877564));
#24209=CARTESIAN_POINT('Ctrl Pts',(-61.741259372031,-111.936600257113,173.149682754692));
#24210=CARTESIAN_POINT('Ctrl Pts',(-62.8993306355734,-111.71886089491,174.32431063182));
#24211=CARTESIAN_POINT('Ctrl Pts',(-62.8893925035395,-111.625639137623,
175.985485236888));
#24212=CARTESIAN_POINT('Ctrl Pts',(-62.8794543715055,-111.532417380336,
177.646659841956));
#24213=CARTESIAN_POINT('Ctrl Pts',(-61.701506884383,-111.563713223648,178.821287620784));
#24214=CARTESIAN_POINT('Ctrl Pts',(-60.5235593972605,-111.595009066961,
179.995915399612));
#24215=CARTESIAN_POINT('Ctrl Pts',(-58.8618066347693,-111.677881784879,
179.995915330104));
#24216=CARTESIAN_POINT('Ctrl Pts',(-57.2000538722782,-111.760754502798,
179.995915260595));
#24217=CARTESIAN_POINT('Ctrl Pts',(-56.0221064829017,-111.79205033569,178.821287383467));
#24218=CARTESIAN_POINT('Ctrl Pts',(-54.8441590935253,-111.823346168582,
177.646659506339));
#24219=CARTESIAN_POINT('Ctrl Pts',(-54.8342210997252,-111.730124396559,
175.985484901271));
#24220=CARTESIAN_POINT('Ctrl Pts',(-54.8242831059251,-111.636902624535,
174.324310296203));
#24221=CARTESIAN_POINT('Ctrl Pts',(-55.9823544672136,-111.419163251912,
173.149682517375));
#24222=CARTESIAN_POINT('Ctrl Pts',(-57.1404258285021,-111.201423879289,
171.975054738546));
#24223=CARTESIAN_POINT('Ctrl Pts',(-58.7823024651592,-110.932107632059,
171.975054808055));
#24224=CARTESIAN_POINT('Ctrl Pts',(-60.4241791018163,-110.66279138483,171.975054877564));
#24225=CARTESIAN_POINT('Ctrl Pts',(-61.5822503653587,-110.445052022627,
173.149682754692));
#24226=CARTESIAN_POINT('Ctrl Pts',(-62.7403216289012,-110.227312660424,
174.32431063182));
#24227=CARTESIAN_POINT('Ctrl Pts',(-62.7303834968672,-110.134090903137,
175.985485236888));
#24228=CARTESIAN_POINT('Ctrl Pts',(-62.7204453648333,-110.04086914585,177.646659841956));
#24229=CARTESIAN_POINT('Ctrl Pts',(-61.5424978777108,-110.072164989163,
178.821287620784));
#24230=CARTESIAN_POINT('Ctrl Pts',(-60.3645503905882,-110.103460832475,
179.995915399612));
#24231=CARTESIAN_POINT('Ctrl Pts',(-58.7027976280971,-110.186333550394,
179.995915330104));
#24232=CARTESIAN_POINT('Ctrl Pts',(-57.041044865606,-110.269206268313,179.995915260595));
#24233=CARTESIAN_POINT('Ctrl Pts',(-55.8630974762295,-110.300502101205,
178.821287383467));
#24234=CARTESIAN_POINT('Ctrl Pts',(-54.6851500868531,-110.331797934097,
177.646659506339));
#24235=CARTESIAN_POINT('Ctrl Pts',(-54.675212093053,-110.238576162073,175.985484901271));
#24236=CARTESIAN_POINT('Ctrl Pts',(-54.6652740992529,-110.145354390049,
174.324310296203));
#24237=CARTESIAN_POINT('Ctrl Pts',(-55.8233454605414,-109.927615017426,
173.149682517375));
#24238=CARTESIAN_POINT('Ctrl Pts',(-56.9814168218299,-109.709875644803,
171.975054738546));
#24239=CARTESIAN_POINT('Ctrl Pts',(-58.623293458487,-109.440559397574,171.975054808055));
#24240=CARTESIAN_POINT('Ctrl Pts',(-60.2651700951441,-109.171243150344,
171.975054877564));
#24241=CARTESIAN_POINT('Ctrl Pts',(-61.4232413586865,-108.953503788142,
173.149682754692));
#24242=CARTESIAN_POINT('Ctrl Pts',(-62.581312622229,-108.735764425939,174.32431063182));
#24243=CARTESIAN_POINT('Ctrl Pts',(-62.571374490195,-108.642542668652,175.985485236888));
#24244=CARTESIAN_POINT('Ctrl Pts',(-62.5614363581611,-108.549320911365,
177.646659841956));
#24245=CARTESIAN_POINT('Ctrl Pts',(-61.3834888710385,-108.580616754677,
178.821287620784));
#24246=CARTESIAN_POINT('Ctrl Pts',(-60.205541383916,-108.61191259799,179.995915399612));
#24247=CARTESIAN_POINT('Ctrl Pts',(-58.5437886214249,-108.694785315908,
179.995915330104));
#24248=CARTESIAN_POINT('Ctrl Pts',(-56.8820358589338,-108.777658033827,
179.995915260595));
#24249=CARTESIAN_POINT('Ctrl Pts',(-55.7040884695573,-108.808953866719,
178.821287383467));
#24250=CARTESIAN_POINT('Ctrl Pts',(-54.5261410801808,-108.840249699611,
177.646659506339));
#24251=CARTESIAN_POINT('Ctrl Pts',(-54.5162030863807,-108.747027927587,
175.985484901271));
#24252=CARTESIAN_POINT('Ctrl Pts',(-54.5062650925806,-108.653806155564,
174.324310296203));
#24253=CARTESIAN_POINT('Ctrl Pts',(-55.6643364538691,-108.436066782941,
173.149682517375));
#24254=CARTESIAN_POINT('Ctrl Pts',(-56.8224078151577,-108.218327410317,
171.975054738546));
#24255=CARTESIAN_POINT('Ctrl Pts',(-58.4642844518147,-107.949011163088,
171.975054808055));
#24256=CARTESIAN_POINT('Ctrl Pts',(-60.1061610884719,-107.679694915859,
171.975054877564));
#24257=CARTESIAN_POINT('Ctrl Pts',(-61.2642323520143,-107.461955553656,
173.149682754692));
#24258=CARTESIAN_POINT('Ctrl Pts',(-62.4223036155567,-107.244216191453,
174.32431063182));
#24259=CARTESIAN_POINT('Ctrl Pts',(-62.4123654835228,-107.150994434166,
175.985485236888));
#24260=CARTESIAN_POINT('Ctrl Pts',(-62.4024273514889,-107.057772676879,
177.646659841956));
#24261=CARTESIAN_POINT('Ctrl Pts',(-61.2244798643663,-107.089068520192,
178.821287620784));
#24262=CARTESIAN_POINT('Ctrl Pts',(-60.0465323772438,-107.120364363504,
179.995915399612));
#24263=CARTESIAN_POINT('Ctrl Pts',(-58.3847796147526,-107.203237081423,
179.995915330104));
#24264=CARTESIAN_POINT('Ctrl Pts',(-56.7230268522615,-107.286109799341,
179.995915260595));
#24265=CARTESIAN_POINT('Ctrl Pts',(-55.5450794628851,-107.317405632233,
178.821287383467));
#24266=CARTESIAN_POINT('Ctrl Pts',(-54.3671320735086,-107.348701465125,
177.646659506339));
#24267=CARTESIAN_POINT('Ctrl Pts',(-54.3571940797085,-107.255479693102,
175.985484901271));
#24268=CARTESIAN_POINT('Ctrl Pts',(-54.3472560859084,-107.162257921078,
174.324310296203));
#24269=CARTESIAN_POINT('Ctrl Pts',(-55.5053274471969,-106.944518548455,
173.149682517375));
#24270=CARTESIAN_POINT('Ctrl Pts',(-56.6633988084854,-106.726779175832,
171.975054738546));
#24271=CARTESIAN_POINT('Ctrl Pts',(-58.3052754451425,-106.457462928602,
171.975054808055));
#24272=CARTESIAN_POINT('Ctrl Pts',(-59.9471520817997,-106.188146681373,
171.975054877564));
#24273=CARTESIAN_POINT('Ctrl Pts',(-61.1052233453421,-105.97040731917,173.149682754692));
#24274=CARTESIAN_POINT('Ctrl Pts',(-62.2632946088845,-105.752667956968,
174.32431063182));
#24275=CARTESIAN_POINT('Ctrl Pts',(-62.2533564768505,-105.659446199681,
175.985485236888));
#24276=CARTESIAN_POINT('Ctrl Pts',(-62.2434183448166,-105.566224442394,
177.646659841956));
#24277=CARTESIAN_POINT('Ctrl Pts',(-61.0654708576941,-105.597520285706,
178.821287620784));
#24278=CARTESIAN_POINT('Ctrl Pts',(-59.8875233705716,-105.628816129018,
179.995915399612));
#24279=CARTESIAN_POINT('Ctrl Pts',(-58.2257706080804,-105.711688846937,
179.995915330104));
#24280=CARTESIAN_POINT('Ctrl Pts',(-56.5640178455893,-105.794561564856,
179.995915260595));
#24281=CARTESIAN_POINT('Ctrl Pts',(-55.3860704562128,-105.825857397748,
178.821287383467));
#24282=CARTESIAN_POINT('Ctrl Pts',(-54.2081230668364,-105.85715323064,177.646659506339));
#24283=CARTESIAN_POINT('Ctrl Pts',(-54.1981850730363,-105.763931458616,
175.985484901271));
#24284=CARTESIAN_POINT('Ctrl Pts',(-54.1882470792362,-105.670709686593,
174.324310296203));
#24285=CARTESIAN_POINT('Ctrl Pts',(-55.3463184405247,-105.452970313969,
173.149682517375));
#24286=CARTESIAN_POINT('Ctrl Pts',(-56.5043898018132,-105.235230941346,
171.975054738546));
#24287=CARTESIAN_POINT('Ctrl Pts',(-58.1462664384703,-104.965914694117,
171.975054808055));
#24288=CARTESIAN_POINT('Ctrl Pts',(-59.7881430751274,-104.696598446888,
171.975054877564));
#24289=CARTESIAN_POINT('Ctrl Pts',(-60.9462143386698,-104.478859084685,
173.149682754692));
#24290=CARTESIAN_POINT('Ctrl Pts',(-62.1042856022123,-104.261119722482,
174.32431063182));
#24291=CARTESIAN_POINT('Ctrl Pts',(-62.0943474701783,-104.167897965195,
175.985485236888));
#24292=CARTESIAN_POINT('Ctrl Pts',(-62.0844093381444,-104.074676207908,
177.646659841956));
#24293=CARTESIAN_POINT('Ctrl Pts',(-60.9064618510219,-104.10597205122,178.821287620784));
#24294=CARTESIAN_POINT('Ctrl Pts',(-59.7285143638993,-104.137267894533,
179.995915399612));
#24295=CARTESIAN_POINT('Ctrl Pts',(-58.0667616014082,-104.220140612451,
179.995915330104));
#24296=CARTESIAN_POINT('Ctrl Pts',(-56.4050088389171,-104.30301333037,179.995915260595));
#24297=CARTESIAN_POINT('Ctrl Pts',(-55.2270614495406,-104.334309163262,
178.821287383467));
#24298=CARTESIAN_POINT('Ctrl Pts',(-54.0491140601642,-104.365604996154,
177.646659506339));
#24299=CARTESIAN_POINT('Ctrl Pts',(-54.039176066364,-104.272383224131,175.985484901271));
#24300=CARTESIAN_POINT('Ctrl Pts',(-54.029238072564,-104.179161452107,174.324310296203));
#24301=CARTESIAN_POINT('Ctrl Pts',(-55.1873094338524,-103.961422079484,
173.149682517375));
#24302=CARTESIAN_POINT('Ctrl Pts',(-56.345380795141,-103.743682706861,171.975054738546));
#24303=CARTESIAN_POINT('Ctrl Pts',(-57.9872574317981,-103.474366459631,
171.975054808055));
#24304=CARTESIAN_POINT('Ctrl Pts',(-59.6291340684552,-103.205050212402,
171.975054877564));
#24305=CARTESIAN_POINT('Ctrl Pts',(-60.7872053319976,-102.987310850199,
173.149682754692));
#24306=CARTESIAN_POINT('Ctrl Pts',(-61.94527659554,-102.769571487996,174.32431063182));
#24307=CARTESIAN_POINT('Ctrl Pts',(-61.9353384635061,-102.676349730709,
175.985485236888));
#24308=CARTESIAN_POINT('Ctrl Pts',(-61.9254003314722,-102.583127973422,
177.646659841956));
#24309=CARTESIAN_POINT('Ctrl Pts',(-60.7474528443496,-102.614423816735,
178.821287620784));
#24310=CARTESIAN_POINT('Ctrl Pts',(-59.5695053572271,-102.645719660047,
179.995915399612));
#24311=CARTESIAN_POINT('Ctrl Pts',(-57.907752594736,-102.728592377966,179.995915330104));
#24312=CARTESIAN_POINT('Ctrl Pts',(-56.2459998322448,-102.811465095885,
179.995915260595));
#24313=CARTESIAN_POINT('Ctrl Pts',(-55.0680524428684,-102.842760928777,
178.821287383467));
#24314=CARTESIAN_POINT('Ctrl Pts',(-53.8901050534919,-102.874056761669,
177.646659506339));
#24315=CARTESIAN_POINT('Ctrl Pts',(-53.8801670596918,-102.780834989645,
175.985484901271));
#24316=CARTESIAN_POINT('Ctrl Pts',(-53.8702290658917,-102.687613217621,
174.324310296203));
#24317=CARTESIAN_POINT('Ctrl Pts',(-55.0283004271802,-102.469873844998,
173.149682517375));
#24318=CARTESIAN_POINT('Ctrl Pts',(-56.1863717884687,-102.252134472375,
171.975054738546));
#24319=CARTESIAN_POINT('Ctrl Pts',(-57.8282484251258,-101.982818225146,
171.975054808055));
#24320=CARTESIAN_POINT('Ctrl Pts',(-59.470125061783,-101.713501977916,171.975054877564));
#24321=CARTESIAN_POINT('Ctrl Pts',(-60.6281963253254,-101.495762615714,
173.149682754692));
#24322=CARTESIAN_POINT('Ctrl Pts',(-61.7862675888678,-101.278023253511,
174.32431063182));
#24323=CARTESIAN_POINT('Ctrl Pts',(-61.7763294568339,-101.184801496224,
175.985485236888));
#24324=CARTESIAN_POINT('Ctrl Pts',(-61.7663913247999,-101.091579738937,
177.646659841956));
#24325=CARTESIAN_POINT('Ctrl Pts',(-60.5884438376774,-101.122875582249,
178.821287620784));
#24326=CARTESIAN_POINT('Ctrl Pts',(-59.4104963505549,-101.154171425562,
179.995915399612));
#24327=CARTESIAN_POINT('Ctrl Pts',(-57.7487435880637,-101.23704414348,179.995915330104));
#24328=CARTESIAN_POINT('Ctrl Pts',(-56.0869908255726,-101.319916861399,
179.995915260595));
#24329=CARTESIAN_POINT('Ctrl Pts',(-54.9090434361961,-101.351212694291,
178.821287383467));
#24330=CARTESIAN_POINT('Ctrl Pts',(-53.7310960468197,-101.382508527183,
177.646659506339));
#24331=CARTESIAN_POINT('Ctrl Pts',(-53.7211580530196,-101.289286755159,
175.985484901271));
#24332=CARTESIAN_POINT('Ctrl Pts',(-53.7112200592195,-101.196064983136,
174.324310296203));
#24333=CARTESIAN_POINT('Ctrl Pts',(-54.869291420508,-100.978325610513,173.149682517375));
#24334=CARTESIAN_POINT('Ctrl Pts',(-56.0273627817965,-100.760586237889,
171.975054738546));
#24335=CARTESIAN_POINT('Ctrl Pts',(-57.6692394184536,-100.49126999066,171.975054808055));
#24336=CARTESIAN_POINT('Ctrl Pts',(-59.3111160551107,-100.221953743431,
171.975054877564));
#24337=CARTESIAN_POINT('Ctrl Pts',(-60.4691873186531,-100.004214381228,
173.149682754692));
#24338=CARTESIAN_POINT('Ctrl Pts',(-61.6272585821956,-99.7864750190253,
174.32431063182));
#24339=CARTESIAN_POINT('Ctrl Pts',(-61.6173204501616,-99.6932532617382,
175.985485236888));
#24340=CARTESIAN_POINT('Ctrl Pts',(-61.6073823181277,-99.6000315044512,
177.646659841956));
#24341=CARTESIAN_POINT('Ctrl Pts',(-60.4294348310052,-99.6313273477637,
178.821287620784));
#24342=CARTESIAN_POINT('Ctrl Pts',(-59.2514873438827,-99.6626231910761,
179.995915399612));
#24343=CARTESIAN_POINT('Ctrl Pts',(-57.5897345813915,-99.7454959089947,
179.995915330104));
#24344=CARTESIAN_POINT('Ctrl Pts',(-55.9279818189004,-99.8283686269133,
179.995915260595));
#24345=CARTESIAN_POINT('Ctrl Pts',(-54.7500344295239,-99.8596644598054,
178.821287383467));
#24346=CARTESIAN_POINT('Ctrl Pts',(-53.5720870401475,-99.8909602926975,
177.646659506339));
#24347=CARTESIAN_POINT('Ctrl Pts',(-53.5621490463474,-99.7977385206737,
175.985484901271));
#24348=CARTESIAN_POINT('Ctrl Pts',(-53.5522110525473,-99.7045167486501,
174.324310296203));
#24349=CARTESIAN_POINT('Ctrl Pts',(-54.7102824138358,-99.4867773760269,
173.149682517375));
#24350=CARTESIAN_POINT('Ctrl Pts',(-55.8683537751243,-99.2690380034038,
171.975054738546));
#24351=CARTESIAN_POINT('Ctrl Pts',(-57.5102304117814,-98.9997217561745,
171.975054808055));
#24352=CARTESIAN_POINT('Ctrl Pts',(-59.1521070484385,-98.7304055089452,
171.975054877564));
#24353=CARTESIAN_POINT('Ctrl Pts',(-60.3101783119809,-98.5126661467424,
173.149682754692));
#24354=CARTESIAN_POINT('Ctrl Pts',(-61.4682495755234,-98.2949267845397,
174.32431063182));
#24355=CARTESIAN_POINT('Ctrl Pts',(-61.4583114434894,-98.2017050272526,
175.985485236888));
#24356=CARTESIAN_POINT('Ctrl Pts',(-61.4483733114555,-98.1084832699656,
177.646659841956));
#24357=CARTESIAN_POINT('Ctrl Pts',(-60.2704258243329,-98.139779113278,178.821287620784));
#24358=CARTESIAN_POINT('Ctrl Pts',(-59.0924783372104,-98.1710749565905,
179.995915399612));
#24359=CARTESIAN_POINT('Ctrl Pts',(-57.4307255747193,-98.2539476745091,
179.995915330104));
#24360=CARTESIAN_POINT('Ctrl Pts',(-55.7689728122282,-98.3368203924277,
179.995915260595));
#24361=CARTESIAN_POINT('Ctrl Pts',(-54.5910254228517,-98.3681162253198,
178.821287383467));
#24362=CARTESIAN_POINT('Ctrl Pts',(-56.1988062143188,-113.449542435949,
178.821287383467));
#24363=CARTESIAN_POINT('Ctrl Pts',(-55.0208588249424,-113.480838268841,
177.646659506339));
#24364=CARTESIAN_POINT('Ctrl Pts',(-55.0109208311422,-113.387616496817,
175.985484901271));
#24365=CARTESIAN_POINT('Ctrl Pts',(-55.0009828373422,-113.294394724794,
174.324310296203));
#24366=CARTESIAN_POINT('Ctrl Pts',(-56.1590541986307,-113.07665535217,173.149682517375));
#24367=CARTESIAN_POINT('Ctrl Pts',(-57.3171255599192,-112.858915979547,
171.975054738546));
#24368=CARTESIAN_POINT('Ctrl Pts',(-58.9590021965763,-112.589599732318,
171.975054808055));
#24369=CARTESIAN_POINT('Ctrl Pts',(-60.6008788332334,-112.320283485089,
171.975054877564));
#24370=CARTESIAN_POINT('Ctrl Pts',(-61.7589500967758,-112.102544122886,
173.149682754692));
#24371=CARTESIAN_POINT('Ctrl Pts',(-62.9170213603182,-111.884804760683,
174.32431063182));
#24372=CARTESIAN_POINT('Ctrl Pts',(-62.9070832282843,-111.791583003396,
175.985485236888));
#24373=CARTESIAN_POINT('Ctrl Pts',(-62.8971450962504,-111.698361246109,
177.646659841956));
#24374=CARTESIAN_POINT('Ctrl Pts',(-61.7191976091278,-111.729657089422,
178.821287620784));
#24375=CARTESIAN_POINT('Ctrl Pts',(-60.5412501220053,-111.760952932734,
179.995915399612));
#24376=CARTESIAN_POINT('Ctrl Pts',(-58.8794973595142,-111.843825650653,
179.995915330104));
#24377=CARTESIAN_POINT('Ctrl Pts',(-57.217744597023,-111.926698368571,179.995915260595));
#24378=CARTESIAN_POINT('Ctrl Pts',(-56.0397972076466,-111.957994201463,
178.821287383467));
#24379=CARTESIAN_POINT('Ctrl Pts',(-54.8618498182701,-111.989290034355,
177.646659506339));
#24380=CARTESIAN_POINT('Ctrl Pts',(-54.85191182447,-111.896068262332,175.985484901271));
#24381=CARTESIAN_POINT('Ctrl Pts',(-54.8419738306699,-111.802846490308,
174.324310296203));
#24382=CARTESIAN_POINT('Ctrl Pts',(-56.0000451919584,-111.585107117685,
173.149682517375));
#24383=CARTESIAN_POINT('Ctrl Pts',(-57.158116553247,-111.367367745062,171.975054738546));
#24384=CARTESIAN_POINT('Ctrl Pts',(-58.799993189904,-111.098051497832,171.975054808055));
#24385=CARTESIAN_POINT('Ctrl Pts',(-60.4418698265612,-110.828735250603,
171.975054877564));
#24386=CARTESIAN_POINT('Ctrl Pts',(-61.5999410901036,-110.6109958884,173.149682754692));
#24387=CARTESIAN_POINT('Ctrl Pts',(-62.758012353646,-110.393256526198,174.32431063182));
#24388=CARTESIAN_POINT('Ctrl Pts',(-62.7480742216121,-110.30003476891,175.985485236888));
#24389=CARTESIAN_POINT('Ctrl Pts',(-62.7381360895782,-110.206813011623,
177.646659841956));
#24390=CARTESIAN_POINT('Ctrl Pts',(-61.5601886024556,-110.238108854936,
178.821287620784));
#24391=CARTESIAN_POINT('Ctrl Pts',(-60.3822411153331,-110.269404698248,
179.995915399612));
#24392=CARTESIAN_POINT('Ctrl Pts',(-58.7204883528419,-110.352277416167,
179.995915330104));
#24393=CARTESIAN_POINT('Ctrl Pts',(-57.0587355903508,-110.435150134086,
179.995915260595));
#24394=CARTESIAN_POINT('Ctrl Pts',(-55.8807882009743,-110.466445966978,
178.821287383467));
#24395=CARTESIAN_POINT('Ctrl Pts',(-54.7028408115979,-110.49774179987,177.646659506339));
#24396=CARTESIAN_POINT('Ctrl Pts',(-54.6929028177978,-110.404520027846,
175.985484901271));
#24397=CARTESIAN_POINT('Ctrl Pts',(-54.6829648239977,-110.311298255822,
174.324310296203));
#24398=CARTESIAN_POINT('Ctrl Pts',(-55.8410361852862,-110.093558883199,
173.149682517375));
#24399=CARTESIAN_POINT('Ctrl Pts',(-56.9991075465747,-109.875819510576,
171.975054738546));
#24400=CARTESIAN_POINT('Ctrl Pts',(-58.6409841832318,-109.606503263347,
171.975054808055));
#24401=CARTESIAN_POINT('Ctrl Pts',(-60.2828608198889,-109.337187016117,
171.975054877564));
#24402=CARTESIAN_POINT('Ctrl Pts',(-61.4409320834313,-109.119447653915,
173.149682754692));
#24403=CARTESIAN_POINT('Ctrl Pts',(-62.5990033469738,-108.901708291712,
174.32431063182));
#24404=CARTESIAN_POINT('Ctrl Pts',(-62.5890652149398,-108.808486534425,
175.985485236888));
#24405=CARTESIAN_POINT('Ctrl Pts',(-62.5791270829059,-108.715264777138,
177.646659841956));
#24406=CARTESIAN_POINT('Ctrl Pts',(-61.4011795957834,-108.74656062045,178.821287620784));
#24407=CARTESIAN_POINT('Ctrl Pts',(-60.2232321086609,-108.777856463763,
179.995915399612));
#24408=CARTESIAN_POINT('Ctrl Pts',(-58.5614793461697,-108.860729181681,
179.995915330104));
#24409=CARTESIAN_POINT('Ctrl Pts',(-56.8997265836786,-108.9436018996,179.995915260595));
#24410=CARTESIAN_POINT('Ctrl Pts',(-55.7217791943021,-108.974897732492,
178.821287383467));
#24411=CARTESIAN_POINT('Ctrl Pts',(-54.5438318049257,-109.006193565384,
177.646659506339));
#24412=CARTESIAN_POINT('Ctrl Pts',(-54.5338938111256,-108.91297179336,175.985484901271));
#24413=CARTESIAN_POINT('Ctrl Pts',(-54.5239558173255,-108.819750021337,
174.324310296203));
#24414=CARTESIAN_POINT('Ctrl Pts',(-55.682027178614,-108.602010648714,173.149682517375));
#24415=CARTESIAN_POINT('Ctrl Pts',(-56.8400985399025,-108.384271276091,
171.975054738546));
#24416=CARTESIAN_POINT('Ctrl Pts',(-58.4819751765596,-108.114955028861,
171.975054808055));
#24417=CARTESIAN_POINT('Ctrl Pts',(-60.1238518132167,-107.845638781632,
171.975054877564));
#24418=CARTESIAN_POINT('Ctrl Pts',(-61.2819230767591,-107.627899419429,
173.149682754692));
#24419=CARTESIAN_POINT('Ctrl Pts',(-62.4399943403016,-107.410160057226,
174.32431063182));
#24420=CARTESIAN_POINT('Ctrl Pts',(-62.4300562082676,-107.316938299939,
175.985485236888));
#24421=CARTESIAN_POINT('Ctrl Pts',(-62.4201180762337,-107.223716542652,
177.646659841956));
#24422=CARTESIAN_POINT('Ctrl Pts',(-61.2421705891111,-107.255012385965,
178.821287620784));
#24423=CARTESIAN_POINT('Ctrl Pts',(-60.0642231019886,-107.286308229277,
179.995915399612));
#24424=CARTESIAN_POINT('Ctrl Pts',(-58.4024703394975,-107.369180947196,
179.995915330104));
#24425=CARTESIAN_POINT('Ctrl Pts',(-56.7407175770064,-107.452053665114,
179.995915260595));
#24426=CARTESIAN_POINT('Ctrl Pts',(-55.5627701876299,-107.483349498006,
178.821287383467));
#24427=CARTESIAN_POINT('Ctrl Pts',(-54.3848227982534,-107.514645330899,
177.646659506339));
#24428=CARTESIAN_POINT('Ctrl Pts',(-54.3748848044533,-107.421423558875,
175.985484901271));
#24429=CARTESIAN_POINT('Ctrl Pts',(-54.3649468106533,-107.328201786851,
174.324310296203));
#24430=CARTESIAN_POINT('Ctrl Pts',(-55.5230181719417,-107.110462414228,
173.149682517375));
#24431=CARTESIAN_POINT('Ctrl Pts',(-56.6810895332303,-106.892723041605,
171.975054738546));
#24432=CARTESIAN_POINT('Ctrl Pts',(-58.3229661698874,-106.623406794376,
171.975054808055));
#24433=CARTESIAN_POINT('Ctrl Pts',(-59.9648428065445,-106.354090547146,
171.975054877564));
#24434=CARTESIAN_POINT('Ctrl Pts',(-61.1229140700869,-106.136351184943,
173.149682754692));
#24435=CARTESIAN_POINT('Ctrl Pts',(-62.2809853336293,-105.918611822741,
174.32431063182));
#24436=CARTESIAN_POINT('Ctrl Pts',(-62.2710472015954,-105.825390065454,
175.985485236888));
#24437=CARTESIAN_POINT('Ctrl Pts',(-62.2611090695615,-105.732168308167,
177.646659841956));
#24438=CARTESIAN_POINT('Ctrl Pts',(-61.0831615824389,-105.763464151479,
178.821287620784));
#24439=CARTESIAN_POINT('Ctrl Pts',(-59.9052140953164,-105.794759994792,
179.995915399612));
#24440=CARTESIAN_POINT('Ctrl Pts',(-58.2434613328252,-105.87763271271,179.995915330104));
#24441=CARTESIAN_POINT('Ctrl Pts',(-56.5817085703341,-105.960505430629,
179.995915260595));
#24442=CARTESIAN_POINT('Ctrl Pts',(-55.4037611809577,-105.991801263521,
178.821287383467));
#24443=CARTESIAN_POINT('Ctrl Pts',(-54.2258137915812,-106.023097096413,
177.646659506339));
#24444=CARTESIAN_POINT('Ctrl Pts',(-54.2158757977811,-105.929875324389,
175.985484901271));
#24445=CARTESIAN_POINT('Ctrl Pts',(-54.205937803981,-105.836653552366,174.324310296203));
#24446=CARTESIAN_POINT('Ctrl Pts',(-55.3640091652695,-105.618914179742,
173.149682517375));
#24447=CARTESIAN_POINT('Ctrl Pts',(-56.522080526558,-105.401174807119,171.975054738546));
#24448=CARTESIAN_POINT('Ctrl Pts',(-58.1639571632151,-105.13185855989,171.975054808055));
#24449=CARTESIAN_POINT('Ctrl Pts',(-59.8058337998722,-104.862542312661,
171.975054877564));
#24450=CARTESIAN_POINT('Ctrl Pts',(-60.9639050634147,-104.644802950458,
173.149682754692));
#24451=CARTESIAN_POINT('Ctrl Pts',(-62.1219763269571,-104.427063588255,
174.32431063182));
#24452=CARTESIAN_POINT('Ctrl Pts',(-62.1120381949232,-104.333841830968,
175.985485236888));
#24453=CARTESIAN_POINT('Ctrl Pts',(-62.1021000628892,-104.240620073681,
177.646659841956));
#24454=CARTESIAN_POINT('Ctrl Pts',(-60.9241525757667,-104.271915916993,
178.821287620784));
#24455=CARTESIAN_POINT('Ctrl Pts',(-59.7462050886442,-104.303211760306,
179.995915399612));
#24456=CARTESIAN_POINT('Ctrl Pts',(-58.084452326153,-104.386084478225,179.995915330104));
#24457=CARTESIAN_POINT('Ctrl Pts',(-56.4226995636619,-104.468957196143,
179.995915260595));
#24458=CARTESIAN_POINT('Ctrl Pts',(-55.2447521742854,-104.500253029035,
178.821287383467));
#24459=CARTESIAN_POINT('Ctrl Pts',(-54.066804784909,-104.531548861927,177.646659506339));
#24460=CARTESIAN_POINT('Ctrl Pts',(-54.0568667911089,-104.438327089904,
175.985484901271));
#24461=CARTESIAN_POINT('Ctrl Pts',(-54.0469287973088,-104.34510531788,174.324310296203));
#24462=CARTESIAN_POINT('Ctrl Pts',(-55.2050001585973,-104.127365945257,
173.149682517375));
#24463=CARTESIAN_POINT('Ctrl Pts',(-56.3630715198858,-103.909626572634,
171.975054738546));
#24464=CARTESIAN_POINT('Ctrl Pts',(-58.0049481565429,-103.640310325404,
171.975054808055));
#24465=CARTESIAN_POINT('Ctrl Pts',(-59.6468247932,-103.370994078175,171.975054877564));
#24466=CARTESIAN_POINT('Ctrl Pts',(-60.8048960567424,-103.153254715972,
173.149682754692));
#24467=CARTESIAN_POINT('Ctrl Pts',(-61.9629673202849,-102.93551535377,174.32431063182));
#24468=CARTESIAN_POINT('Ctrl Pts',(-61.9530291882509,-102.842293596483,
175.985485236888));
#24469=CARTESIAN_POINT('Ctrl Pts',(-61.943091056217,-102.749071839196,177.646659841956));
#24470=CARTESIAN_POINT('Ctrl Pts',(-60.7651435690945,-102.780367682508,
178.821287620784));
#24471=CARTESIAN_POINT('Ctrl Pts',(-59.587196081972,-102.81166352582,179.995915399612));
#24472=CARTESIAN_POINT('Ctrl Pts',(-57.9254433194808,-102.894536243739,
179.995915330104));
#24473=CARTESIAN_POINT('Ctrl Pts',(-56.2636905569897,-102.977408961658,
179.995915260595));
#24474=CARTESIAN_POINT('Ctrl Pts',(-55.0857431676132,-103.00870479455,178.821287383467));
#24475=CARTESIAN_POINT('Ctrl Pts',(-53.9077957782368,-103.040000627442,
177.646659506339));
#24476=CARTESIAN_POINT('Ctrl Pts',(-53.8978577844367,-102.946778855418,
175.985484901271));
#24477=CARTESIAN_POINT('Ctrl Pts',(-53.8879197906366,-102.853557083394,
174.324310296203));
#24478=CARTESIAN_POINT('Ctrl Pts',(-55.0459911519251,-102.635817710771,
173.149682517375));
#24479=CARTESIAN_POINT('Ctrl Pts',(-56.2040625132136,-102.418078338148,
171.975054738546));
#24480=CARTESIAN_POINT('Ctrl Pts',(-57.8459391498707,-102.148762090919,
171.975054808055));
#24481=CARTESIAN_POINT('Ctrl Pts',(-59.4878157865278,-101.879445843689,
171.975054877564));
#24482=CARTESIAN_POINT('Ctrl Pts',(-60.6458870500702,-101.661706481487,
173.149682754692));
#24483=CARTESIAN_POINT('Ctrl Pts',(-61.8039583136126,-101.443967119284,
174.32431063182));
#24484=CARTESIAN_POINT('Ctrl Pts',(-61.7940201815787,-101.350745361997,
175.985485236888));
#24485=CARTESIAN_POINT('Ctrl Pts',(-61.7840820495448,-101.25752360471,177.646659841956));
#24486=CARTESIAN_POINT('Ctrl Pts',(-60.6061345624222,-101.288819448022,
178.821287620784));
#24487=CARTESIAN_POINT('Ctrl Pts',(-59.4281870752997,-101.320115291335,
179.995915399612));
#24488=CARTESIAN_POINT('Ctrl Pts',(-57.7664343128086,-101.402988009253,
179.995915330104));
#24489=CARTESIAN_POINT('Ctrl Pts',(-56.1046815503175,-101.485860727172,
179.995915260595));
#24490=CARTESIAN_POINT('Ctrl Pts',(-54.926734160941,-101.517156560064,178.821287383467));
#24491=CARTESIAN_POINT('Ctrl Pts',(-53.7487867715645,-101.548452392956,
177.646659506339));
#24492=CARTESIAN_POINT('Ctrl Pts',(-53.7388487777644,-101.455230620932,
175.985484901271));
#24493=CARTESIAN_POINT('Ctrl Pts',(-53.7289107839643,-101.362008848909,
174.324310296203));
#24494=CARTESIAN_POINT('Ctrl Pts',(-54.8869821452528,-101.144269476286,
173.149682517375));
#24495=CARTESIAN_POINT('Ctrl Pts',(-56.0450535065414,-100.926530103662,
171.975054738546));
#24496=CARTESIAN_POINT('Ctrl Pts',(-57.6869301431984,-100.657213856433,
171.975054808055));
#24497=CARTESIAN_POINT('Ctrl Pts',(-59.3288067798556,-100.387897609204,
171.975054877564));
#24498=CARTESIAN_POINT('Ctrl Pts',(-60.486878043398,-100.170158247001,173.149682754692));
#24499=CARTESIAN_POINT('Ctrl Pts',(-61.6449493069404,-99.9524188847983,
174.32431063182));
#24500=CARTESIAN_POINT('Ctrl Pts',(-61.6350111749065,-99.8591971275113,
175.985485236888));
#24501=CARTESIAN_POINT('Ctrl Pts',(-61.6250730428726,-99.7659753702243,
177.646659841956));
#24502=CARTESIAN_POINT('Ctrl Pts',(-60.44712555575,-99.7972712135367,178.821287620784));
#24503=CARTESIAN_POINT('Ctrl Pts',(-59.2691780686275,-99.8285670568492,
179.995915399612));
#24504=CARTESIAN_POINT('Ctrl Pts',(-57.6074253061363,-99.9114397747677,
179.995915330104));
#24505=CARTESIAN_POINT('Ctrl Pts',(-55.9456725436452,-99.9943124926864,
179.995915260595));
#24506=CARTESIAN_POINT('Ctrl Pts',(-54.7677251542687,-100.025608325578,
178.821287383467));
#24507=CARTESIAN_POINT('Ctrl Pts',(-53.5897777648923,-100.05690415847,177.646659506339));
#24508=CARTESIAN_POINT('Ctrl Pts',(-53.5798397710922,-99.9636823864468,
175.985484901271));
#24509=CARTESIAN_POINT('Ctrl Pts',(-53.5699017772921,-99.8704606144232,
174.324310296203));
#24510=CARTESIAN_POINT('Ctrl Pts',(-54.7279731385806,-99.6527212418,173.149682517375));
#24511=CARTESIAN_POINT('Ctrl Pts',(-55.8860444998691,-99.4349818691769,
171.975054738546));
#24512=CARTESIAN_POINT('Ctrl Pts',(-57.5279211365262,-99.1656656219475,
171.975054808055));
#24513=CARTESIAN_POINT('Ctrl Pts',(-59.1697977731833,-98.8963493747183,
171.975054877564));
#24514=CARTESIAN_POINT('Ctrl Pts',(-60.3278690367257,-98.6786100125155,
173.149682754692));
#24515=CARTESIAN_POINT('Ctrl Pts',(-61.4859403002682,-98.4608706503128,
174.32431063182));
#24516=CARTESIAN_POINT('Ctrl Pts',(-61.4760021682342,-98.3676488930257,
175.985485236888));
#24517=CARTESIAN_POINT('Ctrl Pts',(-61.4660640362003,-98.2744271357387,
177.646659841956));
#24518=CARTESIAN_POINT('Ctrl Pts',(-60.2881165490778,-98.3057229790511,
178.821287620784));
#24519=CARTESIAN_POINT('Ctrl Pts',(-59.1101690619552,-98.3370188223636,
179.995915399612));
#24520=CARTESIAN_POINT('Ctrl Pts',(-57.4484162994641,-98.4198915402821,
179.995915330104));
#24521=CARTESIAN_POINT('Ctrl Pts',(-55.786663536973,-98.5027642582008,179.995915260595));
#24522=CARTESIAN_POINT('Ctrl Pts',(-54.6087161475965,-98.5340600910929,
178.821287383467));
#24523=CARTESIAN_POINT('Ctrl Pts',(-56.2237961054143,-113.614380048479,
178.813912075476));
#24524=CARTESIAN_POINT('Ctrl Pts',(-55.0488864554725,-113.645352038053,
177.6423391512));
#24525=CARTESIAN_POINT('Ctrl Pts',(-55.0389484614927,-113.552130266048,
175.985484901707));
#24526=CARTESIAN_POINT('Ctrl Pts',(-55.0290104675128,-113.458908494044,
174.328630652215));
#24527=CARTESIAN_POINT('Ctrl Pts',(-56.1840440891124,-113.241492964766,
173.157057825983));
#24528=CARTESIAN_POINT('Ctrl Pts',(-57.3390777107121,-113.024077435489,
171.985484999752));
#24529=CARTESIAN_POINT('Ctrl Pts',(-58.9766583348819,-112.755219171892,
171.985485069079));
#24530=CARTESIAN_POINT('Ctrl Pts',(-60.6142389590518,-112.486360908295,
171.985485138407));
#24531=CARTESIAN_POINT('Ctrl Pts',(-61.7692724831595,-112.268945389411,
173.157058062683));
#24532=CARTESIAN_POINT('Ctrl Pts',(-62.9243060072673,-112.051529870527,
174.328630986959));
#24533=CARTESIAN_POINT('Ctrl Pts',(-62.9143678754131,-111.95830811322,175.985485236451));
#24534=CARTESIAN_POINT('Ctrl Pts',(-62.9044297435589,-111.865086355914,
177.642339485944));
#24535=CARTESIAN_POINT('Ctrl Pts',(-61.7295199961253,-111.896058355881,
178.813912312176));
#24536=CARTESIAN_POINT('Ctrl Pts',(-60.5546102486917,-111.927030355848,
179.985485138407));
#24537=CARTESIAN_POINT('Ctrl Pts',(-58.8971534986878,-112.009445090134,
179.985485069079));
#24538=CARTESIAN_POINT('Ctrl Pts',(-57.2396967486839,-112.09185982442,179.985484999752));
#24539=CARTESIAN_POINT('Ctrl Pts',(-56.0647870987421,-112.122831813994,
178.813912075476));
#24540=CARTESIAN_POINT('Ctrl Pts',(-54.8898774488003,-112.153803803567,
177.6423391512));
#24541=CARTESIAN_POINT('Ctrl Pts',(-54.8799394548205,-112.060582031563,
175.985484901707));
#24542=CARTESIAN_POINT('Ctrl Pts',(-54.8700014608406,-111.967360259558,
174.328630652215));
#24543=CARTESIAN_POINT('Ctrl Pts',(-56.0250350824402,-111.749944730281,
173.157057825983));
#24544=CARTESIAN_POINT('Ctrl Pts',(-57.1800687040398,-111.532529201003,
171.985484999752));
#24545=CARTESIAN_POINT('Ctrl Pts',(-58.8176493282097,-111.263670937406,
171.985485069079));
#24546=CARTESIAN_POINT('Ctrl Pts',(-60.4552299523796,-110.994812673809,
171.985485138407));
#24547=CARTESIAN_POINT('Ctrl Pts',(-61.6102634764873,-110.777397154925,
173.157058062683));
#24548=CARTESIAN_POINT('Ctrl Pts',(-62.7652970005951,-110.559981636041,
174.328630986959));
#24549=CARTESIAN_POINT('Ctrl Pts',(-62.7553588687409,-110.466759878735,
175.985485236451));
#24550=CARTESIAN_POINT('Ctrl Pts',(-62.7454207368867,-110.373538121429,
177.642339485944));
#24551=CARTESIAN_POINT('Ctrl Pts',(-61.5705109894531,-110.404510121395,
178.813912312176));
#24552=CARTESIAN_POINT('Ctrl Pts',(-60.3956012420194,-110.435482121362,
179.985485138407));
#24553=CARTESIAN_POINT('Ctrl Pts',(-58.7381444920155,-110.517896855648,
179.985485069079));
#24554=CARTESIAN_POINT('Ctrl Pts',(-57.0806877420116,-110.600311589935,
179.985484999752));
#24555=CARTESIAN_POINT('Ctrl Pts',(-55.9057780920699,-110.631283579508,
178.813912075476));
#24556=CARTESIAN_POINT('Ctrl Pts',(-54.7308684421281,-110.662255569082,
177.6423391512));
#24557=CARTESIAN_POINT('Ctrl Pts',(-54.7209304481482,-110.569033797077,
175.985484901707));
#24558=CARTESIAN_POINT('Ctrl Pts',(-54.7109924541684,-110.475812025073,
174.328630652215));
#24559=CARTESIAN_POINT('Ctrl Pts',(-55.866026075768,-110.258396495795,173.157057825983));
#24560=CARTESIAN_POINT('Ctrl Pts',(-57.0210596973676,-110.040980966518,
171.985484999752));
#24561=CARTESIAN_POINT('Ctrl Pts',(-58.6586403215375,-109.772122702921,
171.985485069079));
#24562=CARTESIAN_POINT('Ctrl Pts',(-60.2962209457073,-109.503264439324,
171.985485138407));
#24563=CARTESIAN_POINT('Ctrl Pts',(-61.4512544698151,-109.28584892044,173.157058062683));
#24564=CARTESIAN_POINT('Ctrl Pts',(-62.6062879939228,-109.068433401555,
174.328630986959));
#24565=CARTESIAN_POINT('Ctrl Pts',(-62.5963498620687,-108.975211644249,
175.985485236451));
#24566=CARTESIAN_POINT('Ctrl Pts',(-62.5864117302145,-108.881989886943,
177.642339485944));
#24567=CARTESIAN_POINT('Ctrl Pts',(-61.4115019827808,-108.91296188691,178.813912312176));
#24568=CARTESIAN_POINT('Ctrl Pts',(-60.2365922353472,-108.943933886877,
179.985485138407));
#24569=CARTESIAN_POINT('Ctrl Pts',(-58.5791354853433,-109.026348621163,
179.985485069079));
#24570=CARTESIAN_POINT('Ctrl Pts',(-56.9216787353394,-109.108763355449,
179.985484999752));
#24571=CARTESIAN_POINT('Ctrl Pts',(-55.7467690853976,-109.139735345023,
178.813912075476));
#24572=CARTESIAN_POINT('Ctrl Pts',(-54.5718594354559,-109.170707334596,
177.6423391512));
#24573=CARTESIAN_POINT('Ctrl Pts',(-54.561921441476,-109.077485562592,175.985484901707));
#24574=CARTESIAN_POINT('Ctrl Pts',(-54.5519834474962,-108.984263790587,
174.328630652215));
#24575=CARTESIAN_POINT('Ctrl Pts',(-55.7070170690958,-108.76684826131,173.157057825983));
#24576=CARTESIAN_POINT('Ctrl Pts',(-56.8620506906954,-108.549432732032,
171.985484999752));
#24577=CARTESIAN_POINT('Ctrl Pts',(-58.4996313148652,-108.280574468435,
171.985485069079));
#24578=CARTESIAN_POINT('Ctrl Pts',(-60.1372119390351,-108.011716204838,
171.985485138407));
#24579=CARTESIAN_POINT('Ctrl Pts',(-61.2922454631428,-107.794300685954,
173.157058062683));
#24580=CARTESIAN_POINT('Ctrl Pts',(-62.4472789872506,-107.57688516707,174.328630986959));
#24581=CARTESIAN_POINT('Ctrl Pts',(-62.4373408553964,-107.483663409764,
175.985485236451));
#24582=CARTESIAN_POINT('Ctrl Pts',(-62.4274027235423,-107.390441652457,
177.642339485944));
#24583=CARTESIAN_POINT('Ctrl Pts',(-61.2524929761086,-107.421413652424,
178.813912312176));
#24584=CARTESIAN_POINT('Ctrl Pts',(-60.077583228675,-107.452385652391,179.985485138407));
#24585=CARTESIAN_POINT('Ctrl Pts',(-58.4201264786711,-107.534800386677,
179.985485069079));
#24586=CARTESIAN_POINT('Ctrl Pts',(-56.7626697286672,-107.617215120964,
179.985484999752));
#24587=CARTESIAN_POINT('Ctrl Pts',(-55.5877600787254,-107.648187110537,
178.813912075476));
#24588=CARTESIAN_POINT('Ctrl Pts',(-54.4128504287836,-107.67915910011,177.6423391512));
#24589=CARTESIAN_POINT('Ctrl Pts',(-54.4029124348038,-107.585937328106,
175.985484901707));
#24590=CARTESIAN_POINT('Ctrl Pts',(-54.3929744408239,-107.492715556102,
174.328630652215));
#24591=CARTESIAN_POINT('Ctrl Pts',(-55.5480080624235,-107.275300026824,
173.157057825983));
#24592=CARTESIAN_POINT('Ctrl Pts',(-56.7030416840231,-107.057884497547,
171.985484999752));
#24593=CARTESIAN_POINT('Ctrl Pts',(-58.340622308193,-106.78902623395,171.985485069079));
#24594=CARTESIAN_POINT('Ctrl Pts',(-59.9782029323629,-106.520167970353,
171.985485138407));
#24595=CARTESIAN_POINT('Ctrl Pts',(-61.1332364564706,-106.302752451468,
173.157058062683));
#24596=CARTESIAN_POINT('Ctrl Pts',(-62.2882699805784,-106.085336932584,
174.328630986959));
#24597=CARTESIAN_POINT('Ctrl Pts',(-62.2783318487242,-105.992115175278,
175.985485236451));
#24598=CARTESIAN_POINT('Ctrl Pts',(-62.26839371687,-105.898893417972,177.642339485944));
#24599=CARTESIAN_POINT('Ctrl Pts',(-61.0934839694364,-105.929865417939,
178.813912312176));
#24600=CARTESIAN_POINT('Ctrl Pts',(-59.9185742220028,-105.960837417905,
179.985485138407));
#24601=CARTESIAN_POINT('Ctrl Pts',(-58.2611174719989,-106.043252152192,
179.985485069079));
#24602=CARTESIAN_POINT('Ctrl Pts',(-56.603660721995,-106.125666886478,179.985484999752));
#24603=CARTESIAN_POINT('Ctrl Pts',(-55.4287510720532,-106.156638876051,
178.813912075476));
#24604=CARTESIAN_POINT('Ctrl Pts',(-54.2538414221114,-106.187610865625,
177.6423391512));
#24605=CARTESIAN_POINT('Ctrl Pts',(-54.2439034281315,-106.09438909362,175.985484901707));
#24606=CARTESIAN_POINT('Ctrl Pts',(-54.2339654341517,-106.001167321616,
174.328630652215));
#24607=CARTESIAN_POINT('Ctrl Pts',(-55.3889990557513,-105.783751792338,
173.157057825983));
#24608=CARTESIAN_POINT('Ctrl Pts',(-56.5440326773509,-105.566336263061,
171.985484999752));
#24609=CARTESIAN_POINT('Ctrl Pts',(-58.1816133015208,-105.297477999464,
171.985485069079));
#24610=CARTESIAN_POINT('Ctrl Pts',(-59.8191939256906,-105.028619735867,
171.985485138407));
#24611=CARTESIAN_POINT('Ctrl Pts',(-60.9742274497984,-104.811204216983,
173.157058062683));
#24612=CARTESIAN_POINT('Ctrl Pts',(-62.1292609739061,-104.593788698099,
174.328630986959));
#24613=CARTESIAN_POINT('Ctrl Pts',(-62.119322842052,-104.500566940792,175.985485236451));
#24614=CARTESIAN_POINT('Ctrl Pts',(-62.1093847101978,-104.407345183486,
177.642339485944));
#24615=CARTESIAN_POINT('Ctrl Pts',(-60.9344749627642,-104.438317183453,
178.813912312176));
#24616=CARTESIAN_POINT('Ctrl Pts',(-59.7595652153305,-104.46928918342,179.985485138407));
#24617=CARTESIAN_POINT('Ctrl Pts',(-58.1021084653266,-104.551703917706,
179.985485069079));
#24618=CARTESIAN_POINT('Ctrl Pts',(-56.4446517153227,-104.634118651992,
179.985484999752));
#24619=CARTESIAN_POINT('Ctrl Pts',(-55.269742065381,-104.665090641566,178.813912075476));
#24620=CARTESIAN_POINT('Ctrl Pts',(-54.0948324154392,-104.696062631139,
177.6423391512));
#24621=CARTESIAN_POINT('Ctrl Pts',(-54.0848944214593,-104.602840859135,
175.985484901707));
#24622=CARTESIAN_POINT('Ctrl Pts',(-54.0749564274795,-104.50961908713,174.328630652215));
#24623=CARTESIAN_POINT('Ctrl Pts',(-55.2299900490791,-104.292203557853,
173.157057825983));
#24624=CARTESIAN_POINT('Ctrl Pts',(-56.3850236706787,-104.074788028575,
171.985484999752));
#24625=CARTESIAN_POINT('Ctrl Pts',(-58.0226042948486,-103.805929764978,
171.985485069079));
#24626=CARTESIAN_POINT('Ctrl Pts',(-59.6601849190184,-103.537071501381,
171.985485138407));
#24627=CARTESIAN_POINT('Ctrl Pts',(-60.8152184431262,-103.319655982497,
173.157058062683));
#24628=CARTESIAN_POINT('Ctrl Pts',(-61.9702519672339,-103.102240463613,
174.328630986959));
#24629=CARTESIAN_POINT('Ctrl Pts',(-61.9603138353797,-103.009018706307,
175.985485236451));
#24630=CARTESIAN_POINT('Ctrl Pts',(-61.9503757035256,-102.915796949001,
177.642339485944));
#24631=CARTESIAN_POINT('Ctrl Pts',(-60.7754659560919,-102.946768948967,
178.813912312176));
#24632=CARTESIAN_POINT('Ctrl Pts',(-59.6005562086583,-102.977740948934,
179.985485138407));
#24633=CARTESIAN_POINT('Ctrl Pts',(-57.9430994586544,-103.06015568322,179.985485069079));
#24634=CARTESIAN_POINT('Ctrl Pts',(-56.2856427086505,-103.142570417507,
179.985484999752));
#24635=CARTESIAN_POINT('Ctrl Pts',(-55.1107330587087,-103.17354240708,178.813912075476));
#24636=CARTESIAN_POINT('Ctrl Pts',(-53.935823408767,-103.204514396654,177.6423391512));
#24637=CARTESIAN_POINT('Ctrl Pts',(-53.9258854147871,-103.111292624649,
175.985484901707));
#24638=CARTESIAN_POINT('Ctrl Pts',(-53.9159474208072,-103.018070852645,
174.328630652215));
#24639=CARTESIAN_POINT('Ctrl Pts',(-55.0709810424069,-102.800655323367,
173.157057825983));
#24640=CARTESIAN_POINT('Ctrl Pts',(-56.2260146640065,-102.58323979409,171.985484999752));
#24641=CARTESIAN_POINT('Ctrl Pts',(-57.8635952881763,-102.314381530493,
171.985485069079));
#24642=CARTESIAN_POINT('Ctrl Pts',(-59.5011759123462,-102.045523266896,
171.985485138407));
#24643=CARTESIAN_POINT('Ctrl Pts',(-60.6562094364539,-101.828107748012,
173.157058062683));
#24644=CARTESIAN_POINT('Ctrl Pts',(-61.8112429605617,-101.610692229127,
174.328630986959));
#24645=CARTESIAN_POINT('Ctrl Pts',(-61.8013048287075,-101.517470471821,
175.985485236451));
#24646=CARTESIAN_POINT('Ctrl Pts',(-61.7913666968533,-101.424248714515,
177.642339485944));
#24647=CARTESIAN_POINT('Ctrl Pts',(-60.6164569494197,-101.455220714482,
178.813912312176));
#24648=CARTESIAN_POINT('Ctrl Pts',(-59.4415472019861,-101.486192714449,
179.985485138407));
#24649=CARTESIAN_POINT('Ctrl Pts',(-57.7840904519822,-101.568607448735,
179.985485069079));
#24650=CARTESIAN_POINT('Ctrl Pts',(-56.1266337019783,-101.651022183021,
179.985484999752));
#24651=CARTESIAN_POINT('Ctrl Pts',(-54.9517240520365,-101.681994172595,
178.813912075476));
#24652=CARTESIAN_POINT('Ctrl Pts',(-53.7768144020947,-101.712966162168,
177.6423391512));
#24653=CARTESIAN_POINT('Ctrl Pts',(-53.7668764081149,-101.619744390164,
175.985484901707));
#24654=CARTESIAN_POINT('Ctrl Pts',(-53.756938414135,-101.526522618159,174.328630652215));
#24655=CARTESIAN_POINT('Ctrl Pts',(-54.9119720357346,-101.309107088882,
173.157057825983));
#24656=CARTESIAN_POINT('Ctrl Pts',(-56.0670056573342,-101.091691559604,
171.985484999752));
#24657=CARTESIAN_POINT('Ctrl Pts',(-57.7045862815041,-100.822833296007,
171.985485069079));
#24658=CARTESIAN_POINT('Ctrl Pts',(-59.342166905674,-100.55397503241,171.985485138407));
#24659=CARTESIAN_POINT('Ctrl Pts',(-60.4972004297817,-100.336559513526,
173.157058062683));
#24660=CARTESIAN_POINT('Ctrl Pts',(-61.6522339538895,-100.119143994642,
174.328630986959));
#24661=CARTESIAN_POINT('Ctrl Pts',(-61.6422958220353,-100.025922237336,
175.985485236451));
#24662=CARTESIAN_POINT('Ctrl Pts',(-61.6323576901811,-99.9327004800294,
177.642339485944));
#24663=CARTESIAN_POINT('Ctrl Pts',(-60.4574479427475,-99.9636724799962,
178.813912312176));
#24664=CARTESIAN_POINT('Ctrl Pts',(-59.2825381953138,-99.994644479963,179.985485138407));
#24665=CARTESIAN_POINT('Ctrl Pts',(-57.6250814453099,-100.077059214249,
179.985485069079));
#24666=CARTESIAN_POINT('Ctrl Pts',(-55.9676246953061,-100.159473948536,
179.985484999752));
#24667=CARTESIAN_POINT('Ctrl Pts',(-54.7927150453643,-100.190445938109,
178.813912075476));
#24668=CARTESIAN_POINT('Ctrl Pts',(-53.6178053954225,-100.221417927683,
177.6423391512));
#24669=CARTESIAN_POINT('Ctrl Pts',(-53.6078674014426,-100.128196155678,
175.985484901707));
#24670=CARTESIAN_POINT('Ctrl Pts',(-53.5979294074628,-100.034974383673,
174.328630652215));
#24671=CARTESIAN_POINT('Ctrl Pts',(-54.7529630290624,-99.817558854396,173.157057825983));
#24672=CARTESIAN_POINT('Ctrl Pts',(-55.907996650662,-99.6001433251185,171.985484999752));
#24673=CARTESIAN_POINT('Ctrl Pts',(-57.5455772748319,-99.3312850615215,
171.985485069079));
#24674=CARTESIAN_POINT('Ctrl Pts',(-59.1831578990017,-99.0624267979246,
171.985485138407));
#24675=CARTESIAN_POINT('Ctrl Pts',(-60.3381914231095,-98.8450112790404,
173.157058062683));
#24676=CARTESIAN_POINT('Ctrl Pts',(-61.4932249472172,-98.6275957601562,
174.328630986959));
#24677=CARTESIAN_POINT('Ctrl Pts',(-61.4832868153631,-98.53437400285,175.985485236451));
#24678=CARTESIAN_POINT('Ctrl Pts',(-61.4733486835089,-98.4411522455438,
177.642339485944));
#24679=CARTESIAN_POINT('Ctrl Pts',(-60.2984389360752,-98.4721242455106,
178.813912312176));
#24680=CARTESIAN_POINT('Ctrl Pts',(-59.1235291886416,-98.5030962454774,
179.985485138407));
#24681=CARTESIAN_POINT('Ctrl Pts',(-57.4660724386377,-98.5855109797636,
179.985485069079));
#24682=CARTESIAN_POINT('Ctrl Pts',(-55.8086156886338,-98.6679257140499,
179.985484999752));
#24683=CARTESIAN_POINT('Ctrl Pts',(-54.633706038692,-98.6988977036234,178.813912075476));
#24684=CARTESIAN_POINT('Ctrl Pts',(-56.2237961054143,-113.614380048479,
178.813912075476));
#24685=CARTESIAN_POINT('Ctrl Pts',(-55.0488864554725,-113.645352038053,
177.6423391512));
#24686=CARTESIAN_POINT('Ctrl Pts',(-55.0389484614927,-113.552130266048,
175.985484901707));
#24687=CARTESIAN_POINT('Ctrl Pts',(-55.0290104675128,-113.458908494044,
174.328630652215));
#24688=CARTESIAN_POINT('Ctrl Pts',(-56.1840440891124,-113.241492964766,
173.157057825983));
#24689=CARTESIAN_POINT('Ctrl Pts',(-57.3390777107121,-113.024077435489,
171.985484999752));
#24690=CARTESIAN_POINT('Ctrl Pts',(-58.9766583348819,-112.755219171892,
171.985485069079));
#24691=CARTESIAN_POINT('Ctrl Pts',(-60.6142389590518,-112.486360908295,
171.985485138407));
#24692=CARTESIAN_POINT('Ctrl Pts',(-61.7692724831595,-112.268945389411,
173.157058062683));
#24693=CARTESIAN_POINT('Ctrl Pts',(-62.9243060072673,-112.051529870527,
174.328630986959));
#24694=CARTESIAN_POINT('Ctrl Pts',(-62.9143678754131,-111.95830811322,175.985485236451));
#24695=CARTESIAN_POINT('Ctrl Pts',(-62.9044297435589,-111.865086355914,
177.642339485944));
#24696=CARTESIAN_POINT('Ctrl Pts',(-61.7295199961253,-111.896058355881,
178.813912312176));
#24697=CARTESIAN_POINT('Ctrl Pts',(-60.5546102486917,-111.927030355848,
179.985485138407));
#24698=CARTESIAN_POINT('Ctrl Pts',(-58.8971534986878,-112.009445090134,
179.985485069079));
#24699=CARTESIAN_POINT('Ctrl Pts',(-57.2396967486839,-112.09185982442,179.985484999752));
#24700=CARTESIAN_POINT('Ctrl Pts',(-56.0647870987421,-112.122831813994,
178.813912075476));
#24701=CARTESIAN_POINT('Ctrl Pts',(-54.8898774488003,-112.153803803567,
177.6423391512));
#24702=CARTESIAN_POINT('Ctrl Pts',(-54.8799394548205,-112.060582031563,
175.985484901707));
#24703=CARTESIAN_POINT('Ctrl Pts',(-54.8700014608406,-111.967360259558,
174.328630652215));
#24704=CARTESIAN_POINT('Ctrl Pts',(-56.0250350824402,-111.749944730281,
173.157057825983));
#24705=CARTESIAN_POINT('Ctrl Pts',(-57.1800687040398,-111.532529201003,
171.985484999752));
#24706=CARTESIAN_POINT('Ctrl Pts',(-58.8176493282097,-111.263670937406,
171.985485069079));
#24707=CARTESIAN_POINT('Ctrl Pts',(-60.4552299523796,-110.994812673809,
171.985485138407));
#24708=CARTESIAN_POINT('Ctrl Pts',(-61.6102634764873,-110.777397154925,
173.157058062683));
#24709=CARTESIAN_POINT('Ctrl Pts',(-62.7652970005951,-110.559981636041,
174.328630986959));
#24710=CARTESIAN_POINT('Ctrl Pts',(-62.7553588687409,-110.466759878735,
175.985485236451));
#24711=CARTESIAN_POINT('Ctrl Pts',(-62.7454207368867,-110.373538121429,
177.642339485944));
#24712=CARTESIAN_POINT('Ctrl Pts',(-61.5705109894531,-110.404510121395,
178.813912312176));
#24713=CARTESIAN_POINT('Ctrl Pts',(-60.3956012420194,-110.435482121362,
179.985485138407));
#24714=CARTESIAN_POINT('Ctrl Pts',(-58.7381444920155,-110.517896855648,
179.985485069079));
#24715=CARTESIAN_POINT('Ctrl Pts',(-57.0806877420116,-110.600311589935,
179.985484999752));
#24716=CARTESIAN_POINT('Ctrl Pts',(-55.9057780920699,-110.631283579508,
178.813912075476));
#24717=CARTESIAN_POINT('Ctrl Pts',(-54.7308684421281,-110.662255569082,
177.6423391512));
#24718=CARTESIAN_POINT('Ctrl Pts',(-54.7209304481482,-110.569033797077,
175.985484901707));
#24719=CARTESIAN_POINT('Ctrl Pts',(-54.7109924541684,-110.475812025073,
174.328630652215));
#24720=CARTESIAN_POINT('Ctrl Pts',(-55.866026075768,-110.258396495795,173.157057825983));
#24721=CARTESIAN_POINT('Ctrl Pts',(-57.0210596973676,-110.040980966518,
171.985484999752));
#24722=CARTESIAN_POINT('Ctrl Pts',(-58.6586403215375,-109.772122702921,
171.985485069079));
#24723=CARTESIAN_POINT('Ctrl Pts',(-60.2962209457073,-109.503264439324,
171.985485138407));
#24724=CARTESIAN_POINT('Ctrl Pts',(-61.4512544698151,-109.28584892044,173.157058062683));
#24725=CARTESIAN_POINT('Ctrl Pts',(-62.6062879939228,-109.068433401555,
174.328630986959));
#24726=CARTESIAN_POINT('Ctrl Pts',(-62.5963498620687,-108.975211644249,
175.985485236451));
#24727=CARTESIAN_POINT('Ctrl Pts',(-62.5864117302145,-108.881989886943,
177.642339485944));
#24728=CARTESIAN_POINT('Ctrl Pts',(-61.4115019827808,-108.91296188691,178.813912312176));
#24729=CARTESIAN_POINT('Ctrl Pts',(-60.2365922353472,-108.943933886877,
179.985485138407));
#24730=CARTESIAN_POINT('Ctrl Pts',(-58.5791354853433,-109.026348621163,
179.985485069079));
#24731=CARTESIAN_POINT('Ctrl Pts',(-56.9216787353394,-109.108763355449,
179.985484999752));
#24732=CARTESIAN_POINT('Ctrl Pts',(-55.7467690853976,-109.139735345023,
178.813912075476));
#24733=CARTESIAN_POINT('Ctrl Pts',(-54.5718594354559,-109.170707334596,
177.6423391512));
#24734=CARTESIAN_POINT('Ctrl Pts',(-54.561921441476,-109.077485562592,175.985484901707));
#24735=CARTESIAN_POINT('Ctrl Pts',(-54.5519834474962,-108.984263790587,
174.328630652215));
#24736=CARTESIAN_POINT('Ctrl Pts',(-55.7070170690958,-108.76684826131,173.157057825983));
#24737=CARTESIAN_POINT('Ctrl Pts',(-56.8620506906954,-108.549432732032,
171.985484999752));
#24738=CARTESIAN_POINT('Ctrl Pts',(-58.4996313148652,-108.280574468435,
171.985485069079));
#24739=CARTESIAN_POINT('Ctrl Pts',(-60.1372119390351,-108.011716204838,
171.985485138407));
#24740=CARTESIAN_POINT('Ctrl Pts',(-61.2922454631428,-107.794300685954,
173.157058062683));
#24741=CARTESIAN_POINT('Ctrl Pts',(-62.4472789872506,-107.57688516707,174.328630986959));
#24742=CARTESIAN_POINT('Ctrl Pts',(-62.4373408553964,-107.483663409764,
175.985485236451));
#24743=CARTESIAN_POINT('Ctrl Pts',(-62.4274027235423,-107.390441652457,
177.642339485944));
#24744=CARTESIAN_POINT('Ctrl Pts',(-61.2524929761086,-107.421413652424,
178.813912312176));
#24745=CARTESIAN_POINT('Ctrl Pts',(-60.077583228675,-107.452385652391,179.985485138407));
#24746=CARTESIAN_POINT('Ctrl Pts',(-58.4201264786711,-107.534800386677,
179.985485069079));
#24747=CARTESIAN_POINT('Ctrl Pts',(-56.7626697286672,-107.617215120964,
179.985484999752));
#24748=CARTESIAN_POINT('Ctrl Pts',(-55.5877600787254,-107.648187110537,
178.813912075476));
#24749=CARTESIAN_POINT('Ctrl Pts',(-54.4128504287836,-107.67915910011,177.6423391512));
#24750=CARTESIAN_POINT('Ctrl Pts',(-54.4029124348038,-107.585937328106,
175.985484901707));
#24751=CARTESIAN_POINT('Ctrl Pts',(-54.3929744408239,-107.492715556102,
174.328630652215));
#24752=CARTESIAN_POINT('Ctrl Pts',(-55.5480080624235,-107.275300026824,
173.157057825983));
#24753=CARTESIAN_POINT('Ctrl Pts',(-56.7030416840231,-107.057884497547,
171.985484999752));
#24754=CARTESIAN_POINT('Ctrl Pts',(-58.340622308193,-106.78902623395,171.985485069079));
#24755=CARTESIAN_POINT('Ctrl Pts',(-59.9782029323629,-106.520167970353,
171.985485138407));
#24756=CARTESIAN_POINT('Ctrl Pts',(-61.1332364564706,-106.302752451468,
173.157058062683));
#24757=CARTESIAN_POINT('Ctrl Pts',(-62.2882699805784,-106.085336932584,
174.328630986959));
#24758=CARTESIAN_POINT('Ctrl Pts',(-62.2783318487242,-105.992115175278,
175.985485236451));
#24759=CARTESIAN_POINT('Ctrl Pts',(-62.26839371687,-105.898893417972,177.642339485944));
#24760=CARTESIAN_POINT('Ctrl Pts',(-61.0934839694364,-105.929865417939,
178.813912312176));
#24761=CARTESIAN_POINT('Ctrl Pts',(-59.9185742220028,-105.960837417905,
179.985485138407));
#24762=CARTESIAN_POINT('Ctrl Pts',(-58.2611174719989,-106.043252152192,
179.985485069079));
#24763=CARTESIAN_POINT('Ctrl Pts',(-56.603660721995,-106.125666886478,179.985484999752));
#24764=CARTESIAN_POINT('Ctrl Pts',(-55.4287510720532,-106.156638876051,
178.813912075476));
#24765=CARTESIAN_POINT('Ctrl Pts',(-54.2538414221114,-106.187610865625,
177.6423391512));
#24766=CARTESIAN_POINT('Ctrl Pts',(-54.2439034281315,-106.09438909362,175.985484901707));
#24767=CARTESIAN_POINT('Ctrl Pts',(-54.2339654341517,-106.001167321616,
174.328630652215));
#24768=CARTESIAN_POINT('Ctrl Pts',(-55.3889990557513,-105.783751792338,
173.157057825983));
#24769=CARTESIAN_POINT('Ctrl Pts',(-56.5440326773509,-105.566336263061,
171.985484999752));
#24770=CARTESIAN_POINT('Ctrl Pts',(-58.1816133015208,-105.297477999464,
171.985485069079));
#24771=CARTESIAN_POINT('Ctrl Pts',(-59.8191939256906,-105.028619735867,
171.985485138407));
#24772=CARTESIAN_POINT('Ctrl Pts',(-60.9742274497984,-104.811204216983,
173.157058062683));
#24773=CARTESIAN_POINT('Ctrl Pts',(-62.1292609739061,-104.593788698099,
174.328630986959));
#24774=CARTESIAN_POINT('Ctrl Pts',(-62.119322842052,-104.500566940792,175.985485236451));
#24775=CARTESIAN_POINT('Ctrl Pts',(-62.1093847101978,-104.407345183486,
177.642339485944));
#24776=CARTESIAN_POINT('Ctrl Pts',(-60.9344749627642,-104.438317183453,
178.813912312176));
#24777=CARTESIAN_POINT('Ctrl Pts',(-59.7595652153305,-104.46928918342,179.985485138407));
#24778=CARTESIAN_POINT('Ctrl Pts',(-58.1021084653266,-104.551703917706,
179.985485069079));
#24779=CARTESIAN_POINT('Ctrl Pts',(-56.4446517153227,-104.634118651992,
179.985484999752));
#24780=CARTESIAN_POINT('Ctrl Pts',(-55.269742065381,-104.665090641566,178.813912075476));
#24781=CARTESIAN_POINT('Ctrl Pts',(-54.0948324154392,-104.696062631139,
177.6423391512));
#24782=CARTESIAN_POINT('Ctrl Pts',(-54.0848944214593,-104.602840859135,
175.985484901707));
#24783=CARTESIAN_POINT('Ctrl Pts',(-54.0749564274795,-104.50961908713,174.328630652215));
#24784=CARTESIAN_POINT('Ctrl Pts',(-55.2299900490791,-104.292203557853,
173.157057825983));
#24785=CARTESIAN_POINT('Ctrl Pts',(-56.3850236706787,-104.074788028575,
171.985484999752));
#24786=CARTESIAN_POINT('Ctrl Pts',(-58.0226042948486,-103.805929764978,
171.985485069079));
#24787=CARTESIAN_POINT('Ctrl Pts',(-59.6601849190184,-103.537071501381,
171.985485138407));
#24788=CARTESIAN_POINT('Ctrl Pts',(-60.8152184431262,-103.319655982497,
173.157058062683));
#24789=CARTESIAN_POINT('Ctrl Pts',(-61.9702519672339,-103.102240463613,
174.328630986959));
#24790=CARTESIAN_POINT('Ctrl Pts',(-61.9603138353797,-103.009018706307,
175.985485236451));
#24791=CARTESIAN_POINT('Ctrl Pts',(-61.9503757035256,-102.915796949001,
177.642339485944));
#24792=CARTESIAN_POINT('Ctrl Pts',(-60.7754659560919,-102.946768948967,
178.813912312176));
#24793=CARTESIAN_POINT('Ctrl Pts',(-59.6005562086583,-102.977740948934,
179.985485138407));
#24794=CARTESIAN_POINT('Ctrl Pts',(-57.9430994586544,-103.06015568322,179.985485069079));
#24795=CARTESIAN_POINT('Ctrl Pts',(-56.2856427086505,-103.142570417507,
179.985484999752));
#24796=CARTESIAN_POINT('Ctrl Pts',(-55.1107330587087,-103.17354240708,178.813912075476));
#24797=CARTESIAN_POINT('Ctrl Pts',(-53.935823408767,-103.204514396654,177.6423391512));
#24798=CARTESIAN_POINT('Ctrl Pts',(-53.9258854147871,-103.111292624649,
175.985484901707));
#24799=CARTESIAN_POINT('Ctrl Pts',(-53.9159474208072,-103.018070852645,
174.328630652215));
#24800=CARTESIAN_POINT('Ctrl Pts',(-55.0709810424069,-102.800655323367,
173.157057825983));
#24801=CARTESIAN_POINT('Ctrl Pts',(-56.2260146640065,-102.58323979409,171.985484999752));
#24802=CARTESIAN_POINT('Ctrl Pts',(-57.8635952881763,-102.314381530493,
171.985485069079));
#24803=CARTESIAN_POINT('Ctrl Pts',(-59.5011759123462,-102.045523266896,
171.985485138407));
#24804=CARTESIAN_POINT('Ctrl Pts',(-60.6562094364539,-101.828107748012,
173.157058062683));
#24805=CARTESIAN_POINT('Ctrl Pts',(-61.8112429605617,-101.610692229127,
174.328630986959));
#24806=CARTESIAN_POINT('Ctrl Pts',(-61.8013048287075,-101.517470471821,
175.985485236451));
#24807=CARTESIAN_POINT('Ctrl Pts',(-61.7913666968533,-101.424248714515,
177.642339485944));
#24808=CARTESIAN_POINT('Ctrl Pts',(-60.6164569494197,-101.455220714482,
178.813912312176));
#24809=CARTESIAN_POINT('Ctrl Pts',(-59.4415472019861,-101.486192714449,
179.985485138407));
#24810=CARTESIAN_POINT('Ctrl Pts',(-57.7840904519822,-101.568607448735,
179.985485069079));
#24811=CARTESIAN_POINT('Ctrl Pts',(-56.1266337019783,-101.651022183021,
179.985484999752));
#24812=CARTESIAN_POINT('Ctrl Pts',(-54.9517240520365,-101.681994172595,
178.813912075476));
#24813=CARTESIAN_POINT('Ctrl Pts',(-53.7768144020947,-101.712966162168,
177.6423391512));
#24814=CARTESIAN_POINT('Ctrl Pts',(-53.7668764081149,-101.619744390164,
175.985484901707));
#24815=CARTESIAN_POINT('Ctrl Pts',(-53.756938414135,-101.526522618159,174.328630652215));
#24816=CARTESIAN_POINT('Ctrl Pts',(-54.9119720357346,-101.309107088882,
173.157057825983));
#24817=CARTESIAN_POINT('Ctrl Pts',(-56.0670056573342,-101.091691559604,
171.985484999752));
#24818=CARTESIAN_POINT('Ctrl Pts',(-57.7045862815041,-100.822833296007,
171.985485069079));
#24819=CARTESIAN_POINT('Ctrl Pts',(-59.342166905674,-100.55397503241,171.985485138407));
#24820=CARTESIAN_POINT('Ctrl Pts',(-60.4972004297817,-100.336559513526,
173.157058062683));
#24821=CARTESIAN_POINT('Ctrl Pts',(-61.6522339538895,-100.119143994642,
174.328630986959));
#24822=CARTESIAN_POINT('Ctrl Pts',(-61.6422958220353,-100.025922237336,
175.985485236451));
#24823=CARTESIAN_POINT('Ctrl Pts',(-61.6323576901811,-99.9327004800294,
177.642339485944));
#24824=CARTESIAN_POINT('Ctrl Pts',(-60.4574479427475,-99.9636724799962,
178.813912312176));
#24825=CARTESIAN_POINT('Ctrl Pts',(-59.2825381953138,-99.994644479963,179.985485138407));
#24826=CARTESIAN_POINT('Ctrl Pts',(-57.6250814453099,-100.077059214249,
179.985485069079));
#24827=CARTESIAN_POINT('Ctrl Pts',(-55.9676246953061,-100.159473948536,
179.985484999752));
#24828=CARTESIAN_POINT('Ctrl Pts',(-54.7927150453643,-100.190445938109,
178.813912075476));
#24829=CARTESIAN_POINT('Ctrl Pts',(-53.6178053954225,-100.221417927683,
177.6423391512));
#24830=CARTESIAN_POINT('Ctrl Pts',(-53.6078674014426,-100.128196155678,
175.985484901707));
#24831=CARTESIAN_POINT('Ctrl Pts',(-53.5979294074628,-100.034974383673,
174.328630652215));
#24832=CARTESIAN_POINT('Ctrl Pts',(-54.7529630290624,-99.817558854396,173.157057825983));
#24833=CARTESIAN_POINT('Ctrl Pts',(-55.907996650662,-99.6001433251185,171.985484999752));
#24834=CARTESIAN_POINT('Ctrl Pts',(-57.5455772748319,-99.3312850615215,
171.985485069079));
#24835=CARTESIAN_POINT('Ctrl Pts',(-59.1831578990017,-99.0624267979246,
171.985485138407));
#24836=CARTESIAN_POINT('Ctrl Pts',(-60.3381914231095,-98.8450112790404,
173.157058062683));
#24837=CARTESIAN_POINT('Ctrl Pts',(-61.4932249472172,-98.6275957601562,
174.328630986959));
#24838=CARTESIAN_POINT('Ctrl Pts',(-61.4832868153631,-98.53437400285,175.985485236451));
#24839=CARTESIAN_POINT('Ctrl Pts',(-61.4733486835089,-98.4411522455438,
177.642339485944));
#24840=CARTESIAN_POINT('Ctrl Pts',(-60.2984389360752,-98.4721242455106,
178.813912312176));
#24841=CARTESIAN_POINT('Ctrl Pts',(-59.1235291886416,-98.5030962454774,
179.985485138407));
#24842=CARTESIAN_POINT('Ctrl Pts',(-57.4660724386377,-98.5855109797636,
179.985485069079));
#24843=CARTESIAN_POINT('Ctrl Pts',(-55.8086156886338,-98.6679257140499,
179.985484999752));
#24844=CARTESIAN_POINT('Ctrl Pts',(-54.633706038692,-98.6988977036234,178.813912075476));
#24845=CARTESIAN_POINT('Ctrl Pts',(-56.9964983346804,-113.864655531781,
178.072094410988));
#24846=CARTESIAN_POINT('Ctrl Pts',(-56.1271283009022,-113.863054956993,
177.207792449865));
#24847=CARTESIAN_POINT('Ctrl Pts',(-56.117190288842,-113.769833186916,175.985484945604));
#24848=CARTESIAN_POINT('Ctrl Pts',(-56.1072522767819,-113.676611416839,
174.763177441344));
#24849=CARTESIAN_POINT('Ctrl Pts',(-56.9567462566485,-113.491768454648,
173.89887555255));
#24850=CARTESIAN_POINT('Ctrl Pts',(-57.8062402365152,-113.306925492458,
173.034573663757));
#24851=CARTESIAN_POINT('Ctrl Pts',(-59.011722573584,-113.084131793069,173.034573714903));
#24852=CARTESIAN_POINT('Ctrl Pts',(-60.2172049106529,-112.86133809368,173.034573766048));
#24853=CARTESIAN_POINT('Ctrl Pts',(-61.0666988185971,-112.676495139156,
173.898875727171));
#24854=CARTESIAN_POINT('Ctrl Pts',(-61.9161927265413,-112.491652184633,
174.763177688294));
#24855=CARTESIAN_POINT('Ctrl Pts',(-61.9062546127674,-112.398430425399,
175.985485192554));
#24856=CARTESIAN_POINT('Ctrl Pts',(-61.8963164989935,-112.305208666166,
177.207792696815));
#24857=CARTESIAN_POINT('Ctrl Pts',(-61.0269463932928,-112.303608099046,
178.072094585608));
#24858=CARTESIAN_POINT('Ctrl Pts',(-60.1575762875921,-112.302007531926,
178.936396474401));
#24859=CARTESIAN_POINT('Ctrl Pts',(-58.9322178246893,-112.338357702004,
178.936396423256));
#24860=CARTESIAN_POINT('Ctrl Pts',(-57.7068593617864,-112.374707872082,
178.936396372111));
#24861=CARTESIAN_POINT('Ctrl Pts',(-56.8374893280082,-112.373107297295,
178.072094410988));
#24862=CARTESIAN_POINT('Ctrl Pts',(-55.9681192942299,-112.371506722508,
177.207792449865));
#24863=CARTESIAN_POINT('Ctrl Pts',(-55.9581812821698,-112.278284952431,
175.985484945604));
#24864=CARTESIAN_POINT('Ctrl Pts',(-55.9482432701096,-112.185063182354,
174.763177441344));
#24865=CARTESIAN_POINT('Ctrl Pts',(-56.7977372499763,-112.000220220163,
173.89887555255));
#24866=CARTESIAN_POINT('Ctrl Pts',(-57.647231229843,-111.815377257972,173.034573663757));
#24867=CARTESIAN_POINT('Ctrl Pts',(-58.8527135669118,-111.592583558583,
173.034573714903));
#24868=CARTESIAN_POINT('Ctrl Pts',(-60.0581959039807,-111.369789859194,
173.034573766048));
#24869=CARTESIAN_POINT('Ctrl Pts',(-60.9076898119249,-111.184946904671,
173.898875727171));
#24870=CARTESIAN_POINT('Ctrl Pts',(-61.7571837198691,-111.000103950148,
174.763177688294));
#24871=CARTESIAN_POINT('Ctrl Pts',(-61.7472456060952,-110.906882190914,
175.985485192554));
#24872=CARTESIAN_POINT('Ctrl Pts',(-61.7373074923213,-110.81366043168,177.207792696815));
#24873=CARTESIAN_POINT('Ctrl Pts',(-60.8679373866206,-110.81205986456,178.072094585608));
#24874=CARTESIAN_POINT('Ctrl Pts',(-59.9985672809199,-110.81045929744,178.936396474401));
#24875=CARTESIAN_POINT('Ctrl Pts',(-58.7732088180171,-110.846809467519,
178.936396423256));
#24876=CARTESIAN_POINT('Ctrl Pts',(-57.5478503551142,-110.883159637597,
178.936396372111));
#24877=CARTESIAN_POINT('Ctrl Pts',(-56.6784803213359,-110.881559062809,
178.072094410988));
#24878=CARTESIAN_POINT('Ctrl Pts',(-55.8091102875577,-110.879958488022,
177.207792449865));
#24879=CARTESIAN_POINT('Ctrl Pts',(-55.7991722754976,-110.786736717945,
175.985484945604));
#24880=CARTESIAN_POINT('Ctrl Pts',(-55.7892342634374,-110.693514947868,
174.763177441344));
#24881=CARTESIAN_POINT('Ctrl Pts',(-56.6387282433041,-110.508671985677,
173.89887555255));
#24882=CARTESIAN_POINT('Ctrl Pts',(-57.4882222231708,-110.323829023487,
173.034573663757));
#24883=CARTESIAN_POINT('Ctrl Pts',(-58.6937045602396,-110.101035324098,
173.034573714903));
#24884=CARTESIAN_POINT('Ctrl Pts',(-59.8991868973084,-109.878241624709,
173.034573766048));
#24885=CARTESIAN_POINT('Ctrl Pts',(-60.7486808052526,-109.693398670185,
173.898875727171));
#24886=CARTESIAN_POINT('Ctrl Pts',(-61.5981747131968,-109.508555715662,
174.763177688294));
#24887=CARTESIAN_POINT('Ctrl Pts',(-61.588236599423,-109.415333956428,175.985485192554));
#24888=CARTESIAN_POINT('Ctrl Pts',(-61.5782984856491,-109.322112197195,
177.207792696815));
#24889=CARTESIAN_POINT('Ctrl Pts',(-60.7089283799484,-109.320511630075,
178.072094585608));
#24890=CARTESIAN_POINT('Ctrl Pts',(-59.8395582742477,-109.318911062955,
178.936396474401));
#24891=CARTESIAN_POINT('Ctrl Pts',(-58.6141998113448,-109.355261233033,
178.936396423256));
#24892=CARTESIAN_POINT('Ctrl Pts',(-57.388841348442,-109.391611403111,178.936396372111));
#24893=CARTESIAN_POINT('Ctrl Pts',(-56.5194713146637,-109.390010828324,
178.072094410988));
#24894=CARTESIAN_POINT('Ctrl Pts',(-55.6501012808855,-109.388410253536,
177.207792449865));
#24895=CARTESIAN_POINT('Ctrl Pts',(-55.6401632688253,-109.295188483459,
175.985484945604));
#24896=CARTESIAN_POINT('Ctrl Pts',(-55.6302252567652,-109.201966713382,
174.763177441344));
#24897=CARTESIAN_POINT('Ctrl Pts',(-56.4797192366319,-109.017123751192,
173.89887555255));
#24898=CARTESIAN_POINT('Ctrl Pts',(-57.3292132164985,-108.832280789001,
173.034573663757));
#24899=CARTESIAN_POINT('Ctrl Pts',(-58.5346955535674,-108.609487089612,
173.034573714903));
#24900=CARTESIAN_POINT('Ctrl Pts',(-59.7401778906362,-108.386693390223,
173.034573766048));
#24901=CARTESIAN_POINT('Ctrl Pts',(-60.5896717985804,-108.2018504357,173.898875727171));
#24902=CARTESIAN_POINT('Ctrl Pts',(-61.4391657065246,-108.017007481176,
174.763177688294));
#24903=CARTESIAN_POINT('Ctrl Pts',(-61.4292275927507,-107.923785721943,
175.985485192554));
#24904=CARTESIAN_POINT('Ctrl Pts',(-61.4192894789769,-107.830563962709,
177.207792696815));
#24905=CARTESIAN_POINT('Ctrl Pts',(-60.5499193732762,-107.828963395589,
178.072094585608));
#24906=CARTESIAN_POINT('Ctrl Pts',(-59.6805492675755,-107.827362828469,
178.936396474401));
#24907=CARTESIAN_POINT('Ctrl Pts',(-58.4551908046726,-107.863712998547,
178.936396423256));
#24908=CARTESIAN_POINT('Ctrl Pts',(-57.2298323417698,-107.900063168626,
178.936396372111));
#24909=CARTESIAN_POINT('Ctrl Pts',(-56.3604623079915,-107.898462593838,
178.072094410988));
#24910=CARTESIAN_POINT('Ctrl Pts',(-55.4910922742133,-107.896862019051,
177.207792449865));
#24911=CARTESIAN_POINT('Ctrl Pts',(-55.4811542621531,-107.803640248974,
175.985484945604));
#24912=CARTESIAN_POINT('Ctrl Pts',(-55.471216250093,-107.710418478897,174.763177441344));
#24913=CARTESIAN_POINT('Ctrl Pts',(-56.3207102299596,-107.525575516706,
173.89887555255));
#24914=CARTESIAN_POINT('Ctrl Pts',(-57.1702042098263,-107.340732554515,
173.034573663757));
#24915=CARTESIAN_POINT('Ctrl Pts',(-58.3756865468951,-107.117938855126,
173.034573714903));
#24916=CARTESIAN_POINT('Ctrl Pts',(-59.581168883964,-106.895145155737,173.034573766048));
#24917=CARTESIAN_POINT('Ctrl Pts',(-60.4306627919082,-106.710302201214,
173.898875727171));
#24918=CARTESIAN_POINT('Ctrl Pts',(-61.2801566998524,-106.525459246691,
174.763177688294));
#24919=CARTESIAN_POINT('Ctrl Pts',(-61.2702185860785,-106.432237487457,
175.985485192554));
#24920=CARTESIAN_POINT('Ctrl Pts',(-61.2602804723046,-106.339015728223,
177.207792696815));
#24921=CARTESIAN_POINT('Ctrl Pts',(-60.3909103666039,-106.337415161103,
178.072094585608));
#24922=CARTESIAN_POINT('Ctrl Pts',(-59.5215402609032,-106.335814593983,
178.936396474401));
#24923=CARTESIAN_POINT('Ctrl Pts',(-58.2961817980004,-106.372164764062,
178.936396423256));
#24924=CARTESIAN_POINT('Ctrl Pts',(-57.0708233350975,-106.40851493414,178.936396372111));
#24925=CARTESIAN_POINT('Ctrl Pts',(-56.2014533013193,-106.406914359353,
178.072094410988));
#24926=CARTESIAN_POINT('Ctrl Pts',(-55.332083267541,-106.405313784565,177.207792449865));
#24927=CARTESIAN_POINT('Ctrl Pts',(-55.3221452554809,-106.312092014488,
175.985484945604));
#24928=CARTESIAN_POINT('Ctrl Pts',(-55.3122072434207,-106.218870244411,
174.763177441344));
#24929=CARTESIAN_POINT('Ctrl Pts',(-56.1617012232874,-106.034027282221,
173.89887555255));
#24930=CARTESIAN_POINT('Ctrl Pts',(-57.0111952031541,-105.84918432003,173.034573663757));
#24931=CARTESIAN_POINT('Ctrl Pts',(-58.2166775402229,-105.626390620641,
173.034573714903));
#24932=CARTESIAN_POINT('Ctrl Pts',(-59.4221598772917,-105.403596921252,
173.034573766048));
#24933=CARTESIAN_POINT('Ctrl Pts',(-60.2716537852359,-105.218753966728,
173.898875727171));
#24934=CARTESIAN_POINT('Ctrl Pts',(-61.1211476931802,-105.033911012205,
174.763177688294));
#24935=CARTESIAN_POINT('Ctrl Pts',(-61.1112095794063,-104.940689252971,
175.985485192554));
#24936=CARTESIAN_POINT('Ctrl Pts',(-61.1012714656324,-104.847467493738,
177.207792696815));
#24937=CARTESIAN_POINT('Ctrl Pts',(-60.2319013599317,-104.845866926618,
178.072094585608));
#24938=CARTESIAN_POINT('Ctrl Pts',(-59.362531254231,-104.844266359498,178.936396474401));
#24939=CARTESIAN_POINT('Ctrl Pts',(-58.1371727913281,-104.880616529576,
178.936396423256));
#24940=CARTESIAN_POINT('Ctrl Pts',(-56.9118143284253,-104.916966699654,
178.936396372111));
#24941=CARTESIAN_POINT('Ctrl Pts',(-56.042444294647,-104.915366124867,178.072094410988));
#24942=CARTESIAN_POINT('Ctrl Pts',(-55.1730742608688,-104.91376555008,177.207792449865));
#24943=CARTESIAN_POINT('Ctrl Pts',(-55.1631362488087,-104.820543780003,
175.985484945604));
#24944=CARTESIAN_POINT('Ctrl Pts',(-55.1531982367485,-104.727322009926,
174.763177441344));
#24945=CARTESIAN_POINT('Ctrl Pts',(-56.0026922166152,-104.542479047735,
173.89887555255));
#24946=CARTESIAN_POINT('Ctrl Pts',(-56.8521861964818,-104.357636085544,
173.034573663757));
#24947=CARTESIAN_POINT('Ctrl Pts',(-58.0576685335507,-104.134842386155,
173.034573714903));
#24948=CARTESIAN_POINT('Ctrl Pts',(-59.2631508706195,-103.912048686766,
173.034573766048));
#24949=CARTESIAN_POINT('Ctrl Pts',(-60.1126447785637,-103.727205732243,
173.898875727171));
#24950=CARTESIAN_POINT('Ctrl Pts',(-60.9621386865079,-103.54236277772,174.763177688294));
#24951=CARTESIAN_POINT('Ctrl Pts',(-60.952200572734,-103.449141018486,175.985485192554));
#24952=CARTESIAN_POINT('Ctrl Pts',(-60.9422624589602,-103.355919259252,
177.207792696815));
#24953=CARTESIAN_POINT('Ctrl Pts',(-60.0728923532595,-103.354318692132,
178.072094585608));
#24954=CARTESIAN_POINT('Ctrl Pts',(-59.2035222475588,-103.352718125012,
178.936396474401));
#24955=CARTESIAN_POINT('Ctrl Pts',(-57.9781637846559,-103.389068295091,
178.936396423256));
#24956=CARTESIAN_POINT('Ctrl Pts',(-56.7528053217531,-103.425418465169,
178.936396372111));
#24957=CARTESIAN_POINT('Ctrl Pts',(-55.8834352879748,-103.423817890381,
178.072094410988));
#24958=CARTESIAN_POINT('Ctrl Pts',(-55.0140652541966,-103.422217315594,
177.207792449865));
#24959=CARTESIAN_POINT('Ctrl Pts',(-55.0041272421364,-103.328995545517,
175.985484945604));
#24960=CARTESIAN_POINT('Ctrl Pts',(-54.9941892300763,-103.23577377544,174.763177441344));
#24961=CARTESIAN_POINT('Ctrl Pts',(-55.8436832099429,-103.050930813249,
173.89887555255));
#24962=CARTESIAN_POINT('Ctrl Pts',(-56.6931771898096,-102.866087851059,
173.034573663757));
#24963=CARTESIAN_POINT('Ctrl Pts',(-57.8986595268784,-102.64329415167,173.034573714903));
#24964=CARTESIAN_POINT('Ctrl Pts',(-59.1041418639473,-102.420500452281,
173.034573766048));
#24965=CARTESIAN_POINT('Ctrl Pts',(-59.9536357718915,-102.235657497757,
173.898875727171));
#24966=CARTESIAN_POINT('Ctrl Pts',(-60.8031296798357,-102.050814543234,
174.763177688294));
#24967=CARTESIAN_POINT('Ctrl Pts',(-60.7931915660618,-101.957592784,175.985485192554));
#24968=CARTESIAN_POINT('Ctrl Pts',(-60.783253452288,-101.864371024767,177.207792696815));
#24969=CARTESIAN_POINT('Ctrl Pts',(-59.9138833465873,-101.862770457647,
178.072094585608));
#24970=CARTESIAN_POINT('Ctrl Pts',(-59.0445132408866,-101.861169890527,
178.936396474401));
#24971=CARTESIAN_POINT('Ctrl Pts',(-57.8191547779837,-101.897520060605,
178.936396423256));
#24972=CARTESIAN_POINT('Ctrl Pts',(-56.5937963150808,-101.933870230683,
178.936396372111));
#24973=CARTESIAN_POINT('Ctrl Pts',(-55.7244262813026,-101.932269655896,
178.072094410988));
#24974=CARTESIAN_POINT('Ctrl Pts',(-54.8550562475244,-101.930669081108,
177.207792449865));
#24975=CARTESIAN_POINT('Ctrl Pts',(-54.8451182354642,-101.837447311031,
175.985484945604));
#24976=CARTESIAN_POINT('Ctrl Pts',(-54.8351802234041,-101.744225540954,
174.763177441344));
#24977=CARTESIAN_POINT('Ctrl Pts',(-55.6846742032707,-101.559382578764,
173.89887555255));
#24978=CARTESIAN_POINT('Ctrl Pts',(-56.5341681831374,-101.374539616573,
173.034573663757));
#24979=CARTESIAN_POINT('Ctrl Pts',(-57.7396505202062,-101.151745917184,
173.034573714903));
#24980=CARTESIAN_POINT('Ctrl Pts',(-58.9451328572751,-100.928952217795,
173.034573766048));
#24981=CARTESIAN_POINT('Ctrl Pts',(-59.7946267652193,-100.744109263272,
173.898875727171));
#24982=CARTESIAN_POINT('Ctrl Pts',(-60.6441206731635,-100.559266308748,
174.763177688294));
#24983=CARTESIAN_POINT('Ctrl Pts',(-60.6341825593896,-100.466044549515,
175.985485192554));
#24984=CARTESIAN_POINT('Ctrl Pts',(-60.6242444456157,-100.372822790281,
177.207792696815));
#24985=CARTESIAN_POINT('Ctrl Pts',(-59.754874339915,-100.371222223161,178.072094585608));
#24986=CARTESIAN_POINT('Ctrl Pts',(-58.8855042342143,-100.369621656041,
178.936396474401));
#24987=CARTESIAN_POINT('Ctrl Pts',(-57.6601457713115,-100.405971826119,
178.936396423256));
#24988=CARTESIAN_POINT('Ctrl Pts',(-56.4347873084086,-100.442321996198,
178.936396372111));
#24989=CARTESIAN_POINT('Ctrl Pts',(-55.5654172746304,-100.44072142141,178.072094410988));
#24990=CARTESIAN_POINT('Ctrl Pts',(-54.6960472408521,-100.439120846623,
177.207792449865));
#24991=CARTESIAN_POINT('Ctrl Pts',(-54.686109228792,-100.345899076546,175.985484945604));
#24992=CARTESIAN_POINT('Ctrl Pts',(-54.6761712167318,-100.252677306469,
174.763177441344));
#24993=CARTESIAN_POINT('Ctrl Pts',(-55.5256651965985,-100.067834344278,
173.89887555255));
#24994=CARTESIAN_POINT('Ctrl Pts',(-56.3751591764652,-99.8829913820874,
173.034573663757));
#24995=CARTESIAN_POINT('Ctrl Pts',(-57.580641513534,-99.6601976826983,173.034573714903));
#24996=CARTESIAN_POINT('Ctrl Pts',(-58.7861238506028,-99.4374039833093,
173.034573766048));
#24997=CARTESIAN_POINT('Ctrl Pts',(-59.635617758547,-99.252561028786,173.898875727171));
#24998=CARTESIAN_POINT('Ctrl Pts',(-60.4851116664912,-99.0677180742627,
174.763177688294));
#24999=CARTESIAN_POINT('Ctrl Pts',(-60.4751735527174,-98.9744963150291,
175.985485192554));
#25000=CARTESIAN_POINT('Ctrl Pts',(-60.4652354389435,-98.8812745557954,
177.207792696815));
#25001=CARTESIAN_POINT('Ctrl Pts',(-59.5958653332428,-98.8796739886754,
178.072094585608));
#25002=CARTESIAN_POINT('Ctrl Pts',(-58.7264952275421,-98.8780734215554,
178.936396474401));
#25003=CARTESIAN_POINT('Ctrl Pts',(-57.5011367646392,-98.9144235916337,
178.936396423256));
#25004=CARTESIAN_POINT('Ctrl Pts',(-56.2757783017364,-98.9507737617121,
178.936396372111));
#25005=CARTESIAN_POINT('Ctrl Pts',(-55.4064082679581,-98.9491731869247,
178.072094410988));
#25006=CARTESIAN_POINT('Ctrl Pts',(-61.8656266134859,-110.398668935236,
178.485485069079));
#25007=CARTESIAN_POINT('Ctrl Pts',(-61.7270544091292,-110.400383453113,
178.657813499464));
#25008=CARTESIAN_POINT('Ctrl Pts',(-61.5705109894531,-110.404510121395,
178.813912312176));
#25009=CARTESIAN_POINT('Ctrl Pts',(-60.3956012420194,-110.435482121362,
179.985485138407));
#25010=CARTESIAN_POINT('Ctrl Pts',(-58.7381444920155,-110.517896855648,
179.985485069079));
#25011=CARTESIAN_POINT('Ctrl Pts',(-57.0806877420117,-110.600311589935,
179.985484999752));
#25012=CARTESIAN_POINT('Ctrl Pts',(-55.9057780920699,-110.631283579508,
178.813912075476));
#25013=CARTESIAN_POINT('Ctrl Pts',(-54.7308684421281,-110.662255569082,
177.6423391512));
#25014=CARTESIAN_POINT('Ctrl Pts',(-54.7209304481482,-110.569033797077,
175.985484901707));
#25015=CARTESIAN_POINT('Ctrl Pts',(-54.7109924541684,-110.475812025073,
174.328630652215));
#25016=CARTESIAN_POINT('Ctrl Pts',(-55.866026075768,-110.258396495795,173.157057825983));
#25017=CARTESIAN_POINT('Ctrl Pts',(-57.0210596973676,-110.040980966518,
171.985484999752));
#25018=CARTESIAN_POINT('Ctrl Pts',(-58.6586403215375,-109.772122702921,
171.985485069079));
#25019=CARTESIAN_POINT('Ctrl Pts',(-60.2962209457073,-109.503264439324,
171.985485138407));
#25020=CARTESIAN_POINT('Ctrl Pts',(-61.4512544698151,-109.28584892044,173.157058062683));
#25021=CARTESIAN_POINT('Ctrl Pts',(-61.6051494907682,-109.256880786497,
173.313156769748));
#25022=CARTESIAN_POINT('Ctrl Pts',(-61.740968694739,-109.229343357315,173.485485069079));
#25023=CARTESIAN_POINT('Ctrl Pts',(-56.8733667677527,-112.709647553905,
178.072094410988));
#25024=CARTESIAN_POINT('Ctrl Pts',(-56.0039967339745,-112.708046979118,
177.207792449865));
#25025=CARTESIAN_POINT('Ctrl Pts',(-55.9940587219143,-112.614825209041,
175.985484945604));
#25026=CARTESIAN_POINT('Ctrl Pts',(-55.9841207098542,-112.521603438964,
174.763177441344));
#25027=CARTESIAN_POINT('Ctrl Pts',(-56.8336146897208,-112.336760476773,
173.89887555255));
#25028=CARTESIAN_POINT('Ctrl Pts',(-57.6831086695875,-112.151917514582,
173.034573663757));
#25029=CARTESIAN_POINT('Ctrl Pts',(-58.8885910066563,-111.929123815193,
173.034573714903));
#25030=CARTESIAN_POINT('Ctrl Pts',(-60.0940733437252,-111.706330115804,
173.034573766048));
#25031=CARTESIAN_POINT('Ctrl Pts',(-60.9435672516694,-111.521487161281,
173.898875727171));
#25032=CARTESIAN_POINT('Ctrl Pts',(-61.7930611596136,-111.336644206758,
174.763177688294));
#25033=CARTESIAN_POINT('Ctrl Pts',(-61.7831230458397,-111.243422447524,
175.985485192554));
#25034=CARTESIAN_POINT('Ctrl Pts',(-61.7731849320658,-111.15020068829,177.207792696815));
#25035=CARTESIAN_POINT('Ctrl Pts',(-60.9038148263651,-111.14860012117,178.072094585608));
#25036=CARTESIAN_POINT('Ctrl Pts',(-60.0344447206644,-111.14699955405,178.936396474401));
#25037=CARTESIAN_POINT('Ctrl Pts',(-58.8090862577616,-111.183349724129,
178.936396423256));
#25038=CARTESIAN_POINT('Ctrl Pts',(-57.5837277948587,-111.219699894207,
178.936396372111));
#25039=CARTESIAN_POINT('Ctrl Pts',(-56.7143577610805,-111.21809931942,178.072094410988));
#25040=CARTESIAN_POINT('Ctrl Pts',(-55.8449877273022,-111.216498744632,
177.207792449865));
#25041=CARTESIAN_POINT('Ctrl Pts',(-55.8350497152421,-111.123276974555,
175.985484945604));
#25042=CARTESIAN_POINT('Ctrl Pts',(-55.8251117031819,-111.030055204478,
174.763177441344));
#25043=CARTESIAN_POINT('Ctrl Pts',(-56.6746056830486,-110.845212242287,
173.89887555255));
#25044=CARTESIAN_POINT('Ctrl Pts',(-57.5240996629153,-110.660369280097,
173.034573663757));
#25045=CARTESIAN_POINT('Ctrl Pts',(-58.7295819999841,-110.437575580708,
173.034573714903));
#25046=CARTESIAN_POINT('Ctrl Pts',(-59.9350643370529,-110.214781881319,
173.034573766048));
#25047=CARTESIAN_POINT('Ctrl Pts',(-60.7845582449971,-110.029938926795,
173.898875727171));
#25048=CARTESIAN_POINT('Ctrl Pts',(-61.6340521529414,-109.845095972272,
174.763177688294));
#25049=CARTESIAN_POINT('Ctrl Pts',(-61.6241140391675,-109.751874213038,
175.985485192554));
#25050=CARTESIAN_POINT('Ctrl Pts',(-61.6141759253936,-109.658652453805,
177.207792696815));
#25051=CARTESIAN_POINT('Ctrl Pts',(-60.7448058196929,-109.657051886685,
178.072094585608));
#25052=CARTESIAN_POINT('Ctrl Pts',(-59.8754357139922,-109.655451319565,
178.936396474401));
#25053=CARTESIAN_POINT('Ctrl Pts',(-58.6500772510893,-109.691801489643,
178.936396423256));
#25054=CARTESIAN_POINT('Ctrl Pts',(-57.4247187881865,-109.728151659721,
178.936396372111));
#25055=CARTESIAN_POINT('Ctrl Pts',(-56.5553487544082,-109.726551084934,
178.072094410988));
#25056=CARTESIAN_POINT('Ctrl Pts',(-55.68597872063,-109.724950510147,177.207792449865));
#25057=CARTESIAN_POINT('Ctrl Pts',(-55.6760407085698,-109.63172874007,175.985484945604));
#25058=CARTESIAN_POINT('Ctrl Pts',(-55.6661026965097,-109.538506969993,
174.763177441344));
#25059=CARTESIAN_POINT('Ctrl Pts',(-56.5155966763764,-109.353664007802,
173.89887555255));
#25060=CARTESIAN_POINT('Ctrl Pts',(-57.365090656243,-109.168821045611,173.034573663757));
#25061=CARTESIAN_POINT('Ctrl Pts',(-58.5705729933119,-108.946027346222,
173.034573714903));
#25062=CARTESIAN_POINT('Ctrl Pts',(-59.7760553303807,-108.723233646833,
173.034573766048));
#25063=CARTESIAN_POINT('Ctrl Pts',(-60.6255492383249,-108.53839069231,173.898875727171));
#25064=CARTESIAN_POINT('Ctrl Pts',(-61.4750431462691,-108.353547737786,
174.763177688294));
#25065=CARTESIAN_POINT('Ctrl Pts',(-61.4651050324952,-108.260325978553,
175.985485192554));
#25066=CARTESIAN_POINT('Ctrl Pts',(-61.4551669187214,-108.167104219319,
177.207792696815));
#25067=CARTESIAN_POINT('Ctrl Pts',(-60.5857968130207,-108.165503652199,
178.072094585608));
#25068=CARTESIAN_POINT('Ctrl Pts',(-59.71642670732,-108.163903085079,178.936396474401));
#25069=CARTESIAN_POINT('Ctrl Pts',(-58.4910682444171,-108.200253255158,
178.936396423256));
#25070=CARTESIAN_POINT('Ctrl Pts',(-57.2657097815143,-108.236603425236,
178.936396372111));
#25071=CARTESIAN_POINT('Ctrl Pts',(-56.396339747736,-108.235002850448,178.072094410988));
#25072=CARTESIAN_POINT('Ctrl Pts',(-55.5269697139578,-108.233402275661,
177.207792449865));
#25073=CARTESIAN_POINT('Ctrl Pts',(-55.5170317018976,-108.140180505584,
175.985484945604));
#25074=CARTESIAN_POINT('Ctrl Pts',(-55.5070936898375,-108.046958735507,
174.763177441344));
#25075=CARTESIAN_POINT('Ctrl Pts',(-56.3565876697041,-107.862115773316,
173.89887555255));
#25076=CARTESIAN_POINT('Ctrl Pts',(-57.2060816495708,-107.677272811126,
173.034573663757));
#25077=CARTESIAN_POINT('Ctrl Pts',(-58.4115639866396,-107.454479111736,
173.034573714903));
#25078=CARTESIAN_POINT('Ctrl Pts',(-59.6170463237085,-107.231685412347,
173.034573766048));
#25079=CARTESIAN_POINT('Ctrl Pts',(-60.4665402316527,-107.046842457824,
173.898875727171));
#25080=CARTESIAN_POINT('Ctrl Pts',(-61.3160341395969,-106.861999503301,
174.763177688294));
#25081=CARTESIAN_POINT('Ctrl Pts',(-61.306096025823,-106.768777744067,175.985485192554));
#25082=CARTESIAN_POINT('Ctrl Pts',(-61.2961579120492,-106.675555984834,
177.207792696815));
#25083=CARTESIAN_POINT('Ctrl Pts',(-60.4267878063484,-106.673955417714,
178.072094585608));
#25084=CARTESIAN_POINT('Ctrl Pts',(-59.5574177006478,-106.672354850594,
178.936396474401));
#25085=CARTESIAN_POINT('Ctrl Pts',(-58.3320592377449,-106.708705020672,
178.936396423256));
#25086=CARTESIAN_POINT('Ctrl Pts',(-57.106700774842,-106.74505519075,178.936396372111));
#25087=CARTESIAN_POINT('Ctrl Pts',(-56.2373307410638,-106.743454615963,
178.072094410988));
#25088=CARTESIAN_POINT('Ctrl Pts',(-55.3679607072856,-106.741854041175,
177.207792449865));
#25089=CARTESIAN_POINT('Ctrl Pts',(-55.3580226952254,-106.648632271098,
175.985484945604));
#25090=CARTESIAN_POINT('Ctrl Pts',(-55.3480846831652,-106.555410501021,
174.763177441344));
#25091=CARTESIAN_POINT('Ctrl Pts',(-56.1975786630319,-106.370567538831,
173.89887555255));
#25092=CARTESIAN_POINT('Ctrl Pts',(-57.0470726428986,-106.18572457664,173.034573663757));
#25093=CARTESIAN_POINT('Ctrl Pts',(-58.2525549799674,-105.962930877251,
173.034573714903));
#25094=CARTESIAN_POINT('Ctrl Pts',(-59.4580373170363,-105.740137177862,
173.034573766048));
#25095=CARTESIAN_POINT('Ctrl Pts',(-60.3075312249805,-105.555294223339,
173.898875727171));
#25096=CARTESIAN_POINT('Ctrl Pts',(-61.1570251329247,-105.370451268815,
174.763177688294));
#25097=CARTESIAN_POINT('Ctrl Pts',(-61.1470870191508,-105.277229509582,
175.985485192554));
#25098=CARTESIAN_POINT('Ctrl Pts',(-61.1371489053769,-105.184007750348,
177.207792696815));
#25099=CARTESIAN_POINT('Ctrl Pts',(-60.2677787996762,-105.182407183228,
178.072094585608));
#25100=CARTESIAN_POINT('Ctrl Pts',(-59.3984086939755,-105.180806616108,
178.936396474401));
#25101=CARTESIAN_POINT('Ctrl Pts',(-58.1730502310727,-105.217156786186,
178.936396423256));
#25102=CARTESIAN_POINT('Ctrl Pts',(-56.9476917681698,-105.253506956265,
178.936396372111));
#25103=CARTESIAN_POINT('Ctrl Pts',(-56.0783217343916,-105.251906381477,
178.072094410988));
#25104=CARTESIAN_POINT('Ctrl Pts',(-55.2089517006133,-105.25030580669,177.207792449865));
#25105=CARTESIAN_POINT('Ctrl Pts',(-55.1990136885532,-105.157084036613,
175.985484945604));
#25106=CARTESIAN_POINT('Ctrl Pts',(-55.189075676493,-105.063862266536,174.763177441344));
#25107=CARTESIAN_POINT('Ctrl Pts',(-56.0385696563597,-104.879019304345,
173.89887555255));
#25108=CARTESIAN_POINT('Ctrl Pts',(-56.8880636362264,-104.694176342154,
173.034573663757));
#25109=CARTESIAN_POINT('Ctrl Pts',(-58.0935459732952,-104.471382642765,
173.034573714903));
#25110=CARTESIAN_POINT('Ctrl Pts',(-59.299028310364,-104.248588943376,173.034573766048));
#25111=CARTESIAN_POINT('Ctrl Pts',(-60.1485222183082,-104.063745988853,
173.898875727171));
#25112=CARTESIAN_POINT('Ctrl Pts',(-60.9980161262524,-103.87890303433,174.763177688294));
#25113=CARTESIAN_POINT('Ctrl Pts',(-60.9880780124786,-103.785681275096,
175.985485192554));
#25114=CARTESIAN_POINT('Ctrl Pts',(-60.9781398987047,-103.692459515862,
177.207792696815));
#25115=CARTESIAN_POINT('Ctrl Pts',(-60.108769793004,-103.690858948742,178.072094585608));
#25116=CARTESIAN_POINT('Ctrl Pts',(-59.2393996873033,-103.689258381622,
178.936396474401));
#25117=CARTESIAN_POINT('Ctrl Pts',(-58.0140412244004,-103.725608551701,
178.936396423256));
#25118=CARTESIAN_POINT('Ctrl Pts',(-56.7886827614976,-103.761958721779,
178.936396372111));
#25119=CARTESIAN_POINT('Ctrl Pts',(-55.9193127277193,-103.760358146992,
178.072094410988));
#25120=CARTESIAN_POINT('Ctrl Pts',(-55.0499426939411,-103.758757572204,
177.207792449865));
#25121=CARTESIAN_POINT('Ctrl Pts',(-55.0400046818809,-103.665535802127,
175.985484945604));
#25122=CARTESIAN_POINT('Ctrl Pts',(-55.0300666698208,-103.57231403205,174.763177441344));
#25123=CARTESIAN_POINT('Ctrl Pts',(-55.8795606496874,-103.387471069859,
173.89887555255));
#25124=CARTESIAN_POINT('Ctrl Pts',(-56.7290546295541,-103.202628107669,
173.034573663757));
#25125=CARTESIAN_POINT('Ctrl Pts',(-57.934536966623,-102.97983440828,173.034573714903));
#25126=CARTESIAN_POINT('Ctrl Pts',(-59.1400193036918,-102.757040708891,
173.034573766048));
#25127=CARTESIAN_POINT('Ctrl Pts',(-59.989513211636,-102.572197754367,173.898875727171));
#25128=CARTESIAN_POINT('Ctrl Pts',(-60.8390071195802,-102.387354799844,
174.763177688294));
#25129=CARTESIAN_POINT('Ctrl Pts',(-60.8290690058063,-102.29413304061,175.985485192554));
#25130=CARTESIAN_POINT('Ctrl Pts',(-60.8191308920325,-102.200911281377,
177.207792696815));
#25131=CARTESIAN_POINT('Ctrl Pts',(-59.9497607863318,-102.199310714257,
178.072094585608));
#25132=CARTESIAN_POINT('Ctrl Pts',(-59.0803906806311,-102.197710147137,
178.936396474401));
#25133=CARTESIAN_POINT('Ctrl Pts',(-57.8550322177282,-102.234060317215,
178.936396423256));
#25134=CARTESIAN_POINT('Ctrl Pts',(-56.6296737548253,-102.270410487293,
178.936396372111));
#25135=CARTESIAN_POINT('Ctrl Pts',(-55.7603037210471,-102.268809912506,
178.072094410988));
#25136=CARTESIAN_POINT('Ctrl Pts',(-54.8909336872689,-102.267209337719,
177.207792449865));
#25137=CARTESIAN_POINT('Ctrl Pts',(-54.8809956752087,-102.173987567642,
175.985484945604));
#25138=CARTESIAN_POINT('Ctrl Pts',(-54.8710576631486,-102.080765797565,
174.763177441344));
#25139=CARTESIAN_POINT('Ctrl Pts',(-55.7205516430152,-101.895922835374,
173.89887555255));
#25140=CARTESIAN_POINT('Ctrl Pts',(-56.5700456228819,-101.711079873183,
173.034573663757));
#25141=CARTESIAN_POINT('Ctrl Pts',(-57.7755279599507,-101.488286173794,
173.034573714903));
#25142=CARTESIAN_POINT('Ctrl Pts',(-58.9810102970196,-101.265492474405,
173.034573766048));
#25143=CARTESIAN_POINT('Ctrl Pts',(-59.8305042049638,-101.080649519882,
173.898875727171));
#25144=CARTESIAN_POINT('Ctrl Pts',(-60.679998112908,-100.895806565358,174.763177688294));
#25145=CARTESIAN_POINT('Ctrl Pts',(-60.6700599991341,-100.802584806125,
175.985485192554));
#25146=CARTESIAN_POINT('Ctrl Pts',(-60.6601218853602,-100.709363046891,
177.207792696815));
#25147=CARTESIAN_POINT('Ctrl Pts',(-59.7907517796595,-100.707762479771,
178.072094585608));
#25148=CARTESIAN_POINT('Ctrl Pts',(-58.9213816739588,-100.706161912651,
178.936396474401));
#25149=CARTESIAN_POINT('Ctrl Pts',(-57.696023211056,-100.742512082729,178.936396423256));
#25150=CARTESIAN_POINT('Ctrl Pts',(-56.4706647481531,-100.778862252808,
178.936396372111));
#25151=CARTESIAN_POINT('Ctrl Pts',(-55.6012947143749,-100.77726167802,178.072094410988));
#25152=CARTESIAN_POINT('Ctrl Pts',(-54.7319246805966,-100.775661103233,
177.207792449865));
#25153=CARTESIAN_POINT('Ctrl Pts',(-54.7219866685365,-100.682439333156,
175.985484945604));
#25154=CARTESIAN_POINT('Ctrl Pts',(-54.7120486564763,-100.589217563079,
174.763177441344));
#25155=CARTESIAN_POINT('Ctrl Pts',(-55.561542636343,-100.404374600888,173.89887555255));
#25156=CARTESIAN_POINT('Ctrl Pts',(-56.4110366162097,-100.219531638698,
173.034573663757));
#25157=CARTESIAN_POINT('Ctrl Pts',(-57.6165189532785,-99.9967379393085,
173.034573714903));
#25158=CARTESIAN_POINT('Ctrl Pts',(-58.8220012903473,-99.7739442399195,
173.034573766048));
#25159=CARTESIAN_POINT('Ctrl Pts',(-59.6714951982915,-99.5891012853962,
173.898875727171));
#25160=CARTESIAN_POINT('Ctrl Pts',(-60.5209891062358,-99.4042583308729,
174.763177688294));
#25161=CARTESIAN_POINT('Ctrl Pts',(-60.5110509924619,-99.3110365716392,
175.985485192554));
#25162=CARTESIAN_POINT('Ctrl Pts',(-60.501112878688,-99.2178148124055,177.207792696815));
#25163=CARTESIAN_POINT('Ctrl Pts',(-59.6317427729873,-99.2162142452855,
178.072094585608));
#25164=CARTESIAN_POINT('Ctrl Pts',(-58.7623726672866,-99.2146136781656,
178.936396474401));
#25165=CARTESIAN_POINT('Ctrl Pts',(-57.5370142043838,-99.2509638482439,
178.936396423256));
#25166=CARTESIAN_POINT('Ctrl Pts',(-56.3116557414809,-99.2873140183222,
178.936396372111));
#25167=CARTESIAN_POINT('Ctrl Pts',(-55.4422857077027,-99.2857134435348,
178.072094410988));
#25168=CARTESIAN_POINT('Ctrl Pts',(-54.5729156739244,-99.2841128687474,
177.207792449865));
#25169=CARTESIAN_POINT('Ctrl Pts',(-54.5629776618643,-99.1908910986704,
175.985484945604));
#25170=CARTESIAN_POINT('Ctrl Pts',(-54.5530396498041,-99.0976693285933,
174.763177441344));
#25171=CARTESIAN_POINT('Ctrl Pts',(-55.4025336296708,-98.9128263664026,
173.89887555255));
#25172=CARTESIAN_POINT('Ctrl Pts',(-56.2520276095374,-98.727983404212,173.034573663757));
#25173=CARTESIAN_POINT('Ctrl Pts',(-57.4575099466063,-98.5051897048229,
173.034573714903));
#25174=CARTESIAN_POINT('Ctrl Pts',(-58.6629922836751,-98.2823960054338,
173.034573766048));
#25175=CARTESIAN_POINT('Ctrl Pts',(-59.5124861916193,-98.0975530509106,
173.898875727171));
#25176=CARTESIAN_POINT('Ctrl Pts',(-60.3619800995635,-97.9127100963873,
174.763177688294));
#25177=CARTESIAN_POINT('Ctrl Pts',(-60.3520419857897,-97.8194883371536,
175.985485192554));
#25178=CARTESIAN_POINT('Ctrl Pts',(-60.3421038720158,-97.7262665779199,
177.207792696815));
#25179=CARTESIAN_POINT('Ctrl Pts',(-59.4727337663151,-97.7246660108,178.072094585608));
#25180=CARTESIAN_POINT('Ctrl Pts',(-58.6033636606144,-97.72306544368,178.936396474401));
#25181=CARTESIAN_POINT('Ctrl Pts',(-57.3780051977115,-97.7594156137583,
178.936396423256));
#25182=CARTESIAN_POINT('Ctrl Pts',(-56.1526467348087,-97.7957657838366,
178.936396372111));
#25183=CARTESIAN_POINT('Ctrl Pts',(-55.2832767010304,-97.7941652090492,
178.072094410988));
#25184=CARTESIAN_POINT('Ctrl Pts',(-56.1707931031902,-113.117197303651,
178.813912075476));
#25185=CARTESIAN_POINT('Ctrl Pts',(-54.9958834532485,-113.148169293224,
177.6423391512));
#25186=CARTESIAN_POINT('Ctrl Pts',(-54.9859454592686,-113.05494752122,175.985484901707));
#25187=CARTESIAN_POINT('Ctrl Pts',(-54.9760074652888,-112.961725749215,
174.328630652215));
#25188=CARTESIAN_POINT('Ctrl Pts',(-56.1310410868884,-112.744310219938,
173.157057825983));
#25189=CARTESIAN_POINT('Ctrl Pts',(-57.286074708488,-112.52689469066,171.985484999752));
#25190=CARTESIAN_POINT('Ctrl Pts',(-58.9236553326579,-112.258036427063,
171.985485069079));
#25191=CARTESIAN_POINT('Ctrl Pts',(-60.5612359568277,-111.989178163466,
171.985485138407));
#25192=CARTESIAN_POINT('Ctrl Pts',(-61.7162694809355,-111.771762644582,
173.157058062683));
#25193=CARTESIAN_POINT('Ctrl Pts',(-62.8713030050432,-111.554347125698,
174.328630986959));
#25194=CARTESIAN_POINT('Ctrl Pts',(-62.861364873189,-111.461125368392,175.985485236451));
#25195=CARTESIAN_POINT('Ctrl Pts',(-62.8514267413349,-111.367903611086,
177.642339485944));
#25196=CARTESIAN_POINT('Ctrl Pts',(-61.6765169939012,-111.398875611052,
178.813912312176));
#25197=CARTESIAN_POINT('Ctrl Pts',(-60.5016072464676,-111.429847611019,
179.985485138407));
#25198=CARTESIAN_POINT('Ctrl Pts',(-58.8441504964637,-111.512262345305,
179.985485069079));
#25199=CARTESIAN_POINT('Ctrl Pts',(-57.1866937464598,-111.594677079592,
179.985484999752));
#25200=CARTESIAN_POINT('Ctrl Pts',(-56.011784096518,-111.625649069165,178.813912075476));
#25201=CARTESIAN_POINT('Ctrl Pts',(-54.8368744465762,-111.656621058739,
177.6423391512));
#25202=CARTESIAN_POINT('Ctrl Pts',(-54.8269364525964,-111.563399286734,
175.985484901707));
#25203=CARTESIAN_POINT('Ctrl Pts',(-54.8169984586165,-111.47017751473,174.328630652215));
#25204=CARTESIAN_POINT('Ctrl Pts',(-55.9720320802161,-111.252761985452,
173.157057825983));
#25205=CARTESIAN_POINT('Ctrl Pts',(-57.1270657018158,-111.035346456175,
171.985484999752));
#25206=CARTESIAN_POINT('Ctrl Pts',(-58.7646463259856,-110.766488192578,
171.985485069079));
#25207=CARTESIAN_POINT('Ctrl Pts',(-60.4022269501555,-110.497629928981,
171.985485138407));
#25208=CARTESIAN_POINT('Ctrl Pts',(-61.5572604742632,-110.280214410097,
173.157058062683));
#25209=CARTESIAN_POINT('Ctrl Pts',(-62.712293998371,-110.062798891212,174.328630986959));
#25210=CARTESIAN_POINT('Ctrl Pts',(-62.7023558665168,-109.969577133906,
175.985485236451));
#25211=CARTESIAN_POINT('Ctrl Pts',(-62.6924177346626,-109.8763553766,177.642339485944));
#25212=CARTESIAN_POINT('Ctrl Pts',(-61.517507987229,-109.907327376567,178.813912312176));
#25213=CARTESIAN_POINT('Ctrl Pts',(-60.3425982397954,-109.938299376534,
179.985485138407));
#25214=CARTESIAN_POINT('Ctrl Pts',(-58.6851414897915,-110.02071411082,179.985485069079));
#25215=CARTESIAN_POINT('Ctrl Pts',(-57.0276847397876,-110.103128845106,
179.985484999752));
#25216=CARTESIAN_POINT('Ctrl Pts',(-55.8527750898458,-110.13410083468,178.813912075476));
#25217=CARTESIAN_POINT('Ctrl Pts',(-54.677865439904,-110.165072824253,177.6423391512));
#25218=CARTESIAN_POINT('Ctrl Pts',(-54.6679274459242,-110.071851052249,
175.985484901707));
#25219=CARTESIAN_POINT('Ctrl Pts',(-54.6579894519443,-109.978629280244,
174.328630652215));
#25220=CARTESIAN_POINT('Ctrl Pts',(-55.8130230735439,-109.761213750967,
173.157057825983));
#25221=CARTESIAN_POINT('Ctrl Pts',(-56.9680566951435,-109.543798221689,
171.985484999752));
#25222=CARTESIAN_POINT('Ctrl Pts',(-58.6056373193134,-109.274939958092,
171.985485069079));
#25223=CARTESIAN_POINT('Ctrl Pts',(-60.2432179434833,-109.006081694495,
171.985485138407));
#25224=CARTESIAN_POINT('Ctrl Pts',(-61.398251467591,-108.788666175611,173.157058062683));
#25225=CARTESIAN_POINT('Ctrl Pts',(-62.5532849916988,-108.571250656727,
174.328630986959));
#25226=CARTESIAN_POINT('Ctrl Pts',(-62.5433468598446,-108.478028899421,
175.985485236451));
#25227=CARTESIAN_POINT('Ctrl Pts',(-62.5334087279904,-108.384807142114,
177.642339485944));
#25228=CARTESIAN_POINT('Ctrl Pts',(-61.3584989805568,-108.415779142081,
178.813912312176));
#25229=CARTESIAN_POINT('Ctrl Pts',(-60.1835892331231,-108.446751142048,
179.985485138407));
#25230=CARTESIAN_POINT('Ctrl Pts',(-58.5261324831192,-108.529165876334,
179.985485069079));
#25231=CARTESIAN_POINT('Ctrl Pts',(-56.8686757331153,-108.611580610621,
179.985484999752));
#25232=CARTESIAN_POINT('Ctrl Pts',(-55.6937660831736,-108.642552600194,
178.813912075476));
#25233=CARTESIAN_POINT('Ctrl Pts',(-54.5188564332318,-108.673524589768,
177.6423391512));
#25234=CARTESIAN_POINT('Ctrl Pts',(-54.5089184392519,-108.580302817763,
175.985484901707));
#25235=CARTESIAN_POINT('Ctrl Pts',(-54.4989804452721,-108.487081045759,
174.328630652215));
#25236=CARTESIAN_POINT('Ctrl Pts',(-55.6540140668717,-108.269665516481,
173.157057825983));
#25237=CARTESIAN_POINT('Ctrl Pts',(-56.8090476884713,-108.052249987204,
171.985484999752));
#25238=CARTESIAN_POINT('Ctrl Pts',(-58.4466283126412,-107.783391723607,
171.985485069079));
#25239=CARTESIAN_POINT('Ctrl Pts',(-60.084208936811,-107.51453346001,171.985485138407));
#25240=CARTESIAN_POINT('Ctrl Pts',(-61.2392424609188,-107.297117941125,
173.157058062683));
#25241=CARTESIAN_POINT('Ctrl Pts',(-62.3942759850265,-107.079702422241,
174.328630986959));
#25242=CARTESIAN_POINT('Ctrl Pts',(-62.3843378531723,-106.986480664935,
175.985485236451));
#25243=CARTESIAN_POINT('Ctrl Pts',(-62.3743997213182,-106.893258907629,
177.642339485944));
#25244=CARTESIAN_POINT('Ctrl Pts',(-61.1994899738845,-106.924230907596,
178.813912312176));
#25245=CARTESIAN_POINT('Ctrl Pts',(-60.0245802264509,-106.955202907562,
179.985485138407));
#25246=CARTESIAN_POINT('Ctrl Pts',(-58.367123476447,-107.037617641849,179.985485069079));
#25247=CARTESIAN_POINT('Ctrl Pts',(-56.7096667264431,-107.120032376135,
179.985484999752));
#25248=CARTESIAN_POINT('Ctrl Pts',(-55.5347570765013,-107.151004365708,
178.813912075476));
#25249=CARTESIAN_POINT('Ctrl Pts',(-54.3598474265596,-107.181976355282,
177.6423391512));
#25250=CARTESIAN_POINT('Ctrl Pts',(-54.3499094325797,-107.088754583277,
175.985484901707));
#25251=CARTESIAN_POINT('Ctrl Pts',(-54.3399714385998,-106.995532811273,
174.328630652215));
#25252=CARTESIAN_POINT('Ctrl Pts',(-55.4950050601995,-106.778117281995,
173.157057825983));
#25253=CARTESIAN_POINT('Ctrl Pts',(-56.6500386817991,-106.560701752718,
171.985484999752));
#25254=CARTESIAN_POINT('Ctrl Pts',(-58.2876193059689,-106.291843489121,
171.985485069079));
#25255=CARTESIAN_POINT('Ctrl Pts',(-59.9251999301388,-106.022985225524,
171.985485138407));
#25256=CARTESIAN_POINT('Ctrl Pts',(-61.0802334542465,-105.80556970664,173.157058062683));
#25257=CARTESIAN_POINT('Ctrl Pts',(-62.2352669783543,-105.588154187756,
174.328630986959));
#25258=CARTESIAN_POINT('Ctrl Pts',(-62.2253288465001,-105.494932430449,
175.985485236451));
#25259=CARTESIAN_POINT('Ctrl Pts',(-62.2153907146459,-105.401710673143,
177.642339485944));
#25260=CARTESIAN_POINT('Ctrl Pts',(-61.0404809672123,-105.43268267311,178.813912312176));
#25261=CARTESIAN_POINT('Ctrl Pts',(-59.8655712197787,-105.463654673077,
179.985485138407));
#25262=CARTESIAN_POINT('Ctrl Pts',(-58.2081144697748,-105.546069407363,
179.985485069079));
#25263=CARTESIAN_POINT('Ctrl Pts',(-56.5506577197709,-105.628484141649,
179.985484999752));
#25264=CARTESIAN_POINT('Ctrl Pts',(-55.3757480698291,-105.659456131223,
178.813912075476));
#25265=CARTESIAN_POINT('Ctrl Pts',(-54.2008384198873,-105.690428120796,
177.6423391512));
#25266=CARTESIAN_POINT('Ctrl Pts',(-54.1909004259075,-105.597206348792,
175.985484901707));
#25267=CARTESIAN_POINT('Ctrl Pts',(-54.1809624319276,-105.503984576787,
174.328630652215));
#25268=CARTESIAN_POINT('Ctrl Pts',(-55.3359960535272,-105.28656904751,173.157057825983));
#25269=CARTESIAN_POINT('Ctrl Pts',(-56.4910296751268,-105.069153518232,
171.985484999752));
#25270=CARTESIAN_POINT('Ctrl Pts',(-58.1286102992967,-104.800295254635,
171.985485069079));
#25271=CARTESIAN_POINT('Ctrl Pts',(-59.7661909234666,-104.531436991038,
171.985485138407));
#25272=CARTESIAN_POINT('Ctrl Pts',(-60.9212244475743,-104.314021472154,
173.157058062683));
#25273=CARTESIAN_POINT('Ctrl Pts',(-62.0762579716821,-104.09660595327,174.328630986959));
#25274=CARTESIAN_POINT('Ctrl Pts',(-62.0663198398279,-104.003384195964,
175.985485236451));
#25275=CARTESIAN_POINT('Ctrl Pts',(-62.0563817079737,-103.910162438658,
177.642339485944));
#25276=CARTESIAN_POINT('Ctrl Pts',(-60.8814719605401,-103.941134438624,
178.813912312176));
#25277=CARTESIAN_POINT('Ctrl Pts',(-59.7065622131064,-103.972106438591,
179.985485138407));
#25278=CARTESIAN_POINT('Ctrl Pts',(-58.0491054631025,-104.054521172878,
179.985485069079));
#25279=CARTESIAN_POINT('Ctrl Pts',(-56.3916487130987,-104.136935907164,
179.985484999752));
#25280=CARTESIAN_POINT('Ctrl Pts',(-55.2167390631569,-104.167907896737,
178.813912075476));
#25281=CARTESIAN_POINT('Ctrl Pts',(-54.0418294132151,-104.198879886311,
177.6423391512));
#25282=CARTESIAN_POINT('Ctrl Pts',(-54.0318914192353,-104.105658114306,
175.985484901707));
#25283=CARTESIAN_POINT('Ctrl Pts',(-54.0219534252554,-104.012436342302,
174.328630652215));
#25284=CARTESIAN_POINT('Ctrl Pts',(-55.176987046855,-103.795020813024,173.157057825983));
#25285=CARTESIAN_POINT('Ctrl Pts',(-56.3320206684546,-103.577605283747,
171.985484999752));
#25286=CARTESIAN_POINT('Ctrl Pts',(-57.9696012926245,-103.30874702015,171.985485069079));
#25287=CARTESIAN_POINT('Ctrl Pts',(-59.6071819167943,-103.039888756553,
171.985485138407));
#25288=CARTESIAN_POINT('Ctrl Pts',(-60.7622154409021,-102.822473237669,
173.157058062683));
#25289=CARTESIAN_POINT('Ctrl Pts',(-61.9172489650099,-102.605057718784,
174.328630986959));
#25290=CARTESIAN_POINT('Ctrl Pts',(-61.9073108331557,-102.511835961478,
175.985485236451));
#25291=CARTESIAN_POINT('Ctrl Pts',(-61.8973727013015,-102.418614204172,
177.642339485944));
#25292=CARTESIAN_POINT('Ctrl Pts',(-60.7224629538678,-102.449586204139,
178.813912312176));
#25293=CARTESIAN_POINT('Ctrl Pts',(-59.5475532064342,-102.480558204106,
179.985485138407));
#25294=CARTESIAN_POINT('Ctrl Pts',(-57.8900964564303,-102.562972938392,
179.985485069079));
#25295=CARTESIAN_POINT('Ctrl Pts',(-56.2326397064264,-102.645387672678,
179.985484999752));
#25296=CARTESIAN_POINT('Ctrl Pts',(-55.0577300564847,-102.676359662252,
178.813912075476));
#25297=CARTESIAN_POINT('Ctrl Pts',(-53.8828204065429,-102.707331651825,
177.6423391512));
#25298=CARTESIAN_POINT('Ctrl Pts',(-53.872882412563,-102.614109879821,175.985484901707));
#25299=CARTESIAN_POINT('Ctrl Pts',(-53.8629444185832,-102.520888107816,
174.328630652215));
#25300=CARTESIAN_POINT('Ctrl Pts',(-55.0179780401828,-102.303472578539,
173.157057825983));
#25301=CARTESIAN_POINT('Ctrl Pts',(-56.1730116617824,-102.086057049261,
171.985484999752));
#25302=CARTESIAN_POINT('Ctrl Pts',(-57.8105922859523,-101.817198785664,
171.985485069079));
#25303=CARTESIAN_POINT('Ctrl Pts',(-59.4481729101221,-101.548340522067,
171.985485138407));
#25304=CARTESIAN_POINT('Ctrl Pts',(-60.6032064342299,-101.330925003183,
173.157058062683));
#25305=CARTESIAN_POINT('Ctrl Pts',(-61.7582399583376,-101.113509484299,
174.328630986959));
#25306=CARTESIAN_POINT('Ctrl Pts',(-61.7483018264834,-101.020287726993,
175.985485236451));
#25307=CARTESIAN_POINT('Ctrl Pts',(-61.7383636946293,-100.927065969686,
177.642339485944));
#25308=CARTESIAN_POINT('Ctrl Pts',(-60.5634539471956,-100.958037969653,
178.813912312176));
#25309=CARTESIAN_POINT('Ctrl Pts',(-59.388544199762,-100.98900996962,179.985485138407));
#25310=CARTESIAN_POINT('Ctrl Pts',(-57.7310874497581,-101.071424703906,
179.985485069079));
#25311=CARTESIAN_POINT('Ctrl Pts',(-56.0736306997542,-101.153839438193,
179.985484999752));
#25312=CARTESIAN_POINT('Ctrl Pts',(-54.8987210498124,-101.184811427766,
178.813912075476));
#25313=CARTESIAN_POINT('Ctrl Pts',(-53.7238113998707,-101.21578341734,177.6423391512));
#25314=CARTESIAN_POINT('Ctrl Pts',(-53.7138734058908,-101.122561645335,
175.985484901707));
#25315=CARTESIAN_POINT('Ctrl Pts',(-53.7039354119109,-101.029339873331,
174.328630652215));
#25316=CARTESIAN_POINT('Ctrl Pts',(-54.8589690335105,-100.811924344053,
173.157057825983));
#25317=CARTESIAN_POINT('Ctrl Pts',(-56.0140026551102,-100.594508814776,
171.985484999752));
#25318=CARTESIAN_POINT('Ctrl Pts',(-57.65158327928,-100.325650551179,171.985485069079));
#25319=CARTESIAN_POINT('Ctrl Pts',(-59.2891639034499,-100.056792287582,
171.985485138407));
#25320=CARTESIAN_POINT('Ctrl Pts',(-60.4441974275576,-99.8393767686974,
173.157058062683));
#25321=CARTESIAN_POINT('Ctrl Pts',(-61.5992309516654,-99.6219612498133,
174.328630986959));
#25322=CARTESIAN_POINT('Ctrl Pts',(-61.5892928198112,-99.528739492507,175.985485236451));
#25323=CARTESIAN_POINT('Ctrl Pts',(-61.579354687957,-99.4355177352008,177.642339485944));
#25324=CARTESIAN_POINT('Ctrl Pts',(-60.4044449405234,-99.4664897351676,
178.813912312176));
#25325=CARTESIAN_POINT('Ctrl Pts',(-59.2295351930898,-99.4974617351344,
179.985485138407));
#25326=CARTESIAN_POINT('Ctrl Pts',(-57.5720784430859,-99.5798764694207,
179.985485069079));
#25327=CARTESIAN_POINT('Ctrl Pts',(-55.914621693082,-99.662291203707,179.985484999752));
#25328=CARTESIAN_POINT('Ctrl Pts',(-54.7397120431402,-99.6932631932805,
178.813912075476));
#25329=CARTESIAN_POINT('Ctrl Pts',(-53.5648023931984,-99.724235182854,177.6423391512));
#25330=CARTESIAN_POINT('Ctrl Pts',(-53.5548643992186,-99.6310134108495,
175.985484901707));
#25331=CARTESIAN_POINT('Ctrl Pts',(-53.5449264052387,-99.5377916388449,
174.328630652215));
#25332=CARTESIAN_POINT('Ctrl Pts',(-54.6999600268383,-99.3203761095675,
173.157057825983));
#25333=CARTESIAN_POINT('Ctrl Pts',(-55.8549936484379,-99.10296058029,171.985484999752));
#25334=CARTESIAN_POINT('Ctrl Pts',(-57.4925742726078,-98.834102316693,171.985485069079));
#25335=CARTESIAN_POINT('Ctrl Pts',(-59.1301548967777,-98.565244053096,171.985485138407));
#25336=CARTESIAN_POINT('Ctrl Pts',(-60.2851884208854,-98.3478285342118,
173.157058062683));
#25337=CARTESIAN_POINT('Ctrl Pts',(-61.4402219449932,-98.1304130153276,
174.328630986959));
#25338=CARTESIAN_POINT('Ctrl Pts',(-61.430283813139,-98.0371912580215,175.985485236451));
#25339=CARTESIAN_POINT('Ctrl Pts',(-61.4203456812848,-97.9439695007152,
177.642339485944));
#25340=CARTESIAN_POINT('Ctrl Pts',(-60.2454359338512,-97.974941500682,178.813912312176));
#25341=CARTESIAN_POINT('Ctrl Pts',(-59.0705261864175,-98.0059135006488,
179.985485138407));
#25342=CARTESIAN_POINT('Ctrl Pts',(-57.4130694364136,-98.0883282349351,
179.985485069079));
#25343=CARTESIAN_POINT('Ctrl Pts',(-55.7556126864097,-98.1707429692214,
179.985484999752));
#25344=CARTESIAN_POINT('Ctrl Pts',(-54.580703036468,-98.2017149587949,178.813912075476));
#25345=CARTESIAN_POINT('Ctrl Pts',(-61.8126236112619,-109.901486190407,
178.485485069079));
#25346=CARTESIAN_POINT('Ctrl Pts',(-61.6740514069051,-109.903200708285,
178.657813499464));
#25347=CARTESIAN_POINT('Ctrl Pts',(-61.517507987229,-109.907327376567,178.813912312176));
#25348=CARTESIAN_POINT('Ctrl Pts',(-60.3425982397954,-109.938299376534,
179.985485138407));
#25349=CARTESIAN_POINT('Ctrl Pts',(-58.6851414897915,-110.02071411082,179.985485069079));
#25350=CARTESIAN_POINT('Ctrl Pts',(-57.0276847397876,-110.103128845106,
179.985484999752));
#25351=CARTESIAN_POINT('Ctrl Pts',(-55.8527750898458,-110.13410083468,178.813912075476));
#25352=CARTESIAN_POINT('Ctrl Pts',(-54.677865439904,-110.165072824253,177.6423391512));
#25353=CARTESIAN_POINT('Ctrl Pts',(-54.6679274459242,-110.071851052249,
175.985484901707));
#25354=CARTESIAN_POINT('Ctrl Pts',(-54.6579894519443,-109.978629280244,
174.328630652215));
#25355=CARTESIAN_POINT('Ctrl Pts',(-55.8130230735439,-109.761213750967,
173.157057825983));
#25356=CARTESIAN_POINT('Ctrl Pts',(-56.9680566951435,-109.543798221689,
171.985484999752));
#25357=CARTESIAN_POINT('Ctrl Pts',(-58.6056373193134,-109.274939958092,
171.985485069079));
#25358=CARTESIAN_POINT('Ctrl Pts',(-60.2432179434833,-109.006081694495,
171.985485138407));
#25359=CARTESIAN_POINT('Ctrl Pts',(-61.398251467591,-108.788666175611,173.157058062683));
#25360=CARTESIAN_POINT('Ctrl Pts',(-61.5521464885441,-108.759698041669,
173.313156769748));
#25361=CARTESIAN_POINT('Ctrl Pts',(-61.687965692515,-108.732160612486,173.485485069079));
#25362=CARTESIAN_POINT('Ctrl Pts',(-56.1707931031902,-113.117197303651,
178.813912075476));
#25363=CARTESIAN_POINT('Ctrl Pts',(-54.9958834532485,-113.148169293224,
177.6423391512));
#25364=CARTESIAN_POINT('Ctrl Pts',(-54.9859454592686,-113.05494752122,175.985484901707));
#25365=CARTESIAN_POINT('Ctrl Pts',(-54.9760074652888,-112.961725749215,
174.328630652215));
#25366=CARTESIAN_POINT('Ctrl Pts',(-56.1310410868884,-112.744310219938,
173.157057825983));
#25367=CARTESIAN_POINT('Ctrl Pts',(-57.286074708488,-112.52689469066,171.985484999752));
#25368=CARTESIAN_POINT('Ctrl Pts',(-58.9236553326578,-112.258036427063,
171.985485069079));
#25369=CARTESIAN_POINT('Ctrl Pts',(-60.5612359568277,-111.989178163466,
171.985485138407));
#25370=CARTESIAN_POINT('Ctrl Pts',(-61.7162694809355,-111.771762644582,
173.157058062683));
#25371=CARTESIAN_POINT('Ctrl Pts',(-62.8713030050432,-111.554347125698,
174.328630986959));
#25372=CARTESIAN_POINT('Ctrl Pts',(-62.861364873189,-111.461125368392,175.985485236451));
#25373=CARTESIAN_POINT('Ctrl Pts',(-62.8514267413349,-111.367903611086,
177.642339485944));
#25374=CARTESIAN_POINT('Ctrl Pts',(-61.6765169939012,-111.398875611052,
178.813912312176));
#25375=CARTESIAN_POINT('Ctrl Pts',(-60.5016072464676,-111.429847611019,
179.985485138407));
#25376=CARTESIAN_POINT('Ctrl Pts',(-58.8441504964637,-111.512262345305,
179.985485069079));
#25377=CARTESIAN_POINT('Ctrl Pts',(-57.1866937464598,-111.594677079592,
179.985484999752));
#25378=CARTESIAN_POINT('Ctrl Pts',(-56.011784096518,-111.625649069165,178.813912075476));
#25379=CARTESIAN_POINT('Ctrl Pts',(-54.8368744465763,-111.656621058739,
177.6423391512));
#25380=CARTESIAN_POINT('Ctrl Pts',(-54.8269364525964,-111.563399286734,
175.985484901707));
#25381=CARTESIAN_POINT('Ctrl Pts',(-54.8169984586165,-111.47017751473,174.328630652215));
#25382=CARTESIAN_POINT('Ctrl Pts',(-55.9720320802161,-111.252761985452,
173.157057825983));
#25383=CARTESIAN_POINT('Ctrl Pts',(-57.1270657018158,-111.035346456175,
171.985484999752));
#25384=CARTESIAN_POINT('Ctrl Pts',(-58.7646463259856,-110.766488192578,
171.985485069079));
#25385=CARTESIAN_POINT('Ctrl Pts',(-60.4022269501555,-110.497629928981,
171.985485138407));
#25386=CARTESIAN_POINT('Ctrl Pts',(-61.5572604742632,-110.280214410097,
173.157058062683));
#25387=CARTESIAN_POINT('Ctrl Pts',(-62.712293998371,-110.062798891212,174.328630986959));
#25388=CARTESIAN_POINT('Ctrl Pts',(-62.7023558665168,-109.969577133906,
175.985485236451));
#25389=CARTESIAN_POINT('Ctrl Pts',(-62.6924177346626,-109.8763553766,177.642339485944));
#25390=CARTESIAN_POINT('Ctrl Pts',(-61.517507987229,-109.907327376567,178.813912312176));
#25391=CARTESIAN_POINT('Ctrl Pts',(-60.3425982397954,-109.938299376534,
179.985485138407));
#25392=CARTESIAN_POINT('Ctrl Pts',(-58.6851414897915,-110.02071411082,179.985485069079));
#25393=CARTESIAN_POINT('Ctrl Pts',(-57.0276847397876,-110.103128845106,
179.985484999752));
#25394=CARTESIAN_POINT('Ctrl Pts',(-55.8527750898458,-110.13410083468,178.813912075476));
#25395=CARTESIAN_POINT('Ctrl Pts',(-54.677865439904,-110.165072824253,177.6423391512));
#25396=CARTESIAN_POINT('Ctrl Pts',(-54.6679274459242,-110.071851052249,
175.985484901707));
#25397=CARTESIAN_POINT('Ctrl Pts',(-54.6579894519443,-109.978629280244,
174.328630652215));
#25398=CARTESIAN_POINT('Ctrl Pts',(-55.8130230735439,-109.761213750967,
173.157057825983));
#25399=CARTESIAN_POINT('Ctrl Pts',(-56.9680566951435,-109.543798221689,
171.985484999752));
#25400=CARTESIAN_POINT('Ctrl Pts',(-58.6056373193134,-109.274939958092,
171.985485069079));
#25401=CARTESIAN_POINT('Ctrl Pts',(-60.2432179434833,-109.006081694495,
171.985485138407));
#25402=CARTESIAN_POINT('Ctrl Pts',(-61.398251467591,-108.788666175611,173.157058062683));
#25403=CARTESIAN_POINT('Ctrl Pts',(-62.5532849916988,-108.571250656727,
174.328630986959));
#25404=CARTESIAN_POINT('Ctrl Pts',(-62.5433468598446,-108.478028899421,
175.985485236451));
#25405=CARTESIAN_POINT('Ctrl Pts',(-62.5334087279904,-108.384807142114,
177.642339485944));
#25406=CARTESIAN_POINT('Ctrl Pts',(-61.3584989805568,-108.415779142081,
178.813912312176));
#25407=CARTESIAN_POINT('Ctrl Pts',(-60.1835892331231,-108.446751142048,
179.985485138407));
#25408=CARTESIAN_POINT('Ctrl Pts',(-58.5261324831192,-108.529165876334,
179.985485069079));
#25409=CARTESIAN_POINT('Ctrl Pts',(-56.8686757331153,-108.611580610621,
179.985484999752));
#25410=CARTESIAN_POINT('Ctrl Pts',(-55.6937660831736,-108.642552600194,
178.813912075476));
#25411=CARTESIAN_POINT('Ctrl Pts',(-54.5188564332318,-108.673524589768,
177.6423391512));
#25412=CARTESIAN_POINT('Ctrl Pts',(-54.5089184392519,-108.580302817763,
175.985484901707));
#25413=CARTESIAN_POINT('Ctrl Pts',(-54.4989804452721,-108.487081045759,
174.328630652215));
#25414=CARTESIAN_POINT('Ctrl Pts',(-55.6540140668717,-108.269665516481,
173.157057825983));
#25415=CARTESIAN_POINT('Ctrl Pts',(-56.8090476884713,-108.052249987204,
171.985484999752));
#25416=CARTESIAN_POINT('Ctrl Pts',(-58.4466283126412,-107.783391723607,
171.985485069079));
#25417=CARTESIAN_POINT('Ctrl Pts',(-60.084208936811,-107.51453346001,171.985485138407));
#25418=CARTESIAN_POINT('Ctrl Pts',(-61.2392424609188,-107.297117941125,
173.157058062683));
#25419=CARTESIAN_POINT('Ctrl Pts',(-62.3942759850265,-107.079702422241,
174.328630986959));
#25420=CARTESIAN_POINT('Ctrl Pts',(-62.3843378531723,-106.986480664935,
175.985485236451));
#25421=CARTESIAN_POINT('Ctrl Pts',(-62.3743997213182,-106.893258907629,
177.642339485944));
#25422=CARTESIAN_POINT('Ctrl Pts',(-61.1994899738845,-106.924230907596,
178.813912312176));
#25423=CARTESIAN_POINT('Ctrl Pts',(-60.0245802264509,-106.955202907562,
179.985485138407));
#25424=CARTESIAN_POINT('Ctrl Pts',(-58.367123476447,-107.037617641849,179.985485069079));
#25425=CARTESIAN_POINT('Ctrl Pts',(-56.7096667264431,-107.120032376135,
179.985484999752));
#25426=CARTESIAN_POINT('Ctrl Pts',(-55.5347570765013,-107.151004365708,
178.813912075476));
#25427=CARTESIAN_POINT('Ctrl Pts',(-54.3598474265596,-107.181976355282,
177.6423391512));
#25428=CARTESIAN_POINT('Ctrl Pts',(-54.3499094325797,-107.088754583277,
175.985484901707));
#25429=CARTESIAN_POINT('Ctrl Pts',(-54.3399714385998,-106.995532811273,
174.328630652215));
#25430=CARTESIAN_POINT('Ctrl Pts',(-55.4950050601995,-106.778117281995,
173.157057825983));
#25431=CARTESIAN_POINT('Ctrl Pts',(-56.6500386817991,-106.560701752718,
171.985484999752));
#25432=CARTESIAN_POINT('Ctrl Pts',(-58.2876193059689,-106.291843489121,
171.985485069079));
#25433=CARTESIAN_POINT('Ctrl Pts',(-59.9251999301388,-106.022985225524,
171.985485138407));
#25434=CARTESIAN_POINT('Ctrl Pts',(-61.0802334542465,-105.80556970664,173.157058062683));
#25435=CARTESIAN_POINT('Ctrl Pts',(-62.2352669783543,-105.588154187756,
174.328630986959));
#25436=CARTESIAN_POINT('Ctrl Pts',(-62.2253288465001,-105.494932430449,
175.985485236451));
#25437=CARTESIAN_POINT('Ctrl Pts',(-62.2153907146459,-105.401710673143,
177.642339485944));
#25438=CARTESIAN_POINT('Ctrl Pts',(-61.0404809672123,-105.43268267311,178.813912312176));
#25439=CARTESIAN_POINT('Ctrl Pts',(-59.8655712197787,-105.463654673077,
179.985485138407));
#25440=CARTESIAN_POINT('Ctrl Pts',(-58.2081144697748,-105.546069407363,
179.985485069079));
#25441=CARTESIAN_POINT('Ctrl Pts',(-56.5506577197709,-105.628484141649,
179.985484999752));
#25442=CARTESIAN_POINT('Ctrl Pts',(-55.3757480698291,-105.659456131223,
178.813912075476));
#25443=CARTESIAN_POINT('Ctrl Pts',(-54.2008384198873,-105.690428120796,
177.6423391512));
#25444=CARTESIAN_POINT('Ctrl Pts',(-54.1909004259075,-105.597206348792,
175.985484901707));
#25445=CARTESIAN_POINT('Ctrl Pts',(-54.1809624319276,-105.503984576787,
174.328630652215));
#25446=CARTESIAN_POINT('Ctrl Pts',(-55.3359960535272,-105.28656904751,173.157057825983));
#25447=CARTESIAN_POINT('Ctrl Pts',(-56.4910296751268,-105.069153518232,
171.985484999752));
#25448=CARTESIAN_POINT('Ctrl Pts',(-58.1286102992967,-104.800295254635,
171.985485069079));
#25449=CARTESIAN_POINT('Ctrl Pts',(-59.7661909234666,-104.531436991038,
171.985485138407));
#25450=CARTESIAN_POINT('Ctrl Pts',(-60.9212244475743,-104.314021472154,
173.157058062683));
#25451=CARTESIAN_POINT('Ctrl Pts',(-62.0762579716821,-104.09660595327,174.328630986959));
#25452=CARTESIAN_POINT('Ctrl Pts',(-62.0663198398279,-104.003384195964,
175.985485236451));
#25453=CARTESIAN_POINT('Ctrl Pts',(-62.0563817079737,-103.910162438658,
177.642339485944));
#25454=CARTESIAN_POINT('Ctrl Pts',(-60.8814719605401,-103.941134438624,
178.813912312176));
#25455=CARTESIAN_POINT('Ctrl Pts',(-59.7065622131064,-103.972106438591,
179.985485138407));
#25456=CARTESIAN_POINT('Ctrl Pts',(-58.0491054631025,-104.054521172878,
179.985485069079));
#25457=CARTESIAN_POINT('Ctrl Pts',(-56.3916487130987,-104.136935907164,
179.985484999752));
#25458=CARTESIAN_POINT('Ctrl Pts',(-55.2167390631569,-104.167907896737,
178.813912075476));
#25459=CARTESIAN_POINT('Ctrl Pts',(-54.0418294132151,-104.198879886311,
177.6423391512));
#25460=CARTESIAN_POINT('Ctrl Pts',(-54.0318914192353,-104.105658114306,
175.985484901707));
#25461=CARTESIAN_POINT('Ctrl Pts',(-54.0219534252554,-104.012436342302,
174.328630652215));
#25462=CARTESIAN_POINT('Ctrl Pts',(-55.176987046855,-103.795020813024,173.157057825983));
#25463=CARTESIAN_POINT('Ctrl Pts',(-56.3320206684546,-103.577605283747,
171.985484999752));
#25464=CARTESIAN_POINT('Ctrl Pts',(-57.9696012926245,-103.30874702015,171.985485069079));
#25465=CARTESIAN_POINT('Ctrl Pts',(-59.6071819167943,-103.039888756553,
171.985485138407));
#25466=CARTESIAN_POINT('Ctrl Pts',(-60.7622154409021,-102.822473237669,
173.157058062683));
#25467=CARTESIAN_POINT('Ctrl Pts',(-61.9172489650099,-102.605057718784,
174.328630986959));
#25468=CARTESIAN_POINT('Ctrl Pts',(-61.9073108331557,-102.511835961478,
175.985485236451));
#25469=CARTESIAN_POINT('Ctrl Pts',(-61.8973727013015,-102.418614204172,
177.642339485944));
#25470=CARTESIAN_POINT('Ctrl Pts',(-60.7224629538678,-102.449586204139,
178.813912312176));
#25471=CARTESIAN_POINT('Ctrl Pts',(-59.5475532064342,-102.480558204106,
179.985485138407));
#25472=CARTESIAN_POINT('Ctrl Pts',(-57.8900964564303,-102.562972938392,
179.985485069079));
#25473=CARTESIAN_POINT('Ctrl Pts',(-56.2326397064264,-102.645387672678,
179.985484999752));
#25474=CARTESIAN_POINT('Ctrl Pts',(-55.0577300564847,-102.676359662252,
178.813912075476));
#25475=CARTESIAN_POINT('Ctrl Pts',(-53.8828204065429,-102.707331651825,
177.6423391512));
#25476=CARTESIAN_POINT('Ctrl Pts',(-53.872882412563,-102.614109879821,175.985484901707));
#25477=CARTESIAN_POINT('Ctrl Pts',(-53.8629444185832,-102.520888107816,
174.328630652215));
#25478=CARTESIAN_POINT('Ctrl Pts',(-55.0179780401828,-102.303472578539,
173.157057825983));
#25479=CARTESIAN_POINT('Ctrl Pts',(-56.1730116617824,-102.086057049261,
171.985484999752));
#25480=CARTESIAN_POINT('Ctrl Pts',(-57.8105922859523,-101.817198785664,
171.985485069079));
#25481=CARTESIAN_POINT('Ctrl Pts',(-59.4481729101221,-101.548340522067,
171.985485138407));
#25482=CARTESIAN_POINT('Ctrl Pts',(-60.6032064342299,-101.330925003183,
173.157058062683));
#25483=CARTESIAN_POINT('Ctrl Pts',(-61.7582399583376,-101.113509484299,
174.328630986959));
#25484=CARTESIAN_POINT('Ctrl Pts',(-61.7483018264834,-101.020287726993,
175.985485236451));
#25485=CARTESIAN_POINT('Ctrl Pts',(-61.7383636946293,-100.927065969686,
177.642339485944));
#25486=CARTESIAN_POINT('Ctrl Pts',(-60.5634539471956,-100.958037969653,
178.813912312176));
#25487=CARTESIAN_POINT('Ctrl Pts',(-59.388544199762,-100.98900996962,179.985485138407));
#25488=CARTESIAN_POINT('Ctrl Pts',(-57.7310874497581,-101.071424703906,
179.985485069079));
#25489=CARTESIAN_POINT('Ctrl Pts',(-56.0736306997542,-101.153839438193,
179.985484999752));
#25490=CARTESIAN_POINT('Ctrl Pts',(-54.8987210498124,-101.184811427766,
178.813912075476));
#25491=CARTESIAN_POINT('Ctrl Pts',(-53.7238113998707,-101.21578341734,177.6423391512));
#25492=CARTESIAN_POINT('Ctrl Pts',(-53.7138734058908,-101.122561645335,
175.985484901707));
#25493=CARTESIAN_POINT('Ctrl Pts',(-53.7039354119109,-101.029339873331,
174.328630652215));
#25494=CARTESIAN_POINT('Ctrl Pts',(-54.8589690335105,-100.811924344053,
173.157057825983));
#25495=CARTESIAN_POINT('Ctrl Pts',(-56.0140026551102,-100.594508814776,
171.985484999752));
#25496=CARTESIAN_POINT('Ctrl Pts',(-57.65158327928,-100.325650551179,171.985485069079));
#25497=CARTESIAN_POINT('Ctrl Pts',(-59.2891639034499,-100.056792287582,
171.985485138407));
#25498=CARTESIAN_POINT('Ctrl Pts',(-60.4441974275576,-99.8393767686974,
173.157058062683));
#25499=CARTESIAN_POINT('Ctrl Pts',(-61.5992309516654,-99.6219612498133,
174.328630986959));
#25500=CARTESIAN_POINT('Ctrl Pts',(-61.5892928198112,-99.528739492507,175.985485236451));
#25501=CARTESIAN_POINT('Ctrl Pts',(-61.579354687957,-99.4355177352008,177.642339485944));
#25502=CARTESIAN_POINT('Ctrl Pts',(-60.4044449405234,-99.4664897351676,
178.813912312176));
#25503=CARTESIAN_POINT('Ctrl Pts',(-59.2295351930898,-99.4974617351344,
179.985485138407));
#25504=CARTESIAN_POINT('Ctrl Pts',(-57.5720784430859,-99.5798764694207,
179.985485069079));
#25505=CARTESIAN_POINT('Ctrl Pts',(-55.914621693082,-99.662291203707,179.985484999752));
#25506=CARTESIAN_POINT('Ctrl Pts',(-54.7397120431402,-99.6932631932805,
178.813912075476));
#25507=CARTESIAN_POINT('Ctrl Pts',(-53.5648023931984,-99.724235182854,177.6423391512));
#25508=CARTESIAN_POINT('Ctrl Pts',(-53.5548643992186,-99.6310134108495,
175.985484901707));
#25509=CARTESIAN_POINT('Ctrl Pts',(-53.5449264052387,-99.5377916388449,
174.328630652215));
#25510=CARTESIAN_POINT('Ctrl Pts',(-54.6999600268383,-99.3203761095675,
173.157057825983));
#25511=CARTESIAN_POINT('Ctrl Pts',(-55.8549936484379,-99.10296058029,171.985484999752));
#25512=CARTESIAN_POINT('Ctrl Pts',(-57.4925742726078,-98.834102316693,171.985485069079));
#25513=CARTESIAN_POINT('Ctrl Pts',(-59.1301548967777,-98.5652440530961,
171.985485138407));
#25514=CARTESIAN_POINT('Ctrl Pts',(-60.2851884208854,-98.3478285342118,
173.157058062683));
#25515=CARTESIAN_POINT('Ctrl Pts',(-61.4402219449932,-98.1304130153276,
174.328630986959));
#25516=CARTESIAN_POINT('Ctrl Pts',(-61.430283813139,-98.0371912580215,175.985485236451));
#25517=CARTESIAN_POINT('Ctrl Pts',(-61.4203456812848,-97.9439695007152,
177.642339485944));
#25518=CARTESIAN_POINT('Ctrl Pts',(-60.2454359338512,-97.974941500682,178.813912312176));
#25519=CARTESIAN_POINT('Ctrl Pts',(-59.0705261864175,-98.0059135006488,
179.985485138407));
#25520=CARTESIAN_POINT('Ctrl Pts',(-57.4130694364136,-98.0883282349351,
179.985485069079));
#25521=CARTESIAN_POINT('Ctrl Pts',(-55.7556126864097,-98.1707429692214,
179.985484999752));
#25522=CARTESIAN_POINT('Ctrl Pts',(-54.580703036468,-98.2017149587949,178.813912075476));
#25523=CARTESIAN_POINT('Ctrl Pts',(-56.181115489574,-113.283598570176,178.821287383467));
#25524=CARTESIAN_POINT('Ctrl Pts',(-55.0031681001975,-113.314894403068,
177.646659506339));
#25525=CARTESIAN_POINT('Ctrl Pts',(-54.9932301063974,-113.221672631044,
175.985484901271));
#25526=CARTESIAN_POINT('Ctrl Pts',(-54.9832921125973,-113.12845085902,174.324310296203));
#25527=CARTESIAN_POINT('Ctrl Pts',(-56.1413634738858,-112.910711486397,
173.149682517375));
#25528=CARTESIAN_POINT('Ctrl Pts',(-57.2994348351743,-112.692972113774,
171.975054738546));
#25529=CARTESIAN_POINT('Ctrl Pts',(-58.9413114718314,-112.423655866545,
171.975054808055));
#25530=CARTESIAN_POINT('Ctrl Pts',(-60.5831881084886,-112.154339619316,
171.975054877564));
#25531=CARTESIAN_POINT('Ctrl Pts',(-61.741259372031,-111.936600257113,173.149682754692));
#25532=CARTESIAN_POINT('Ctrl Pts',(-62.8993306355734,-111.71886089491,174.32431063182));
#25533=CARTESIAN_POINT('Ctrl Pts',(-62.8893925035395,-111.625639137623,
175.985485236888));
#25534=CARTESIAN_POINT('Ctrl Pts',(-62.8794543715055,-111.532417380336,
177.646659841956));
#25535=CARTESIAN_POINT('Ctrl Pts',(-61.701506884383,-111.563713223648,178.821287620784));
#25536=CARTESIAN_POINT('Ctrl Pts',(-60.5235593972605,-111.595009066961,
179.995915399612));
#25537=CARTESIAN_POINT('Ctrl Pts',(-58.8618066347693,-111.677881784879,
179.995915330104));
#25538=CARTESIAN_POINT('Ctrl Pts',(-57.2000538722782,-111.760754502798,
179.995915260595));
#25539=CARTESIAN_POINT('Ctrl Pts',(-56.0221064829017,-111.79205033569,178.821287383467));
#25540=CARTESIAN_POINT('Ctrl Pts',(-54.8441590935253,-111.823346168582,
177.646659506339));
#25541=CARTESIAN_POINT('Ctrl Pts',(-54.8342210997252,-111.730124396559,
175.985484901271));
#25542=CARTESIAN_POINT('Ctrl Pts',(-54.8242831059251,-111.636902624535,
174.324310296203));
#25543=CARTESIAN_POINT('Ctrl Pts',(-55.9823544672136,-111.419163251912,
173.149682517375));
#25544=CARTESIAN_POINT('Ctrl Pts',(-57.1404258285021,-111.201423879289,
171.975054738546));
#25545=CARTESIAN_POINT('Ctrl Pts',(-58.7823024651592,-110.932107632059,
171.975054808055));
#25546=CARTESIAN_POINT('Ctrl Pts',(-60.4241791018163,-110.66279138483,171.975054877564));
#25547=CARTESIAN_POINT('Ctrl Pts',(-61.5822503653587,-110.445052022627,
173.149682754692));
#25548=CARTESIAN_POINT('Ctrl Pts',(-62.7403216289012,-110.227312660424,
174.32431063182));
#25549=CARTESIAN_POINT('Ctrl Pts',(-62.7303834968672,-110.134090903137,
175.985485236888));
#25550=CARTESIAN_POINT('Ctrl Pts',(-62.7204453648333,-110.04086914585,177.646659841956));
#25551=CARTESIAN_POINT('Ctrl Pts',(-61.5424978777108,-110.072164989163,
178.821287620784));
#25552=CARTESIAN_POINT('Ctrl Pts',(-60.3645503905882,-110.103460832475,
179.995915399612));
#25553=CARTESIAN_POINT('Ctrl Pts',(-58.7027976280971,-110.186333550394,
179.995915330104));
#25554=CARTESIAN_POINT('Ctrl Pts',(-57.041044865606,-110.269206268313,179.995915260595));
#25555=CARTESIAN_POINT('Ctrl Pts',(-55.8630974762295,-110.300502101205,
178.821287383467));
#25556=CARTESIAN_POINT('Ctrl Pts',(-54.6851500868531,-110.331797934097,
177.646659506339));
#25557=CARTESIAN_POINT('Ctrl Pts',(-54.675212093053,-110.238576162073,175.985484901271));
#25558=CARTESIAN_POINT('Ctrl Pts',(-54.6652740992529,-110.145354390049,
174.324310296203));
#25559=CARTESIAN_POINT('Ctrl Pts',(-55.8233454605414,-109.927615017426,
173.149682517375));
#25560=CARTESIAN_POINT('Ctrl Pts',(-56.9814168218299,-109.709875644803,
171.975054738546));
#25561=CARTESIAN_POINT('Ctrl Pts',(-58.623293458487,-109.440559397574,171.975054808055));
#25562=CARTESIAN_POINT('Ctrl Pts',(-60.2651700951441,-109.171243150344,
171.975054877564));
#25563=CARTESIAN_POINT('Ctrl Pts',(-61.4232413586865,-108.953503788142,
173.149682754692));
#25564=CARTESIAN_POINT('Ctrl Pts',(-62.581312622229,-108.735764425939,174.32431063182));
#25565=CARTESIAN_POINT('Ctrl Pts',(-62.571374490195,-108.642542668652,175.985485236888));
#25566=CARTESIAN_POINT('Ctrl Pts',(-62.5614363581611,-108.549320911365,
177.646659841956));
#25567=CARTESIAN_POINT('Ctrl Pts',(-61.3834888710385,-108.580616754677,
178.821287620784));
#25568=CARTESIAN_POINT('Ctrl Pts',(-60.205541383916,-108.61191259799,179.995915399612));
#25569=CARTESIAN_POINT('Ctrl Pts',(-58.5437886214249,-108.694785315908,
179.995915330104));
#25570=CARTESIAN_POINT('Ctrl Pts',(-56.8820358589338,-108.777658033827,
179.995915260595));
#25571=CARTESIAN_POINT('Ctrl Pts',(-55.7040884695573,-108.808953866719,
178.821287383467));
#25572=CARTESIAN_POINT('Ctrl Pts',(-54.5261410801808,-108.840249699611,
177.646659506339));
#25573=CARTESIAN_POINT('Ctrl Pts',(-54.5162030863807,-108.747027927587,
175.985484901271));
#25574=CARTESIAN_POINT('Ctrl Pts',(-54.5062650925806,-108.653806155564,
174.324310296203));
#25575=CARTESIAN_POINT('Ctrl Pts',(-55.6643364538691,-108.436066782941,
173.149682517375));
#25576=CARTESIAN_POINT('Ctrl Pts',(-56.8224078151577,-108.218327410317,
171.975054738546));
#25577=CARTESIAN_POINT('Ctrl Pts',(-58.4642844518147,-107.949011163088,
171.975054808055));
#25578=CARTESIAN_POINT('Ctrl Pts',(-60.1061610884719,-107.679694915859,
171.975054877564));
#25579=CARTESIAN_POINT('Ctrl Pts',(-61.2642323520143,-107.461955553656,
173.149682754692));
#25580=CARTESIAN_POINT('Ctrl Pts',(-62.4223036155567,-107.244216191453,
174.32431063182));
#25581=CARTESIAN_POINT('Ctrl Pts',(-62.4123654835228,-107.150994434166,
175.985485236888));
#25582=CARTESIAN_POINT('Ctrl Pts',(-62.4024273514889,-107.057772676879,
177.646659841956));
#25583=CARTESIAN_POINT('Ctrl Pts',(-61.2244798643663,-107.089068520192,
178.821287620784));
#25584=CARTESIAN_POINT('Ctrl Pts',(-60.0465323772438,-107.120364363504,
179.995915399612));
#25585=CARTESIAN_POINT('Ctrl Pts',(-58.3847796147526,-107.203237081423,
179.995915330104));
#25586=CARTESIAN_POINT('Ctrl Pts',(-56.7230268522615,-107.286109799341,
179.995915260595));
#25587=CARTESIAN_POINT('Ctrl Pts',(-55.5450794628851,-107.317405632233,
178.821287383467));
#25588=CARTESIAN_POINT('Ctrl Pts',(-54.3671320735086,-107.348701465125,
177.646659506339));
#25589=CARTESIAN_POINT('Ctrl Pts',(-54.3571940797085,-107.255479693102,
175.985484901271));
#25590=CARTESIAN_POINT('Ctrl Pts',(-54.3472560859084,-107.162257921078,
174.324310296203));
#25591=CARTESIAN_POINT('Ctrl Pts',(-55.5053274471969,-106.944518548455,
173.149682517375));
#25592=CARTESIAN_POINT('Ctrl Pts',(-56.6633988084854,-106.726779175832,
171.975054738546));
#25593=CARTESIAN_POINT('Ctrl Pts',(-58.3052754451425,-106.457462928602,
171.975054808055));
#25594=CARTESIAN_POINT('Ctrl Pts',(-59.9471520817997,-106.188146681373,
171.975054877564));
#25595=CARTESIAN_POINT('Ctrl Pts',(-61.1052233453421,-105.97040731917,173.149682754692));
#25596=CARTESIAN_POINT('Ctrl Pts',(-62.2632946088845,-105.752667956968,
174.32431063182));
#25597=CARTESIAN_POINT('Ctrl Pts',(-62.2533564768505,-105.659446199681,
175.985485236888));
#25598=CARTESIAN_POINT('Ctrl Pts',(-62.2434183448166,-105.566224442394,
177.646659841956));
#25599=CARTESIAN_POINT('Ctrl Pts',(-61.0654708576941,-105.597520285706,
178.821287620784));
#25600=CARTESIAN_POINT('Ctrl Pts',(-59.8875233705716,-105.628816129018,
179.995915399612));
#25601=CARTESIAN_POINT('Ctrl Pts',(-58.2257706080804,-105.711688846937,
179.995915330104));
#25602=CARTESIAN_POINT('Ctrl Pts',(-56.5640178455893,-105.794561564856,
179.995915260595));
#25603=CARTESIAN_POINT('Ctrl Pts',(-55.3860704562128,-105.825857397748,
178.821287383467));
#25604=CARTESIAN_POINT('Ctrl Pts',(-54.2081230668364,-105.85715323064,177.646659506339));
#25605=CARTESIAN_POINT('Ctrl Pts',(-54.1981850730363,-105.763931458616,
175.985484901271));
#25606=CARTESIAN_POINT('Ctrl Pts',(-54.1882470792362,-105.670709686593,
174.324310296203));
#25607=CARTESIAN_POINT('Ctrl Pts',(-55.3463184405247,-105.452970313969,
173.149682517375));
#25608=CARTESIAN_POINT('Ctrl Pts',(-56.5043898018132,-105.235230941346,
171.975054738546));
#25609=CARTESIAN_POINT('Ctrl Pts',(-58.1462664384703,-104.965914694117,
171.975054808055));
#25610=CARTESIAN_POINT('Ctrl Pts',(-59.7881430751274,-104.696598446888,
171.975054877564));
#25611=CARTESIAN_POINT('Ctrl Pts',(-60.9462143386698,-104.478859084685,
173.149682754692));
#25612=CARTESIAN_POINT('Ctrl Pts',(-62.1042856022123,-104.261119722482,
174.32431063182));
#25613=CARTESIAN_POINT('Ctrl Pts',(-62.0943474701783,-104.167897965195,
175.985485236888));
#25614=CARTESIAN_POINT('Ctrl Pts',(-62.0844093381444,-104.074676207908,
177.646659841956));
#25615=CARTESIAN_POINT('Ctrl Pts',(-60.9064618510219,-104.10597205122,178.821287620784));
#25616=CARTESIAN_POINT('Ctrl Pts',(-59.7285143638993,-104.137267894533,
179.995915399612));
#25617=CARTESIAN_POINT('Ctrl Pts',(-58.0667616014082,-104.220140612451,
179.995915330104));
#25618=CARTESIAN_POINT('Ctrl Pts',(-56.4050088389171,-104.30301333037,179.995915260595));
#25619=CARTESIAN_POINT('Ctrl Pts',(-55.2270614495406,-104.334309163262,
178.821287383467));
#25620=CARTESIAN_POINT('Ctrl Pts',(-54.0491140601642,-104.365604996154,
177.646659506339));
#25621=CARTESIAN_POINT('Ctrl Pts',(-54.039176066364,-104.272383224131,175.985484901271));
#25622=CARTESIAN_POINT('Ctrl Pts',(-54.029238072564,-104.179161452107,174.324310296203));
#25623=CARTESIAN_POINT('Ctrl Pts',(-55.1873094338524,-103.961422079484,
173.149682517375));
#25624=CARTESIAN_POINT('Ctrl Pts',(-56.345380795141,-103.743682706861,171.975054738546));
#25625=CARTESIAN_POINT('Ctrl Pts',(-57.9872574317981,-103.474366459631,
171.975054808055));
#25626=CARTESIAN_POINT('Ctrl Pts',(-59.6291340684552,-103.205050212402,
171.975054877564));
#25627=CARTESIAN_POINT('Ctrl Pts',(-60.7872053319976,-102.987310850199,
173.149682754692));
#25628=CARTESIAN_POINT('Ctrl Pts',(-61.94527659554,-102.769571487996,174.32431063182));
#25629=CARTESIAN_POINT('Ctrl Pts',(-61.9353384635061,-102.676349730709,
175.985485236888));
#25630=CARTESIAN_POINT('Ctrl Pts',(-61.9254003314722,-102.583127973422,
177.646659841956));
#25631=CARTESIAN_POINT('Ctrl Pts',(-60.7474528443496,-102.614423816735,
178.821287620784));
#25632=CARTESIAN_POINT('Ctrl Pts',(-59.5695053572271,-102.645719660047,
179.995915399612));
#25633=CARTESIAN_POINT('Ctrl Pts',(-57.907752594736,-102.728592377966,179.995915330104));
#25634=CARTESIAN_POINT('Ctrl Pts',(-56.2459998322448,-102.811465095885,
179.995915260595));
#25635=CARTESIAN_POINT('Ctrl Pts',(-55.0680524428684,-102.842760928777,
178.821287383467));
#25636=CARTESIAN_POINT('Ctrl Pts',(-53.8901050534919,-102.874056761669,
177.646659506339));
#25637=CARTESIAN_POINT('Ctrl Pts',(-53.8801670596918,-102.780834989645,
175.985484901271));
#25638=CARTESIAN_POINT('Ctrl Pts',(-53.8702290658917,-102.687613217621,
174.324310296203));
#25639=CARTESIAN_POINT('Ctrl Pts',(-55.0283004271802,-102.469873844998,
173.149682517375));
#25640=CARTESIAN_POINT('Ctrl Pts',(-56.1863717884687,-102.252134472375,
171.975054738546));
#25641=CARTESIAN_POINT('Ctrl Pts',(-57.8282484251258,-101.982818225146,
171.975054808055));
#25642=CARTESIAN_POINT('Ctrl Pts',(-59.470125061783,-101.713501977916,171.975054877564));
#25643=CARTESIAN_POINT('Ctrl Pts',(-60.6281963253254,-101.495762615714,
173.149682754692));
#25644=CARTESIAN_POINT('Ctrl Pts',(-61.7862675888678,-101.278023253511,
174.32431063182));
#25645=CARTESIAN_POINT('Ctrl Pts',(-61.7763294568339,-101.184801496224,
175.985485236888));
#25646=CARTESIAN_POINT('Ctrl Pts',(-61.7663913247999,-101.091579738937,
177.646659841956));
#25647=CARTESIAN_POINT('Ctrl Pts',(-60.5884438376774,-101.122875582249,
178.821287620784));
#25648=CARTESIAN_POINT('Ctrl Pts',(-59.4104963505549,-101.154171425562,
179.995915399612));
#25649=CARTESIAN_POINT('Ctrl Pts',(-57.7487435880637,-101.23704414348,179.995915330104));
#25650=CARTESIAN_POINT('Ctrl Pts',(-56.0869908255726,-101.319916861399,
179.995915260595));
#25651=CARTESIAN_POINT('Ctrl Pts',(-54.9090434361961,-101.351212694291,
178.821287383467));
#25652=CARTESIAN_POINT('Ctrl Pts',(-53.7310960468197,-101.382508527183,
177.646659506339));
#25653=CARTESIAN_POINT('Ctrl Pts',(-53.7211580530196,-101.289286755159,
175.985484901271));
#25654=CARTESIAN_POINT('Ctrl Pts',(-53.7112200592195,-101.196064983136,
174.324310296203));
#25655=CARTESIAN_POINT('Ctrl Pts',(-54.869291420508,-100.978325610513,173.149682517375));
#25656=CARTESIAN_POINT('Ctrl Pts',(-56.0273627817965,-100.760586237889,
171.975054738546));
#25657=CARTESIAN_POINT('Ctrl Pts',(-57.6692394184536,-100.49126999066,171.975054808055));
#25658=CARTESIAN_POINT('Ctrl Pts',(-59.3111160551107,-100.221953743431,
171.975054877564));
#25659=CARTESIAN_POINT('Ctrl Pts',(-60.4691873186531,-100.004214381228,
173.149682754692));
#25660=CARTESIAN_POINT('Ctrl Pts',(-61.6272585821956,-99.7864750190253,
174.32431063182));
#25661=CARTESIAN_POINT('Ctrl Pts',(-61.6173204501616,-99.6932532617382,
175.985485236888));
#25662=CARTESIAN_POINT('Ctrl Pts',(-61.6073823181277,-99.6000315044512,
177.646659841956));
#25663=CARTESIAN_POINT('Ctrl Pts',(-60.4294348310052,-99.6313273477637,
178.821287620784));
#25664=CARTESIAN_POINT('Ctrl Pts',(-59.2514873438827,-99.6626231910761,
179.995915399612));
#25665=CARTESIAN_POINT('Ctrl Pts',(-57.5897345813915,-99.7454959089947,
179.995915330104));
#25666=CARTESIAN_POINT('Ctrl Pts',(-55.9279818189004,-99.8283686269133,
179.995915260595));
#25667=CARTESIAN_POINT('Ctrl Pts',(-54.7500344295239,-99.8596644598054,
178.821287383467));
#25668=CARTESIAN_POINT('Ctrl Pts',(-53.5720870401475,-99.8909602926975,
177.646659506339));
#25669=CARTESIAN_POINT('Ctrl Pts',(-53.5621490463474,-99.7977385206737,
175.985484901271));
#25670=CARTESIAN_POINT('Ctrl Pts',(-53.5522110525473,-99.7045167486501,
174.324310296203));
#25671=CARTESIAN_POINT('Ctrl Pts',(-54.7102824138358,-99.4867773760269,
173.149682517375));
#25672=CARTESIAN_POINT('Ctrl Pts',(-55.8683537751243,-99.2690380034038,
171.975054738546));
#25673=CARTESIAN_POINT('Ctrl Pts',(-57.5102304117814,-98.9997217561745,
171.975054808055));
#25674=CARTESIAN_POINT('Ctrl Pts',(-59.1521070484385,-98.7304055089452,
171.975054877564));
#25675=CARTESIAN_POINT('Ctrl Pts',(-60.3101783119809,-98.5126661467424,
173.149682754692));
#25676=CARTESIAN_POINT('Ctrl Pts',(-61.4682495755234,-98.2949267845397,
174.32431063182));
#25677=CARTESIAN_POINT('Ctrl Pts',(-61.4583114434894,-98.2017050272526,
175.985485236888));
#25678=CARTESIAN_POINT('Ctrl Pts',(-61.4483733114555,-98.1084832699656,
177.646659841956));
#25679=CARTESIAN_POINT('Ctrl Pts',(-60.2704258243329,-98.139779113278,178.821287620784));
#25680=CARTESIAN_POINT('Ctrl Pts',(-59.0924783372104,-98.1710749565905,
179.995915399612));
#25681=CARTESIAN_POINT('Ctrl Pts',(-57.4307255747193,-98.2539476745091,
179.995915330104));
#25682=CARTESIAN_POINT('Ctrl Pts',(-55.7689728122282,-98.3368203924277,
179.995915260595));
#25683=CARTESIAN_POINT('Ctrl Pts',(-54.5910254228517,-98.3681162253198,
178.821287383467));
#25684=CARTESIAN_POINT('Ctrl Pts',(-56.1988062143188,-113.449542435949,
178.821287383467));
#25685=CARTESIAN_POINT('Ctrl Pts',(-55.0208588249424,-113.480838268841,
177.646659506339));
#25686=CARTESIAN_POINT('Ctrl Pts',(-55.0109208311422,-113.387616496817,
175.985484901271));
#25687=CARTESIAN_POINT('Ctrl Pts',(-55.0009828373422,-113.294394724794,
174.324310296203));
#25688=CARTESIAN_POINT('Ctrl Pts',(-56.1590541986307,-113.07665535217,173.149682517375));
#25689=CARTESIAN_POINT('Ctrl Pts',(-57.3171255599192,-112.858915979547,
171.975054738546));
#25690=CARTESIAN_POINT('Ctrl Pts',(-58.9590021965763,-112.589599732318,
171.975054808055));
#25691=CARTESIAN_POINT('Ctrl Pts',(-60.6008788332334,-112.320283485089,
171.975054877564));
#25692=CARTESIAN_POINT('Ctrl Pts',(-61.7589500967758,-112.102544122886,
173.149682754692));
#25693=CARTESIAN_POINT('Ctrl Pts',(-62.9170213603182,-111.884804760683,
174.32431063182));
#25694=CARTESIAN_POINT('Ctrl Pts',(-62.9070832282843,-111.791583003396,
175.985485236888));
#25695=CARTESIAN_POINT('Ctrl Pts',(-62.8971450962504,-111.698361246109,
177.646659841956));
#25696=CARTESIAN_POINT('Ctrl Pts',(-61.7191976091278,-111.729657089422,
178.821287620784));
#25697=CARTESIAN_POINT('Ctrl Pts',(-60.5412501220053,-111.760952932734,
179.995915399612));
#25698=CARTESIAN_POINT('Ctrl Pts',(-58.8794973595142,-111.843825650653,
179.995915330104));
#25699=CARTESIAN_POINT('Ctrl Pts',(-57.217744597023,-111.926698368571,179.995915260595));
#25700=CARTESIAN_POINT('Ctrl Pts',(-56.0397972076466,-111.957994201463,
178.821287383467));
#25701=CARTESIAN_POINT('Ctrl Pts',(-54.8618498182701,-111.989290034355,
177.646659506339));
#25702=CARTESIAN_POINT('Ctrl Pts',(-54.85191182447,-111.896068262332,175.985484901271));
#25703=CARTESIAN_POINT('Ctrl Pts',(-54.8419738306699,-111.802846490308,
174.324310296203));
#25704=CARTESIAN_POINT('Ctrl Pts',(-56.0000451919584,-111.585107117685,
173.149682517375));
#25705=CARTESIAN_POINT('Ctrl Pts',(-57.158116553247,-111.367367745062,171.975054738546));
#25706=CARTESIAN_POINT('Ctrl Pts',(-58.799993189904,-111.098051497832,171.975054808055));
#25707=CARTESIAN_POINT('Ctrl Pts',(-60.4418698265612,-110.828735250603,
171.975054877564));
#25708=CARTESIAN_POINT('Ctrl Pts',(-61.5999410901036,-110.6109958884,173.149682754692));
#25709=CARTESIAN_POINT('Ctrl Pts',(-62.758012353646,-110.393256526198,174.32431063182));
#25710=CARTESIAN_POINT('Ctrl Pts',(-62.7480742216121,-110.30003476891,175.985485236888));
#25711=CARTESIAN_POINT('Ctrl Pts',(-62.7381360895782,-110.206813011623,
177.646659841956));
#25712=CARTESIAN_POINT('Ctrl Pts',(-61.5601886024556,-110.238108854936,
178.821287620784));
#25713=CARTESIAN_POINT('Ctrl Pts',(-60.3822411153331,-110.269404698248,
179.995915399612));
#25714=CARTESIAN_POINT('Ctrl Pts',(-58.7204883528419,-110.352277416167,
179.995915330104));
#25715=CARTESIAN_POINT('Ctrl Pts',(-57.0587355903508,-110.435150134086,
179.995915260595));
#25716=CARTESIAN_POINT('Ctrl Pts',(-55.8807882009743,-110.466445966978,
178.821287383467));
#25717=CARTESIAN_POINT('Ctrl Pts',(-54.7028408115979,-110.49774179987,177.646659506339));
#25718=CARTESIAN_POINT('Ctrl Pts',(-54.6929028177978,-110.404520027846,
175.985484901271));
#25719=CARTESIAN_POINT('Ctrl Pts',(-54.6829648239977,-110.311298255822,
174.324310296203));
#25720=CARTESIAN_POINT('Ctrl Pts',(-55.8410361852862,-110.093558883199,
173.149682517375));
#25721=CARTESIAN_POINT('Ctrl Pts',(-56.9991075465747,-109.875819510576,
171.975054738546));
#25722=CARTESIAN_POINT('Ctrl Pts',(-58.6409841832318,-109.606503263347,
171.975054808055));
#25723=CARTESIAN_POINT('Ctrl Pts',(-60.2828608198889,-109.337187016117,
171.975054877564));
#25724=CARTESIAN_POINT('Ctrl Pts',(-61.4409320834313,-109.119447653915,
173.149682754692));
#25725=CARTESIAN_POINT('Ctrl Pts',(-62.5990033469738,-108.901708291712,
174.32431063182));
#25726=CARTESIAN_POINT('Ctrl Pts',(-62.5890652149398,-108.808486534425,
175.985485236888));
#25727=CARTESIAN_POINT('Ctrl Pts',(-62.5791270829059,-108.715264777138,
177.646659841956));
#25728=CARTESIAN_POINT('Ctrl Pts',(-61.4011795957834,-108.74656062045,178.821287620784));
#25729=CARTESIAN_POINT('Ctrl Pts',(-60.2232321086609,-108.777856463763,
179.995915399612));
#25730=CARTESIAN_POINT('Ctrl Pts',(-58.5614793461697,-108.860729181681,
179.995915330104));
#25731=CARTESIAN_POINT('Ctrl Pts',(-56.8997265836786,-108.9436018996,179.995915260595));
#25732=CARTESIAN_POINT('Ctrl Pts',(-55.7217791943021,-108.974897732492,
178.821287383467));
#25733=CARTESIAN_POINT('Ctrl Pts',(-54.5438318049257,-109.006193565384,
177.646659506339));
#25734=CARTESIAN_POINT('Ctrl Pts',(-54.5338938111256,-108.91297179336,175.985484901271));
#25735=CARTESIAN_POINT('Ctrl Pts',(-54.5239558173255,-108.819750021337,
174.324310296203));
#25736=CARTESIAN_POINT('Ctrl Pts',(-55.682027178614,-108.602010648714,173.149682517375));
#25737=CARTESIAN_POINT('Ctrl Pts',(-56.8400985399025,-108.384271276091,
171.975054738546));
#25738=CARTESIAN_POINT('Ctrl Pts',(-58.4819751765596,-108.114955028861,
171.975054808055));
#25739=CARTESIAN_POINT('Ctrl Pts',(-60.1238518132167,-107.845638781632,
171.975054877564));
#25740=CARTESIAN_POINT('Ctrl Pts',(-61.2819230767591,-107.627899419429,
173.149682754692));
#25741=CARTESIAN_POINT('Ctrl Pts',(-62.4399943403016,-107.410160057226,
174.32431063182));
#25742=CARTESIAN_POINT('Ctrl Pts',(-62.4300562082676,-107.316938299939,
175.985485236888));
#25743=CARTESIAN_POINT('Ctrl Pts',(-62.4201180762337,-107.223716542652,
177.646659841956));
#25744=CARTESIAN_POINT('Ctrl Pts',(-61.2421705891111,-107.255012385965,
178.821287620784));
#25745=CARTESIAN_POINT('Ctrl Pts',(-60.0642231019886,-107.286308229277,
179.995915399612));
#25746=CARTESIAN_POINT('Ctrl Pts',(-58.4024703394975,-107.369180947196,
179.995915330104));
#25747=CARTESIAN_POINT('Ctrl Pts',(-56.7407175770064,-107.452053665114,
179.995915260595));
#25748=CARTESIAN_POINT('Ctrl Pts',(-55.5627701876299,-107.483349498006,
178.821287383467));
#25749=CARTESIAN_POINT('Ctrl Pts',(-54.3848227982534,-107.514645330899,
177.646659506339));
#25750=CARTESIAN_POINT('Ctrl Pts',(-54.3748848044533,-107.421423558875,
175.985484901271));
#25751=CARTESIAN_POINT('Ctrl Pts',(-54.3649468106533,-107.328201786851,
174.324310296203));
#25752=CARTESIAN_POINT('Ctrl Pts',(-55.5230181719417,-107.110462414228,
173.149682517375));
#25753=CARTESIAN_POINT('Ctrl Pts',(-56.6810895332303,-106.892723041605,
171.975054738546));
#25754=CARTESIAN_POINT('Ctrl Pts',(-58.3229661698874,-106.623406794376,
171.975054808055));
#25755=CARTESIAN_POINT('Ctrl Pts',(-59.9648428065445,-106.354090547146,
171.975054877564));
#25756=CARTESIAN_POINT('Ctrl Pts',(-61.1229140700869,-106.136351184943,
173.149682754692));
#25757=CARTESIAN_POINT('Ctrl Pts',(-62.2809853336293,-105.918611822741,
174.32431063182));
#25758=CARTESIAN_POINT('Ctrl Pts',(-62.2710472015954,-105.825390065454,
175.985485236888));
#25759=CARTESIAN_POINT('Ctrl Pts',(-62.2611090695615,-105.732168308167,
177.646659841956));
#25760=CARTESIAN_POINT('Ctrl Pts',(-61.0831615824389,-105.763464151479,
178.821287620784));
#25761=CARTESIAN_POINT('Ctrl Pts',(-59.9052140953164,-105.794759994792,
179.995915399612));
#25762=CARTESIAN_POINT('Ctrl Pts',(-58.2434613328252,-105.87763271271,179.995915330104));
#25763=CARTESIAN_POINT('Ctrl Pts',(-56.5817085703341,-105.960505430629,
179.995915260595));
#25764=CARTESIAN_POINT('Ctrl Pts',(-55.4037611809577,-105.991801263521,
178.821287383467));
#25765=CARTESIAN_POINT('Ctrl Pts',(-54.2258137915812,-106.023097096413,
177.646659506339));
#25766=CARTESIAN_POINT('Ctrl Pts',(-54.2158757977811,-105.929875324389,
175.985484901271));
#25767=CARTESIAN_POINT('Ctrl Pts',(-54.205937803981,-105.836653552366,174.324310296203));
#25768=CARTESIAN_POINT('Ctrl Pts',(-55.3640091652695,-105.618914179742,
173.149682517375));
#25769=CARTESIAN_POINT('Ctrl Pts',(-56.522080526558,-105.401174807119,171.975054738546));
#25770=CARTESIAN_POINT('Ctrl Pts',(-58.1639571632151,-105.13185855989,171.975054808055));
#25771=CARTESIAN_POINT('Ctrl Pts',(-59.8058337998722,-104.862542312661,
171.975054877564));
#25772=CARTESIAN_POINT('Ctrl Pts',(-60.9639050634147,-104.644802950458,
173.149682754692));
#25773=CARTESIAN_POINT('Ctrl Pts',(-62.1219763269571,-104.427063588255,
174.32431063182));
#25774=CARTESIAN_POINT('Ctrl Pts',(-62.1120381949232,-104.333841830968,
175.985485236888));
#25775=CARTESIAN_POINT('Ctrl Pts',(-62.1021000628892,-104.240620073681,
177.646659841956));
#25776=CARTESIAN_POINT('Ctrl Pts',(-60.9241525757667,-104.271915916993,
178.821287620784));
#25777=CARTESIAN_POINT('Ctrl Pts',(-59.7462050886442,-104.303211760306,
179.995915399612));
#25778=CARTESIAN_POINT('Ctrl Pts',(-58.084452326153,-104.386084478225,179.995915330104));
#25779=CARTESIAN_POINT('Ctrl Pts',(-56.4226995636619,-104.468957196143,
179.995915260595));
#25780=CARTESIAN_POINT('Ctrl Pts',(-55.2447521742854,-104.500253029035,
178.821287383467));
#25781=CARTESIAN_POINT('Ctrl Pts',(-54.066804784909,-104.531548861927,177.646659506339));
#25782=CARTESIAN_POINT('Ctrl Pts',(-54.0568667911089,-104.438327089904,
175.985484901271));
#25783=CARTESIAN_POINT('Ctrl Pts',(-54.0469287973088,-104.34510531788,174.324310296203));
#25784=CARTESIAN_POINT('Ctrl Pts',(-55.2050001585973,-104.127365945257,
173.149682517375));
#25785=CARTESIAN_POINT('Ctrl Pts',(-56.3630715198858,-103.909626572634,
171.975054738546));
#25786=CARTESIAN_POINT('Ctrl Pts',(-58.0049481565429,-103.640310325404,
171.975054808055));
#25787=CARTESIAN_POINT('Ctrl Pts',(-59.6468247932,-103.370994078175,171.975054877564));
#25788=CARTESIAN_POINT('Ctrl Pts',(-60.8048960567424,-103.153254715972,
173.149682754692));
#25789=CARTESIAN_POINT('Ctrl Pts',(-61.9629673202849,-102.93551535377,174.32431063182));
#25790=CARTESIAN_POINT('Ctrl Pts',(-61.9530291882509,-102.842293596483,
175.985485236888));
#25791=CARTESIAN_POINT('Ctrl Pts',(-61.943091056217,-102.749071839196,177.646659841956));
#25792=CARTESIAN_POINT('Ctrl Pts',(-60.7651435690945,-102.780367682508,
178.821287620784));
#25793=CARTESIAN_POINT('Ctrl Pts',(-59.587196081972,-102.81166352582,179.995915399612));
#25794=CARTESIAN_POINT('Ctrl Pts',(-57.9254433194808,-102.894536243739,
179.995915330104));
#25795=CARTESIAN_POINT('Ctrl Pts',(-56.2636905569897,-102.977408961658,
179.995915260595));
#25796=CARTESIAN_POINT('Ctrl Pts',(-55.0857431676132,-103.00870479455,178.821287383467));
#25797=CARTESIAN_POINT('Ctrl Pts',(-53.9077957782368,-103.040000627442,
177.646659506339));
#25798=CARTESIAN_POINT('Ctrl Pts',(-53.8978577844367,-102.946778855418,
175.985484901271));
#25799=CARTESIAN_POINT('Ctrl Pts',(-53.8879197906366,-102.853557083394,
174.324310296203));
#25800=CARTESIAN_POINT('Ctrl Pts',(-55.0459911519251,-102.635817710771,
173.149682517375));
#25801=CARTESIAN_POINT('Ctrl Pts',(-56.2040625132136,-102.418078338148,
171.975054738546));
#25802=CARTESIAN_POINT('Ctrl Pts',(-57.8459391498707,-102.148762090919,
171.975054808055));
#25803=CARTESIAN_POINT('Ctrl Pts',(-59.4878157865278,-101.879445843689,
171.975054877564));
#25804=CARTESIAN_POINT('Ctrl Pts',(-60.6458870500702,-101.661706481487,
173.149682754692));
#25805=CARTESIAN_POINT('Ctrl Pts',(-61.8039583136126,-101.443967119284,
174.32431063182));
#25806=CARTESIAN_POINT('Ctrl Pts',(-61.7940201815787,-101.350745361997,
175.985485236888));
#25807=CARTESIAN_POINT('Ctrl Pts',(-61.7840820495448,-101.25752360471,177.646659841956));
#25808=CARTESIAN_POINT('Ctrl Pts',(-60.6061345624222,-101.288819448022,
178.821287620784));
#25809=CARTESIAN_POINT('Ctrl Pts',(-59.4281870752997,-101.320115291335,
179.995915399612));
#25810=CARTESIAN_POINT('Ctrl Pts',(-57.7664343128086,-101.402988009253,
179.995915330104));
#25811=CARTESIAN_POINT('Ctrl Pts',(-56.1046815503175,-101.485860727172,
179.995915260595));
#25812=CARTESIAN_POINT('Ctrl Pts',(-54.926734160941,-101.517156560064,178.821287383467));
#25813=CARTESIAN_POINT('Ctrl Pts',(-53.7487867715645,-101.548452392956,
177.646659506339));
#25814=CARTESIAN_POINT('Ctrl Pts',(-53.7388487777644,-101.455230620932,
175.985484901271));
#25815=CARTESIAN_POINT('Ctrl Pts',(-53.7289107839643,-101.362008848909,
174.324310296203));
#25816=CARTESIAN_POINT('Ctrl Pts',(-54.8869821452528,-101.144269476286,
173.149682517375));
#25817=CARTESIAN_POINT('Ctrl Pts',(-56.0450535065414,-100.926530103662,
171.975054738546));
#25818=CARTESIAN_POINT('Ctrl Pts',(-57.6869301431984,-100.657213856433,
171.975054808055));
#25819=CARTESIAN_POINT('Ctrl Pts',(-59.3288067798556,-100.387897609204,
171.975054877564));
#25820=CARTESIAN_POINT('Ctrl Pts',(-60.486878043398,-100.170158247001,173.149682754692));
#25821=CARTESIAN_POINT('Ctrl Pts',(-61.6449493069404,-99.9524188847983,
174.32431063182));
#25822=CARTESIAN_POINT('Ctrl Pts',(-61.6350111749065,-99.8591971275113,
175.985485236888));
#25823=CARTESIAN_POINT('Ctrl Pts',(-61.6250730428726,-99.7659753702243,
177.646659841956));
#25824=CARTESIAN_POINT('Ctrl Pts',(-60.44712555575,-99.7972712135367,178.821287620784));
#25825=CARTESIAN_POINT('Ctrl Pts',(-59.2691780686275,-99.8285670568492,
179.995915399612));
#25826=CARTESIAN_POINT('Ctrl Pts',(-57.6074253061363,-99.9114397747677,
179.995915330104));
#25827=CARTESIAN_POINT('Ctrl Pts',(-55.9456725436452,-99.9943124926864,
179.995915260595));
#25828=CARTESIAN_POINT('Ctrl Pts',(-54.7677251542687,-100.025608325578,
178.821287383467));
#25829=CARTESIAN_POINT('Ctrl Pts',(-53.5897777648923,-100.05690415847,177.646659506339));
#25830=CARTESIAN_POINT('Ctrl Pts',(-53.5798397710922,-99.9636823864468,
175.985484901271));
#25831=CARTESIAN_POINT('Ctrl Pts',(-53.5699017772921,-99.8704606144232,
174.324310296203));
#25832=CARTESIAN_POINT('Ctrl Pts',(-54.7279731385806,-99.6527212418,173.149682517375));
#25833=CARTESIAN_POINT('Ctrl Pts',(-55.8860444998691,-99.4349818691769,
171.975054738546));
#25834=CARTESIAN_POINT('Ctrl Pts',(-57.5279211365262,-99.1656656219475,
171.975054808055));
#25835=CARTESIAN_POINT('Ctrl Pts',(-59.1697977731833,-98.8963493747183,
171.975054877564));
#25836=CARTESIAN_POINT('Ctrl Pts',(-60.3278690367257,-98.6786100125155,
173.149682754692));
#25837=CARTESIAN_POINT('Ctrl Pts',(-61.4859403002682,-98.4608706503128,
174.32431063182));
#25838=CARTESIAN_POINT('Ctrl Pts',(-61.4760021682342,-98.3676488930257,
175.985485236888));
#25839=CARTESIAN_POINT('Ctrl Pts',(-61.4660640362003,-98.2744271357387,
177.646659841956));
#25840=CARTESIAN_POINT('Ctrl Pts',(-60.2881165490778,-98.3057229790511,
178.821287620784));
#25841=CARTESIAN_POINT('Ctrl Pts',(-59.1101690619552,-98.3370188223636,
179.995915399612));
#25842=CARTESIAN_POINT('Ctrl Pts',(-57.4484162994641,-98.4198915402821,
179.995915330104));
#25843=CARTESIAN_POINT('Ctrl Pts',(-55.786663536973,-98.5027642582008,179.995915260595));
#25844=CARTESIAN_POINT('Ctrl Pts',(-54.6087161475965,-98.5340600910929,
178.821287383467));
#25845=CARTESIAN_POINT('Ctrl Pts',(-56.2237961054143,-113.614380048479,
178.813912075476));
#25846=CARTESIAN_POINT('Ctrl Pts',(-55.0488864554725,-113.645352038053,
177.6423391512));
#25847=CARTESIAN_POINT('Ctrl Pts',(-55.0389484614927,-113.552130266048,
175.985484901707));
#25848=CARTESIAN_POINT('Ctrl Pts',(-55.0290104675128,-113.458908494044,
174.328630652215));
#25849=CARTESIAN_POINT('Ctrl Pts',(-56.1840440891124,-113.241492964766,
173.157057825983));
#25850=CARTESIAN_POINT('Ctrl Pts',(-57.3390777107121,-113.024077435489,
171.985484999752));
#25851=CARTESIAN_POINT('Ctrl Pts',(-58.9766583348819,-112.755219171892,
171.985485069079));
#25852=CARTESIAN_POINT('Ctrl Pts',(-60.6142389590518,-112.486360908295,
171.985485138407));
#25853=CARTESIAN_POINT('Ctrl Pts',(-61.7692724831595,-112.268945389411,
173.157058062683));
#25854=CARTESIAN_POINT('Ctrl Pts',(-62.9243060072673,-112.051529870527,
174.328630986959));
#25855=CARTESIAN_POINT('Ctrl Pts',(-62.9143678754131,-111.95830811322,175.985485236451));
#25856=CARTESIAN_POINT('Ctrl Pts',(-62.9044297435589,-111.865086355914,
177.642339485944));
#25857=CARTESIAN_POINT('Ctrl Pts',(-61.7295199961253,-111.896058355881,
178.813912312176));
#25858=CARTESIAN_POINT('Ctrl Pts',(-60.5546102486917,-111.927030355848,
179.985485138407));
#25859=CARTESIAN_POINT('Ctrl Pts',(-58.8971534986878,-112.009445090134,
179.985485069079));
#25860=CARTESIAN_POINT('Ctrl Pts',(-57.2396967486839,-112.09185982442,179.985484999752));
#25861=CARTESIAN_POINT('Ctrl Pts',(-56.0647870987421,-112.122831813994,
178.813912075476));
#25862=CARTESIAN_POINT('Ctrl Pts',(-54.8898774488003,-112.153803803567,
177.6423391512));
#25863=CARTESIAN_POINT('Ctrl Pts',(-54.8799394548205,-112.060582031563,
175.985484901707));
#25864=CARTESIAN_POINT('Ctrl Pts',(-54.8700014608406,-111.967360259558,
174.328630652215));
#25865=CARTESIAN_POINT('Ctrl Pts',(-56.0250350824402,-111.749944730281,
173.157057825983));
#25866=CARTESIAN_POINT('Ctrl Pts',(-57.1800687040398,-111.532529201003,
171.985484999752));
#25867=CARTESIAN_POINT('Ctrl Pts',(-58.8176493282097,-111.263670937406,
171.985485069079));
#25868=CARTESIAN_POINT('Ctrl Pts',(-60.4552299523796,-110.994812673809,
171.985485138407));
#25869=CARTESIAN_POINT('Ctrl Pts',(-61.6102634764873,-110.777397154925,
173.157058062683));
#25870=CARTESIAN_POINT('Ctrl Pts',(-62.7652970005951,-110.559981636041,
174.328630986959));
#25871=CARTESIAN_POINT('Ctrl Pts',(-62.7553588687409,-110.466759878735,
175.985485236451));
#25872=CARTESIAN_POINT('Ctrl Pts',(-62.7454207368867,-110.373538121429,
177.642339485944));
#25873=CARTESIAN_POINT('Ctrl Pts',(-61.5705109894531,-110.404510121395,
178.813912312176));
#25874=CARTESIAN_POINT('Ctrl Pts',(-60.3956012420194,-110.435482121362,
179.985485138407));
#25875=CARTESIAN_POINT('Ctrl Pts',(-58.7381444920155,-110.517896855648,
179.985485069079));
#25876=CARTESIAN_POINT('Ctrl Pts',(-57.0806877420116,-110.600311589935,
179.985484999752));
#25877=CARTESIAN_POINT('Ctrl Pts',(-55.9057780920699,-110.631283579508,
178.813912075476));
#25878=CARTESIAN_POINT('Ctrl Pts',(-54.7308684421281,-110.662255569082,
177.6423391512));
#25879=CARTESIAN_POINT('Ctrl Pts',(-54.7209304481482,-110.569033797077,
175.985484901707));
#25880=CARTESIAN_POINT('Ctrl Pts',(-54.7109924541684,-110.475812025073,
174.328630652215));
#25881=CARTESIAN_POINT('Ctrl Pts',(-55.866026075768,-110.258396495795,173.157057825983));
#25882=CARTESIAN_POINT('Ctrl Pts',(-57.0210596973676,-110.040980966518,
171.985484999752));
#25883=CARTESIAN_POINT('Ctrl Pts',(-58.6586403215375,-109.772122702921,
171.985485069079));
#25884=CARTESIAN_POINT('Ctrl Pts',(-60.2962209457073,-109.503264439324,
171.985485138407));
#25885=CARTESIAN_POINT('Ctrl Pts',(-61.4512544698151,-109.28584892044,173.157058062683));
#25886=CARTESIAN_POINT('Ctrl Pts',(-62.6062879939228,-109.068433401555,
174.328630986959));
#25887=CARTESIAN_POINT('Ctrl Pts',(-62.5963498620687,-108.975211644249,
175.985485236451));
#25888=CARTESIAN_POINT('Ctrl Pts',(-62.5864117302145,-108.881989886943,
177.642339485944));
#25889=CARTESIAN_POINT('Ctrl Pts',(-61.4115019827808,-108.91296188691,178.813912312176));
#25890=CARTESIAN_POINT('Ctrl Pts',(-60.2365922353472,-108.943933886877,
179.985485138407));
#25891=CARTESIAN_POINT('Ctrl Pts',(-58.5791354853433,-109.026348621163,
179.985485069079));
#25892=CARTESIAN_POINT('Ctrl Pts',(-56.9216787353394,-109.108763355449,
179.985484999752));
#25893=CARTESIAN_POINT('Ctrl Pts',(-55.7467690853976,-109.139735345023,
178.813912075476));
#25894=CARTESIAN_POINT('Ctrl Pts',(-54.5718594354559,-109.170707334596,
177.6423391512));
#25895=CARTESIAN_POINT('Ctrl Pts',(-54.561921441476,-109.077485562592,175.985484901707));
#25896=CARTESIAN_POINT('Ctrl Pts',(-54.5519834474962,-108.984263790587,
174.328630652215));
#25897=CARTESIAN_POINT('Ctrl Pts',(-55.7070170690958,-108.76684826131,173.157057825983));
#25898=CARTESIAN_POINT('Ctrl Pts',(-56.8620506906954,-108.549432732032,
171.985484999752));
#25899=CARTESIAN_POINT('Ctrl Pts',(-58.4996313148652,-108.280574468435,
171.985485069079));
#25900=CARTESIAN_POINT('Ctrl Pts',(-60.1372119390351,-108.011716204838,
171.985485138407));
#25901=CARTESIAN_POINT('Ctrl Pts',(-61.2922454631428,-107.794300685954,
173.157058062683));
#25902=CARTESIAN_POINT('Ctrl Pts',(-62.4472789872506,-107.57688516707,174.328630986959));
#25903=CARTESIAN_POINT('Ctrl Pts',(-62.4373408553964,-107.483663409764,
175.985485236451));
#25904=CARTESIAN_POINT('Ctrl Pts',(-62.4274027235423,-107.390441652457,
177.642339485944));
#25905=CARTESIAN_POINT('Ctrl Pts',(-61.2524929761086,-107.421413652424,
178.813912312176));
#25906=CARTESIAN_POINT('Ctrl Pts',(-60.077583228675,-107.452385652391,179.985485138407));
#25907=CARTESIAN_POINT('Ctrl Pts',(-58.4201264786711,-107.534800386677,
179.985485069079));
#25908=CARTESIAN_POINT('Ctrl Pts',(-56.7626697286672,-107.617215120964,
179.985484999752));
#25909=CARTESIAN_POINT('Ctrl Pts',(-55.5877600787254,-107.648187110537,
178.813912075476));
#25910=CARTESIAN_POINT('Ctrl Pts',(-54.4128504287836,-107.67915910011,177.6423391512));
#25911=CARTESIAN_POINT('Ctrl Pts',(-54.4029124348038,-107.585937328106,
175.985484901707));
#25912=CARTESIAN_POINT('Ctrl Pts',(-54.3929744408239,-107.492715556102,
174.328630652215));
#25913=CARTESIAN_POINT('Ctrl Pts',(-55.5480080624235,-107.275300026824,
173.157057825983));
#25914=CARTESIAN_POINT('Ctrl Pts',(-56.7030416840231,-107.057884497547,
171.985484999752));
#25915=CARTESIAN_POINT('Ctrl Pts',(-58.340622308193,-106.78902623395,171.985485069079));
#25916=CARTESIAN_POINT('Ctrl Pts',(-59.9782029323629,-106.520167970353,
171.985485138407));
#25917=CARTESIAN_POINT('Ctrl Pts',(-61.1332364564706,-106.302752451468,
173.157058062683));
#25918=CARTESIAN_POINT('Ctrl Pts',(-62.2882699805784,-106.085336932584,
174.328630986959));
#25919=CARTESIAN_POINT('Ctrl Pts',(-62.2783318487242,-105.992115175278,
175.985485236451));
#25920=CARTESIAN_POINT('Ctrl Pts',(-62.26839371687,-105.898893417972,177.642339485944));
#25921=CARTESIAN_POINT('Ctrl Pts',(-61.0934839694364,-105.929865417939,
178.813912312176));
#25922=CARTESIAN_POINT('Ctrl Pts',(-59.9185742220028,-105.960837417905,
179.985485138407));
#25923=CARTESIAN_POINT('Ctrl Pts',(-58.2611174719989,-106.043252152192,
179.985485069079));
#25924=CARTESIAN_POINT('Ctrl Pts',(-56.603660721995,-106.125666886478,179.985484999752));
#25925=CARTESIAN_POINT('Ctrl Pts',(-55.4287510720532,-106.156638876051,
178.813912075476));
#25926=CARTESIAN_POINT('Ctrl Pts',(-54.2538414221114,-106.187610865625,
177.6423391512));
#25927=CARTESIAN_POINT('Ctrl Pts',(-54.2439034281315,-106.09438909362,175.985484901707));
#25928=CARTESIAN_POINT('Ctrl Pts',(-54.2339654341517,-106.001167321616,
174.328630652215));
#25929=CARTESIAN_POINT('Ctrl Pts',(-55.3889990557513,-105.783751792338,
173.157057825983));
#25930=CARTESIAN_POINT('Ctrl Pts',(-56.5440326773509,-105.566336263061,
171.985484999752));
#25931=CARTESIAN_POINT('Ctrl Pts',(-58.1816133015208,-105.297477999464,
171.985485069079));
#25932=CARTESIAN_POINT('Ctrl Pts',(-59.8191939256906,-105.028619735867,
171.985485138407));
#25933=CARTESIAN_POINT('Ctrl Pts',(-60.9742274497984,-104.811204216983,
173.157058062683));
#25934=CARTESIAN_POINT('Ctrl Pts',(-62.1292609739061,-104.593788698099,
174.328630986959));
#25935=CARTESIAN_POINT('Ctrl Pts',(-62.119322842052,-104.500566940792,175.985485236451));
#25936=CARTESIAN_POINT('Ctrl Pts',(-62.1093847101978,-104.407345183486,
177.642339485944));
#25937=CARTESIAN_POINT('Ctrl Pts',(-60.9344749627642,-104.438317183453,
178.813912312176));
#25938=CARTESIAN_POINT('Ctrl Pts',(-59.7595652153305,-104.46928918342,179.985485138407));
#25939=CARTESIAN_POINT('Ctrl Pts',(-58.1021084653266,-104.551703917706,
179.985485069079));
#25940=CARTESIAN_POINT('Ctrl Pts',(-56.4446517153227,-104.634118651992,
179.985484999752));
#25941=CARTESIAN_POINT('Ctrl Pts',(-55.269742065381,-104.665090641566,178.813912075476));
#25942=CARTESIAN_POINT('Ctrl Pts',(-54.0948324154392,-104.696062631139,
177.6423391512));
#25943=CARTESIAN_POINT('Ctrl Pts',(-54.0848944214593,-104.602840859135,
175.985484901707));
#25944=CARTESIAN_POINT('Ctrl Pts',(-54.0749564274795,-104.50961908713,174.328630652215));
#25945=CARTESIAN_POINT('Ctrl Pts',(-55.2299900490791,-104.292203557853,
173.157057825983));
#25946=CARTESIAN_POINT('Ctrl Pts',(-56.3850236706787,-104.074788028575,
171.985484999752));
#25947=CARTESIAN_POINT('Ctrl Pts',(-58.0226042948486,-103.805929764978,
171.985485069079));
#25948=CARTESIAN_POINT('Ctrl Pts',(-59.6601849190184,-103.537071501381,
171.985485138407));
#25949=CARTESIAN_POINT('Ctrl Pts',(-60.8152184431262,-103.319655982497,
173.157058062683));
#25950=CARTESIAN_POINT('Ctrl Pts',(-61.9702519672339,-103.102240463613,
174.328630986959));
#25951=CARTESIAN_POINT('Ctrl Pts',(-61.9603138353797,-103.009018706307,
175.985485236451));
#25952=CARTESIAN_POINT('Ctrl Pts',(-61.9503757035256,-102.915796949001,
177.642339485944));
#25953=CARTESIAN_POINT('Ctrl Pts',(-60.7754659560919,-102.946768948967,
178.813912312176));
#25954=CARTESIAN_POINT('Ctrl Pts',(-59.6005562086583,-102.977740948934,
179.985485138407));
#25955=CARTESIAN_POINT('Ctrl Pts',(-57.9430994586544,-103.06015568322,179.985485069079));
#25956=CARTESIAN_POINT('Ctrl Pts',(-56.2856427086505,-103.142570417507,
179.985484999752));
#25957=CARTESIAN_POINT('Ctrl Pts',(-55.1107330587087,-103.17354240708,178.813912075476));
#25958=CARTESIAN_POINT('Ctrl Pts',(-53.935823408767,-103.204514396654,177.6423391512));
#25959=CARTESIAN_POINT('Ctrl Pts',(-53.9258854147871,-103.111292624649,
175.985484901707));
#25960=CARTESIAN_POINT('Ctrl Pts',(-53.9159474208072,-103.018070852645,
174.328630652215));
#25961=CARTESIAN_POINT('Ctrl Pts',(-55.0709810424069,-102.800655323367,
173.157057825983));
#25962=CARTESIAN_POINT('Ctrl Pts',(-56.2260146640065,-102.58323979409,171.985484999752));
#25963=CARTESIAN_POINT('Ctrl Pts',(-57.8635952881763,-102.314381530493,
171.985485069079));
#25964=CARTESIAN_POINT('Ctrl Pts',(-59.5011759123462,-102.045523266896,
171.985485138407));
#25965=CARTESIAN_POINT('Ctrl Pts',(-60.6562094364539,-101.828107748012,
173.157058062683));
#25966=CARTESIAN_POINT('Ctrl Pts',(-61.8112429605617,-101.610692229127,
174.328630986959));
#25967=CARTESIAN_POINT('Ctrl Pts',(-61.8013048287075,-101.517470471821,
175.985485236451));
#25968=CARTESIAN_POINT('Ctrl Pts',(-61.7913666968533,-101.424248714515,
177.642339485944));
#25969=CARTESIAN_POINT('Ctrl Pts',(-60.6164569494197,-101.455220714482,
178.813912312176));
#25970=CARTESIAN_POINT('Ctrl Pts',(-59.4415472019861,-101.486192714449,
179.985485138407));
#25971=CARTESIAN_POINT('Ctrl Pts',(-57.7840904519822,-101.568607448735,
179.985485069079));
#25972=CARTESIAN_POINT('Ctrl Pts',(-56.1266337019783,-101.651022183021,
179.985484999752));
#25973=CARTESIAN_POINT('Ctrl Pts',(-54.9517240520365,-101.681994172595,
178.813912075476));
#25974=CARTESIAN_POINT('Ctrl Pts',(-53.7768144020947,-101.712966162168,
177.6423391512));
#25975=CARTESIAN_POINT('Ctrl Pts',(-53.7668764081149,-101.619744390164,
175.985484901707));
#25976=CARTESIAN_POINT('Ctrl Pts',(-53.756938414135,-101.526522618159,174.328630652215));
#25977=CARTESIAN_POINT('Ctrl Pts',(-54.9119720357346,-101.309107088882,
173.157057825983));
#25978=CARTESIAN_POINT('Ctrl Pts',(-56.0670056573342,-101.091691559604,
171.985484999752));
#25979=CARTESIAN_POINT('Ctrl Pts',(-57.7045862815041,-100.822833296007,
171.985485069079));
#25980=CARTESIAN_POINT('Ctrl Pts',(-59.342166905674,-100.55397503241,171.985485138407));
#25981=CARTESIAN_POINT('Ctrl Pts',(-60.4972004297817,-100.336559513526,
173.157058062683));
#25982=CARTESIAN_POINT('Ctrl Pts',(-61.6522339538895,-100.119143994642,
174.328630986959));
#25983=CARTESIAN_POINT('Ctrl Pts',(-61.6422958220353,-100.025922237336,
175.985485236451));
#25984=CARTESIAN_POINT('Ctrl Pts',(-61.6323576901811,-99.9327004800294,
177.642339485944));
#25985=CARTESIAN_POINT('Ctrl Pts',(-60.4574479427475,-99.9636724799962,
178.813912312176));
#25986=CARTESIAN_POINT('Ctrl Pts',(-59.2825381953138,-99.994644479963,179.985485138407));
#25987=CARTESIAN_POINT('Ctrl Pts',(-57.6250814453099,-100.077059214249,
179.985485069079));
#25988=CARTESIAN_POINT('Ctrl Pts',(-55.9676246953061,-100.159473948536,
179.985484999752));
#25989=CARTESIAN_POINT('Ctrl Pts',(-54.7927150453643,-100.190445938109,
178.813912075476));
#25990=CARTESIAN_POINT('Ctrl Pts',(-53.6178053954225,-100.221417927683,
177.6423391512));
#25991=CARTESIAN_POINT('Ctrl Pts',(-53.6078674014426,-100.128196155678,
175.985484901707));
#25992=CARTESIAN_POINT('Ctrl Pts',(-53.5979294074628,-100.034974383673,
174.328630652215));
#25993=CARTESIAN_POINT('Ctrl Pts',(-54.7529630290624,-99.817558854396,173.157057825983));
#25994=CARTESIAN_POINT('Ctrl Pts',(-55.907996650662,-99.6001433251185,171.985484999752));
#25995=CARTESIAN_POINT('Ctrl Pts',(-57.5455772748319,-99.3312850615215,
171.985485069079));
#25996=CARTESIAN_POINT('Ctrl Pts',(-59.1831578990017,-99.0624267979246,
171.985485138407));
#25997=CARTESIAN_POINT('Ctrl Pts',(-60.3381914231095,-98.8450112790404,
173.157058062683));
#25998=CARTESIAN_POINT('Ctrl Pts',(-61.4932249472172,-98.6275957601562,
174.328630986959));
#25999=CARTESIAN_POINT('Ctrl Pts',(-61.4832868153631,-98.53437400285,175.985485236451));
#26000=CARTESIAN_POINT('Ctrl Pts',(-61.4733486835089,-98.4411522455438,
177.642339485944));
#26001=CARTESIAN_POINT('Ctrl Pts',(-60.2984389360752,-98.4721242455106,
178.813912312176));
#26002=CARTESIAN_POINT('Ctrl Pts',(-59.1235291886416,-98.5030962454774,
179.985485138407));
#26003=CARTESIAN_POINT('Ctrl Pts',(-57.4660724386377,-98.5855109797636,
179.985485069079));
#26004=CARTESIAN_POINT('Ctrl Pts',(-55.8086156886338,-98.6679257140499,
179.985484999752));
#26005=CARTESIAN_POINT('Ctrl Pts',(-54.633706038692,-98.6988977036234,178.813912075476));
#26006=CARTESIAN_POINT('Ctrl Pts',(-56.2237961054143,-113.614380048479,
178.813912075476));
#26007=CARTESIAN_POINT('Ctrl Pts',(-55.0488864554725,-113.645352038053,
177.6423391512));
#26008=CARTESIAN_POINT('Ctrl Pts',(-55.0389484614927,-113.552130266048,
175.985484901707));
#26009=CARTESIAN_POINT('Ctrl Pts',(-55.0290104675128,-113.458908494044,
174.328630652215));
#26010=CARTESIAN_POINT('Ctrl Pts',(-56.1840440891124,-113.241492964766,
173.157057825983));
#26011=CARTESIAN_POINT('Ctrl Pts',(-57.3390777107121,-113.024077435489,
171.985484999752));
#26012=CARTESIAN_POINT('Ctrl Pts',(-58.9766583348819,-112.755219171892,
171.985485069079));
#26013=CARTESIAN_POINT('Ctrl Pts',(-60.6142389590518,-112.486360908295,
171.985485138407));
#26014=CARTESIAN_POINT('Ctrl Pts',(-61.7692724831595,-112.268945389411,
173.157058062683));
#26015=CARTESIAN_POINT('Ctrl Pts',(-62.9243060072673,-112.051529870527,
174.328630986959));
#26016=CARTESIAN_POINT('Ctrl Pts',(-62.9143678754131,-111.95830811322,175.985485236451));
#26017=CARTESIAN_POINT('Ctrl Pts',(-62.9044297435589,-111.865086355914,
177.642339485944));
#26018=CARTESIAN_POINT('Ctrl Pts',(-61.7295199961253,-111.896058355881,
178.813912312176));
#26019=CARTESIAN_POINT('Ctrl Pts',(-60.5546102486917,-111.927030355848,
179.985485138407));
#26020=CARTESIAN_POINT('Ctrl Pts',(-58.8971534986878,-112.009445090134,
179.985485069079));
#26021=CARTESIAN_POINT('Ctrl Pts',(-57.2396967486839,-112.09185982442,179.985484999752));
#26022=CARTESIAN_POINT('Ctrl Pts',(-56.0647870987421,-112.122831813994,
178.813912075476));
#26023=CARTESIAN_POINT('Ctrl Pts',(-54.8898774488003,-112.153803803567,
177.6423391512));
#26024=CARTESIAN_POINT('Ctrl Pts',(-54.8799394548205,-112.060582031563,
175.985484901707));
#26025=CARTESIAN_POINT('Ctrl Pts',(-54.8700014608406,-111.967360259558,
174.328630652215));
#26026=CARTESIAN_POINT('Ctrl Pts',(-56.0250350824402,-111.749944730281,
173.157057825983));
#26027=CARTESIAN_POINT('Ctrl Pts',(-57.1800687040398,-111.532529201003,
171.985484999752));
#26028=CARTESIAN_POINT('Ctrl Pts',(-58.8176493282097,-111.263670937406,
171.985485069079));
#26029=CARTESIAN_POINT('Ctrl Pts',(-60.4552299523796,-110.994812673809,
171.985485138407));
#26030=CARTESIAN_POINT('Ctrl Pts',(-61.6102634764873,-110.777397154925,
173.157058062683));
#26031=CARTESIAN_POINT('Ctrl Pts',(-62.7652970005951,-110.559981636041,
174.328630986959));
#26032=CARTESIAN_POINT('Ctrl Pts',(-62.7553588687409,-110.466759878735,
175.985485236451));
#26033=CARTESIAN_POINT('Ctrl Pts',(-62.7454207368867,-110.373538121429,
177.642339485944));
#26034=CARTESIAN_POINT('Ctrl Pts',(-61.5705109894531,-110.404510121395,
178.813912312176));
#26035=CARTESIAN_POINT('Ctrl Pts',(-60.3956012420194,-110.435482121362,
179.985485138407));
#26036=CARTESIAN_POINT('Ctrl Pts',(-58.7381444920155,-110.517896855648,
179.985485069079));
#26037=CARTESIAN_POINT('Ctrl Pts',(-57.0806877420116,-110.600311589935,
179.985484999752));
#26038=CARTESIAN_POINT('Ctrl Pts',(-55.9057780920699,-110.631283579508,
178.813912075476));
#26039=CARTESIAN_POINT('Ctrl Pts',(-54.7308684421281,-110.662255569082,
177.6423391512));
#26040=CARTESIAN_POINT('Ctrl Pts',(-54.7209304481482,-110.569033797077,
175.985484901707));
#26041=CARTESIAN_POINT('Ctrl Pts',(-54.7109924541684,-110.475812025073,
174.328630652215));
#26042=CARTESIAN_POINT('Ctrl Pts',(-55.866026075768,-110.258396495795,173.157057825983));
#26043=CARTESIAN_POINT('Ctrl Pts',(-57.0210596973676,-110.040980966518,
171.985484999752));
#26044=CARTESIAN_POINT('Ctrl Pts',(-58.6586403215375,-109.772122702921,
171.985485069079));
#26045=CARTESIAN_POINT('Ctrl Pts',(-60.2962209457073,-109.503264439324,
171.985485138407));
#26046=CARTESIAN_POINT('Ctrl Pts',(-61.4512544698151,-109.28584892044,173.157058062683));
#26047=CARTESIAN_POINT('Ctrl Pts',(-62.6062879939228,-109.068433401555,
174.328630986959));
#26048=CARTESIAN_POINT('Ctrl Pts',(-62.5963498620687,-108.975211644249,
175.985485236451));
#26049=CARTESIAN_POINT('Ctrl Pts',(-62.5864117302145,-108.881989886943,
177.642339485944));
#26050=CARTESIAN_POINT('Ctrl Pts',(-61.4115019827808,-108.91296188691,178.813912312176));
#26051=CARTESIAN_POINT('Ctrl Pts',(-60.2365922353472,-108.943933886877,
179.985485138407));
#26052=CARTESIAN_POINT('Ctrl Pts',(-58.5791354853433,-109.026348621163,
179.985485069079));
#26053=CARTESIAN_POINT('Ctrl Pts',(-56.9216787353394,-109.108763355449,
179.985484999752));
#26054=CARTESIAN_POINT('Ctrl Pts',(-55.7467690853976,-109.139735345023,
178.813912075476));
#26055=CARTESIAN_POINT('Ctrl Pts',(-54.5718594354559,-109.170707334596,
177.6423391512));
#26056=CARTESIAN_POINT('Ctrl Pts',(-54.561921441476,-109.077485562592,175.985484901707));
#26057=CARTESIAN_POINT('Ctrl Pts',(-54.5519834474962,-108.984263790587,
174.328630652215));
#26058=CARTESIAN_POINT('Ctrl Pts',(-55.7070170690958,-108.76684826131,173.157057825983));
#26059=CARTESIAN_POINT('Ctrl Pts',(-56.8620506906954,-108.549432732032,
171.985484999752));
#26060=CARTESIAN_POINT('Ctrl Pts',(-58.4996313148652,-108.280574468435,
171.985485069079));
#26061=CARTESIAN_POINT('Ctrl Pts',(-60.1372119390351,-108.011716204838,
171.985485138407));
#26062=CARTESIAN_POINT('Ctrl Pts',(-61.2922454631428,-107.794300685954,
173.157058062683));
#26063=CARTESIAN_POINT('Ctrl Pts',(-62.4472789872506,-107.57688516707,174.328630986959));
#26064=CARTESIAN_POINT('Ctrl Pts',(-62.4373408553964,-107.483663409764,
175.985485236451));
#26065=CARTESIAN_POINT('Ctrl Pts',(-62.4274027235423,-107.390441652457,
177.642339485944));
#26066=CARTESIAN_POINT('Ctrl Pts',(-61.2524929761086,-107.421413652424,
178.813912312176));
#26067=CARTESIAN_POINT('Ctrl Pts',(-60.077583228675,-107.452385652391,179.985485138407));
#26068=CARTESIAN_POINT('Ctrl Pts',(-58.4201264786711,-107.534800386677,
179.985485069079));
#26069=CARTESIAN_POINT('Ctrl Pts',(-56.7626697286672,-107.617215120964,
179.985484999752));
#26070=CARTESIAN_POINT('Ctrl Pts',(-55.5877600787254,-107.648187110537,
178.813912075476));
#26071=CARTESIAN_POINT('Ctrl Pts',(-54.4128504287836,-107.67915910011,177.6423391512));
#26072=CARTESIAN_POINT('Ctrl Pts',(-54.4029124348038,-107.585937328106,
175.985484901707));
#26073=CARTESIAN_POINT('Ctrl Pts',(-54.3929744408239,-107.492715556102,
174.328630652215));
#26074=CARTESIAN_POINT('Ctrl Pts',(-55.5480080624235,-107.275300026824,
173.157057825983));
#26075=CARTESIAN_POINT('Ctrl Pts',(-56.7030416840231,-107.057884497547,
171.985484999752));
#26076=CARTESIAN_POINT('Ctrl Pts',(-58.340622308193,-106.78902623395,171.985485069079));
#26077=CARTESIAN_POINT('Ctrl Pts',(-59.9782029323629,-106.520167970353,
171.985485138407));
#26078=CARTESIAN_POINT('Ctrl Pts',(-61.1332364564706,-106.302752451468,
173.157058062683));
#26079=CARTESIAN_POINT('Ctrl Pts',(-62.2882699805784,-106.085336932584,
174.328630986959));
#26080=CARTESIAN_POINT('Ctrl Pts',(-62.2783318487242,-105.992115175278,
175.985485236451));
#26081=CARTESIAN_POINT('Ctrl Pts',(-62.26839371687,-105.898893417972,177.642339485944));
#26082=CARTESIAN_POINT('Ctrl Pts',(-61.0934839694364,-105.929865417939,
178.813912312176));
#26083=CARTESIAN_POINT('Ctrl Pts',(-59.9185742220028,-105.960837417905,
179.985485138407));
#26084=CARTESIAN_POINT('Ctrl Pts',(-58.2611174719989,-106.043252152192,
179.985485069079));
#26085=CARTESIAN_POINT('Ctrl Pts',(-56.603660721995,-106.125666886478,179.985484999752));
#26086=CARTESIAN_POINT('Ctrl Pts',(-55.4287510720532,-106.156638876051,
178.813912075476));
#26087=CARTESIAN_POINT('Ctrl Pts',(-54.2538414221114,-106.187610865625,
177.6423391512));
#26088=CARTESIAN_POINT('Ctrl Pts',(-54.2439034281315,-106.09438909362,175.985484901707));
#26089=CARTESIAN_POINT('Ctrl Pts',(-54.2339654341517,-106.001167321616,
174.328630652215));
#26090=CARTESIAN_POINT('Ctrl Pts',(-55.3889990557513,-105.783751792338,
173.157057825983));
#26091=CARTESIAN_POINT('Ctrl Pts',(-56.5440326773509,-105.566336263061,
171.985484999752));
#26092=CARTESIAN_POINT('Ctrl Pts',(-58.1816133015208,-105.297477999464,
171.985485069079));
#26093=CARTESIAN_POINT('Ctrl Pts',(-59.8191939256906,-105.028619735867,
171.985485138407));
#26094=CARTESIAN_POINT('Ctrl Pts',(-60.9742274497984,-104.811204216983,
173.157058062683));
#26095=CARTESIAN_POINT('Ctrl Pts',(-62.1292609739061,-104.593788698099,
174.328630986959));
#26096=CARTESIAN_POINT('Ctrl Pts',(-62.119322842052,-104.500566940792,175.985485236451));
#26097=CARTESIAN_POINT('Ctrl Pts',(-62.1093847101978,-104.407345183486,
177.642339485944));
#26098=CARTESIAN_POINT('Ctrl Pts',(-60.9344749627642,-104.438317183453,
178.813912312176));
#26099=CARTESIAN_POINT('Ctrl Pts',(-59.7595652153305,-104.46928918342,179.985485138407));
#26100=CARTESIAN_POINT('Ctrl Pts',(-58.1021084653266,-104.551703917706,
179.985485069079));
#26101=CARTESIAN_POINT('Ctrl Pts',(-56.4446517153227,-104.634118651992,
179.985484999752));
#26102=CARTESIAN_POINT('Ctrl Pts',(-55.269742065381,-104.665090641566,178.813912075476));
#26103=CARTESIAN_POINT('Ctrl Pts',(-54.0948324154392,-104.696062631139,
177.6423391512));
#26104=CARTESIAN_POINT('Ctrl Pts',(-54.0848944214593,-104.602840859135,
175.985484901707));
#26105=CARTESIAN_POINT('Ctrl Pts',(-54.0749564274795,-104.50961908713,174.328630652215));
#26106=CARTESIAN_POINT('Ctrl Pts',(-55.2299900490791,-104.292203557853,
173.157057825983));
#26107=CARTESIAN_POINT('Ctrl Pts',(-56.3850236706787,-104.074788028575,
171.985484999752));
#26108=CARTESIAN_POINT('Ctrl Pts',(-58.0226042948486,-103.805929764978,
171.985485069079));
#26109=CARTESIAN_POINT('Ctrl Pts',(-59.6601849190184,-103.537071501381,
171.985485138407));
#26110=CARTESIAN_POINT('Ctrl Pts',(-60.8152184431262,-103.319655982497,
173.157058062683));
#26111=CARTESIAN_POINT('Ctrl Pts',(-61.9702519672339,-103.102240463613,
174.328630986959));
#26112=CARTESIAN_POINT('Ctrl Pts',(-61.9603138353797,-103.009018706307,
175.985485236451));
#26113=CARTESIAN_POINT('Ctrl Pts',(-61.9503757035256,-102.915796949001,
177.642339485944));
#26114=CARTESIAN_POINT('Ctrl Pts',(-60.7754659560919,-102.946768948967,
178.813912312176));
#26115=CARTESIAN_POINT('Ctrl Pts',(-59.6005562086583,-102.977740948934,
179.985485138407));
#26116=CARTESIAN_POINT('Ctrl Pts',(-57.9430994586544,-103.06015568322,179.985485069079));
#26117=CARTESIAN_POINT('Ctrl Pts',(-56.2856427086505,-103.142570417507,
179.985484999752));
#26118=CARTESIAN_POINT('Ctrl Pts',(-55.1107330587087,-103.17354240708,178.813912075476));
#26119=CARTESIAN_POINT('Ctrl Pts',(-53.935823408767,-103.204514396654,177.6423391512));
#26120=CARTESIAN_POINT('Ctrl Pts',(-53.9258854147871,-103.111292624649,
175.985484901707));
#26121=CARTESIAN_POINT('Ctrl Pts',(-53.9159474208072,-103.018070852645,
174.328630652215));
#26122=CARTESIAN_POINT('Ctrl Pts',(-55.0709810424069,-102.800655323367,
173.157057825983));
#26123=CARTESIAN_POINT('Ctrl Pts',(-56.2260146640065,-102.58323979409,171.985484999752));
#26124=CARTESIAN_POINT('Ctrl Pts',(-57.8635952881763,-102.314381530493,
171.985485069079));
#26125=CARTESIAN_POINT('Ctrl Pts',(-59.5011759123462,-102.045523266896,
171.985485138407));
#26126=CARTESIAN_POINT('Ctrl Pts',(-60.6562094364539,-101.828107748012,
173.157058062683));
#26127=CARTESIAN_POINT('Ctrl Pts',(-61.8112429605617,-101.610692229127,
174.328630986959));
#26128=CARTESIAN_POINT('Ctrl Pts',(-61.8013048287075,-101.517470471821,
175.985485236451));
#26129=CARTESIAN_POINT('Ctrl Pts',(-61.7913666968533,-101.424248714515,
177.642339485944));
#26130=CARTESIAN_POINT('Ctrl Pts',(-60.6164569494197,-101.455220714482,
178.813912312176));
#26131=CARTESIAN_POINT('Ctrl Pts',(-59.4415472019861,-101.486192714449,
179.985485138407));
#26132=CARTESIAN_POINT('Ctrl Pts',(-57.7840904519822,-101.568607448735,
179.985485069079));
#26133=CARTESIAN_POINT('Ctrl Pts',(-56.1266337019783,-101.651022183021,
179.985484999752));
#26134=CARTESIAN_POINT('Ctrl Pts',(-54.9517240520365,-101.681994172595,
178.813912075476));
#26135=CARTESIAN_POINT('Ctrl Pts',(-53.7768144020947,-101.712966162168,
177.6423391512));
#26136=CARTESIAN_POINT('Ctrl Pts',(-53.7668764081149,-101.619744390164,
175.985484901707));
#26137=CARTESIAN_POINT('Ctrl Pts',(-53.756938414135,-101.526522618159,174.328630652215));
#26138=CARTESIAN_POINT('Ctrl Pts',(-54.9119720357346,-101.309107088882,
173.157057825983));
#26139=CARTESIAN_POINT('Ctrl Pts',(-56.0670056573342,-101.091691559604,
171.985484999752));
#26140=CARTESIAN_POINT('Ctrl Pts',(-57.7045862815041,-100.822833296007,
171.985485069079));
#26141=CARTESIAN_POINT('Ctrl Pts',(-59.342166905674,-100.55397503241,171.985485138407));
#26142=CARTESIAN_POINT('Ctrl Pts',(-60.4972004297817,-100.336559513526,
173.157058062683));
#26143=CARTESIAN_POINT('Ctrl Pts',(-61.6522339538895,-100.119143994642,
174.328630986959));
#26144=CARTESIAN_POINT('Ctrl Pts',(-61.6422958220353,-100.025922237336,
175.985485236451));
#26145=CARTESIAN_POINT('Ctrl Pts',(-61.6323576901811,-99.9327004800294,
177.642339485944));
#26146=CARTESIAN_POINT('Ctrl Pts',(-60.4574479427475,-99.9636724799962,
178.813912312176));
#26147=CARTESIAN_POINT('Ctrl Pts',(-59.2825381953138,-99.994644479963,179.985485138407));
#26148=CARTESIAN_POINT('Ctrl Pts',(-57.6250814453099,-100.077059214249,
179.985485069079));
#26149=CARTESIAN_POINT('Ctrl Pts',(-55.9676246953061,-100.159473948536,
179.985484999752));
#26150=CARTESIAN_POINT('Ctrl Pts',(-54.7927150453643,-100.190445938109,
178.813912075476));
#26151=CARTESIAN_POINT('Ctrl Pts',(-53.6178053954225,-100.221417927683,
177.6423391512));
#26152=CARTESIAN_POINT('Ctrl Pts',(-53.6078674014426,-100.128196155678,
175.985484901707));
#26153=CARTESIAN_POINT('Ctrl Pts',(-53.5979294074628,-100.034974383673,
174.328630652215));
#26154=CARTESIAN_POINT('Ctrl Pts',(-54.7529630290624,-99.817558854396,173.157057825983));
#26155=CARTESIAN_POINT('Ctrl Pts',(-55.907996650662,-99.6001433251185,171.985484999752));
#26156=CARTESIAN_POINT('Ctrl Pts',(-57.5455772748319,-99.3312850615215,
171.985485069079));
#26157=CARTESIAN_POINT('Ctrl Pts',(-59.1831578990017,-99.0624267979246,
171.985485138407));
#26158=CARTESIAN_POINT('Ctrl Pts',(-60.3381914231095,-98.8450112790404,
173.157058062683));
#26159=CARTESIAN_POINT('Ctrl Pts',(-61.4932249472172,-98.6275957601562,
174.328630986959));
#26160=CARTESIAN_POINT('Ctrl Pts',(-61.4832868153631,-98.53437400285,175.985485236451));
#26161=CARTESIAN_POINT('Ctrl Pts',(-61.4733486835089,-98.4411522455438,
177.642339485944));
#26162=CARTESIAN_POINT('Ctrl Pts',(-60.2984389360752,-98.4721242455106,
178.813912312176));
#26163=CARTESIAN_POINT('Ctrl Pts',(-59.1235291886416,-98.5030962454774,
179.985485138407));
#26164=CARTESIAN_POINT('Ctrl Pts',(-57.4660724386377,-98.5855109797636,
179.985485069079));
#26165=CARTESIAN_POINT('Ctrl Pts',(-55.8086156886338,-98.6679257140499,
179.985484999752));
#26166=CARTESIAN_POINT('Ctrl Pts',(-54.633706038692,-98.6988977036234,178.813912075476));
#26167=CARTESIAN_POINT('Ctrl Pts',(-56.9964983346804,-113.864655531781,
178.072094410988));
#26168=CARTESIAN_POINT('Ctrl Pts',(-56.1271283009022,-113.863054956993,
177.207792449865));
#26169=CARTESIAN_POINT('Ctrl Pts',(-56.117190288842,-113.769833186916,175.985484945604));
#26170=CARTESIAN_POINT('Ctrl Pts',(-56.1072522767819,-113.676611416839,
174.763177441344));
#26171=CARTESIAN_POINT('Ctrl Pts',(-56.9567462566485,-113.491768454648,
173.89887555255));
#26172=CARTESIAN_POINT('Ctrl Pts',(-57.8062402365152,-113.306925492458,
173.034573663757));
#26173=CARTESIAN_POINT('Ctrl Pts',(-59.011722573584,-113.084131793069,173.034573714903));
#26174=CARTESIAN_POINT('Ctrl Pts',(-60.2172049106529,-112.86133809368,173.034573766048));
#26175=CARTESIAN_POINT('Ctrl Pts',(-61.0666988185971,-112.676495139156,
173.898875727171));
#26176=CARTESIAN_POINT('Ctrl Pts',(-61.9161927265413,-112.491652184633,
174.763177688294));
#26177=CARTESIAN_POINT('Ctrl Pts',(-61.9062546127674,-112.398430425399,
175.985485192554));
#26178=CARTESIAN_POINT('Ctrl Pts',(-61.8963164989935,-112.305208666166,
177.207792696815));
#26179=CARTESIAN_POINT('Ctrl Pts',(-61.0269463932928,-112.303608099046,
178.072094585608));
#26180=CARTESIAN_POINT('Ctrl Pts',(-60.1575762875921,-112.302007531926,
178.936396474401));
#26181=CARTESIAN_POINT('Ctrl Pts',(-58.9322178246893,-112.338357702004,
178.936396423256));
#26182=CARTESIAN_POINT('Ctrl Pts',(-57.7068593617864,-112.374707872082,
178.936396372111));
#26183=CARTESIAN_POINT('Ctrl Pts',(-56.8374893280082,-112.373107297295,
178.072094410988));
#26184=CARTESIAN_POINT('Ctrl Pts',(-55.9681192942299,-112.371506722508,
177.207792449865));
#26185=CARTESIAN_POINT('Ctrl Pts',(-55.9581812821698,-112.278284952431,
175.985484945604));
#26186=CARTESIAN_POINT('Ctrl Pts',(-55.9482432701096,-112.185063182354,
174.763177441344));
#26187=CARTESIAN_POINT('Ctrl Pts',(-56.7977372499763,-112.000220220163,
173.89887555255));
#26188=CARTESIAN_POINT('Ctrl Pts',(-57.647231229843,-111.815377257972,173.034573663757));
#26189=CARTESIAN_POINT('Ctrl Pts',(-58.8527135669118,-111.592583558583,
173.034573714903));
#26190=CARTESIAN_POINT('Ctrl Pts',(-60.0581959039807,-111.369789859194,
173.034573766048));
#26191=CARTESIAN_POINT('Ctrl Pts',(-60.9076898119249,-111.184946904671,
173.898875727171));
#26192=CARTESIAN_POINT('Ctrl Pts',(-61.7571837198691,-111.000103950148,
174.763177688294));
#26193=CARTESIAN_POINT('Ctrl Pts',(-61.7472456060952,-110.906882190914,
175.985485192554));
#26194=CARTESIAN_POINT('Ctrl Pts',(-61.7373074923213,-110.81366043168,177.207792696815));
#26195=CARTESIAN_POINT('Ctrl Pts',(-60.8679373866206,-110.81205986456,178.072094585608));
#26196=CARTESIAN_POINT('Ctrl Pts',(-59.9985672809199,-110.81045929744,178.936396474401));
#26197=CARTESIAN_POINT('Ctrl Pts',(-58.7732088180171,-110.846809467519,
178.936396423256));
#26198=CARTESIAN_POINT('Ctrl Pts',(-57.5478503551142,-110.883159637597,
178.936396372111));
#26199=CARTESIAN_POINT('Ctrl Pts',(-56.6784803213359,-110.881559062809,
178.072094410988));
#26200=CARTESIAN_POINT('Ctrl Pts',(-55.8091102875577,-110.879958488022,
177.207792449865));
#26201=CARTESIAN_POINT('Ctrl Pts',(-55.7991722754976,-110.786736717945,
175.985484945604));
#26202=CARTESIAN_POINT('Ctrl Pts',(-55.7892342634374,-110.693514947868,
174.763177441344));
#26203=CARTESIAN_POINT('Ctrl Pts',(-56.6387282433041,-110.508671985677,
173.89887555255));
#26204=CARTESIAN_POINT('Ctrl Pts',(-57.4882222231708,-110.323829023487,
173.034573663757));
#26205=CARTESIAN_POINT('Ctrl Pts',(-58.6937045602396,-110.101035324098,
173.034573714903));
#26206=CARTESIAN_POINT('Ctrl Pts',(-59.8991868973084,-109.878241624709,
173.034573766048));
#26207=CARTESIAN_POINT('Ctrl Pts',(-60.7486808052526,-109.693398670185,
173.898875727171));
#26208=CARTESIAN_POINT('Ctrl Pts',(-61.5981747131968,-109.508555715662,
174.763177688294));
#26209=CARTESIAN_POINT('Ctrl Pts',(-61.588236599423,-109.415333956428,175.985485192554));
#26210=CARTESIAN_POINT('Ctrl Pts',(-61.5782984856491,-109.322112197195,
177.207792696815));
#26211=CARTESIAN_POINT('Ctrl Pts',(-60.7089283799484,-109.320511630075,
178.072094585608));
#26212=CARTESIAN_POINT('Ctrl Pts',(-59.8395582742477,-109.318911062955,
178.936396474401));
#26213=CARTESIAN_POINT('Ctrl Pts',(-58.6141998113448,-109.355261233033,
178.936396423256));
#26214=CARTESIAN_POINT('Ctrl Pts',(-57.388841348442,-109.391611403111,178.936396372111));
#26215=CARTESIAN_POINT('Ctrl Pts',(-56.5194713146637,-109.390010828324,
178.072094410988));
#26216=CARTESIAN_POINT('Ctrl Pts',(-55.6501012808855,-109.388410253536,
177.207792449865));
#26217=CARTESIAN_POINT('Ctrl Pts',(-55.6401632688253,-109.295188483459,
175.985484945604));
#26218=CARTESIAN_POINT('Ctrl Pts',(-55.6302252567652,-109.201966713382,
174.763177441344));
#26219=CARTESIAN_POINT('Ctrl Pts',(-56.4797192366319,-109.017123751192,
173.89887555255));
#26220=CARTESIAN_POINT('Ctrl Pts',(-57.3292132164985,-108.832280789001,
173.034573663757));
#26221=CARTESIAN_POINT('Ctrl Pts',(-58.5346955535674,-108.609487089612,
173.034573714903));
#26222=CARTESIAN_POINT('Ctrl Pts',(-59.7401778906362,-108.386693390223,
173.034573766048));
#26223=CARTESIAN_POINT('Ctrl Pts',(-60.5896717985804,-108.2018504357,173.898875727171));
#26224=CARTESIAN_POINT('Ctrl Pts',(-61.4391657065246,-108.017007481176,
174.763177688294));
#26225=CARTESIAN_POINT('Ctrl Pts',(-61.4292275927507,-107.923785721943,
175.985485192554));
#26226=CARTESIAN_POINT('Ctrl Pts',(-61.4192894789769,-107.830563962709,
177.207792696815));
#26227=CARTESIAN_POINT('Ctrl Pts',(-60.5499193732762,-107.828963395589,
178.072094585608));
#26228=CARTESIAN_POINT('Ctrl Pts',(-59.6805492675755,-107.827362828469,
178.936396474401));
#26229=CARTESIAN_POINT('Ctrl Pts',(-58.4551908046726,-107.863712998547,
178.936396423256));
#26230=CARTESIAN_POINT('Ctrl Pts',(-57.2298323417698,-107.900063168626,
178.936396372111));
#26231=CARTESIAN_POINT('Ctrl Pts',(-56.3604623079915,-107.898462593838,
178.072094410988));
#26232=CARTESIAN_POINT('Ctrl Pts',(-55.4910922742133,-107.896862019051,
177.207792449865));
#26233=CARTESIAN_POINT('Ctrl Pts',(-55.4811542621531,-107.803640248974,
175.985484945604));
#26234=CARTESIAN_POINT('Ctrl Pts',(-55.471216250093,-107.710418478897,174.763177441344));
#26235=CARTESIAN_POINT('Ctrl Pts',(-56.3207102299596,-107.525575516706,
173.89887555255));
#26236=CARTESIAN_POINT('Ctrl Pts',(-57.1702042098263,-107.340732554515,
173.034573663757));
#26237=CARTESIAN_POINT('Ctrl Pts',(-58.3756865468951,-107.117938855126,
173.034573714903));
#26238=CARTESIAN_POINT('Ctrl Pts',(-59.581168883964,-106.895145155737,173.034573766048));
#26239=CARTESIAN_POINT('Ctrl Pts',(-60.4306627919082,-106.710302201214,
173.898875727171));
#26240=CARTESIAN_POINT('Ctrl Pts',(-61.2801566998524,-106.525459246691,
174.763177688294));
#26241=CARTESIAN_POINT('Ctrl Pts',(-61.2702185860785,-106.432237487457,
175.985485192554));
#26242=CARTESIAN_POINT('Ctrl Pts',(-61.2602804723046,-106.339015728223,
177.207792696815));
#26243=CARTESIAN_POINT('Ctrl Pts',(-60.3909103666039,-106.337415161103,
178.072094585608));
#26244=CARTESIAN_POINT('Ctrl Pts',(-59.5215402609032,-106.335814593983,
178.936396474401));
#26245=CARTESIAN_POINT('Ctrl Pts',(-58.2961817980004,-106.372164764062,
178.936396423256));
#26246=CARTESIAN_POINT('Ctrl Pts',(-57.0708233350975,-106.40851493414,178.936396372111));
#26247=CARTESIAN_POINT('Ctrl Pts',(-56.2014533013193,-106.406914359353,
178.072094410988));
#26248=CARTESIAN_POINT('Ctrl Pts',(-55.332083267541,-106.405313784565,177.207792449865));
#26249=CARTESIAN_POINT('Ctrl Pts',(-55.3221452554809,-106.312092014488,
175.985484945604));
#26250=CARTESIAN_POINT('Ctrl Pts',(-55.3122072434207,-106.218870244411,
174.763177441344));
#26251=CARTESIAN_POINT('Ctrl Pts',(-56.1617012232874,-106.034027282221,
173.89887555255));
#26252=CARTESIAN_POINT('Ctrl Pts',(-57.0111952031541,-105.84918432003,173.034573663757));
#26253=CARTESIAN_POINT('Ctrl Pts',(-58.2166775402229,-105.626390620641,
173.034573714903));
#26254=CARTESIAN_POINT('Ctrl Pts',(-59.4221598772917,-105.403596921252,
173.034573766048));
#26255=CARTESIAN_POINT('Ctrl Pts',(-60.2716537852359,-105.218753966728,
173.898875727171));
#26256=CARTESIAN_POINT('Ctrl Pts',(-61.1211476931802,-105.033911012205,
174.763177688294));
#26257=CARTESIAN_POINT('Ctrl Pts',(-61.1112095794063,-104.940689252971,
175.985485192554));
#26258=CARTESIAN_POINT('Ctrl Pts',(-61.1012714656324,-104.847467493738,
177.207792696815));
#26259=CARTESIAN_POINT('Ctrl Pts',(-60.2319013599317,-104.845866926618,
178.072094585608));
#26260=CARTESIAN_POINT('Ctrl Pts',(-59.362531254231,-104.844266359498,178.936396474401));
#26261=CARTESIAN_POINT('Ctrl Pts',(-58.1371727913281,-104.880616529576,
178.936396423256));
#26262=CARTESIAN_POINT('Ctrl Pts',(-56.9118143284253,-104.916966699654,
178.936396372111));
#26263=CARTESIAN_POINT('Ctrl Pts',(-56.042444294647,-104.915366124867,178.072094410988));
#26264=CARTESIAN_POINT('Ctrl Pts',(-55.1730742608688,-104.91376555008,177.207792449865));
#26265=CARTESIAN_POINT('Ctrl Pts',(-55.1631362488087,-104.820543780003,
175.985484945604));
#26266=CARTESIAN_POINT('Ctrl Pts',(-55.1531982367485,-104.727322009926,
174.763177441344));
#26267=CARTESIAN_POINT('Ctrl Pts',(-56.0026922166152,-104.542479047735,
173.89887555255));
#26268=CARTESIAN_POINT('Ctrl Pts',(-56.8521861964818,-104.357636085544,
173.034573663757));
#26269=CARTESIAN_POINT('Ctrl Pts',(-58.0576685335507,-104.134842386155,
173.034573714903));
#26270=CARTESIAN_POINT('Ctrl Pts',(-59.2631508706195,-103.912048686766,
173.034573766048));
#26271=CARTESIAN_POINT('Ctrl Pts',(-60.1126447785637,-103.727205732243,
173.898875727171));
#26272=CARTESIAN_POINT('Ctrl Pts',(-60.9621386865079,-103.54236277772,174.763177688294));
#26273=CARTESIAN_POINT('Ctrl Pts',(-60.952200572734,-103.449141018486,175.985485192554));
#26274=CARTESIAN_POINT('Ctrl Pts',(-60.9422624589602,-103.355919259252,
177.207792696815));
#26275=CARTESIAN_POINT('Ctrl Pts',(-60.0728923532595,-103.354318692132,
178.072094585608));
#26276=CARTESIAN_POINT('Ctrl Pts',(-59.2035222475588,-103.352718125012,
178.936396474401));
#26277=CARTESIAN_POINT('Ctrl Pts',(-57.9781637846559,-103.389068295091,
178.936396423256));
#26278=CARTESIAN_POINT('Ctrl Pts',(-56.7528053217531,-103.425418465169,
178.936396372111));
#26279=CARTESIAN_POINT('Ctrl Pts',(-55.8834352879748,-103.423817890381,
178.072094410988));
#26280=CARTESIAN_POINT('Ctrl Pts',(-55.0140652541966,-103.422217315594,
177.207792449865));
#26281=CARTESIAN_POINT('Ctrl Pts',(-55.0041272421364,-103.328995545517,
175.985484945604));
#26282=CARTESIAN_POINT('Ctrl Pts',(-54.9941892300763,-103.23577377544,174.763177441344));
#26283=CARTESIAN_POINT('Ctrl Pts',(-55.8436832099429,-103.050930813249,
173.89887555255));
#26284=CARTESIAN_POINT('Ctrl Pts',(-56.6931771898096,-102.866087851059,
173.034573663757));
#26285=CARTESIAN_POINT('Ctrl Pts',(-57.8986595268784,-102.64329415167,173.034573714903));
#26286=CARTESIAN_POINT('Ctrl Pts',(-59.1041418639473,-102.420500452281,
173.034573766048));
#26287=CARTESIAN_POINT('Ctrl Pts',(-59.9536357718915,-102.235657497757,
173.898875727171));
#26288=CARTESIAN_POINT('Ctrl Pts',(-60.8031296798357,-102.050814543234,
174.763177688294));
#26289=CARTESIAN_POINT('Ctrl Pts',(-60.7931915660618,-101.957592784,175.985485192554));
#26290=CARTESIAN_POINT('Ctrl Pts',(-60.783253452288,-101.864371024767,177.207792696815));
#26291=CARTESIAN_POINT('Ctrl Pts',(-59.9138833465873,-101.862770457647,
178.072094585608));
#26292=CARTESIAN_POINT('Ctrl Pts',(-59.0445132408866,-101.861169890527,
178.936396474401));
#26293=CARTESIAN_POINT('Ctrl Pts',(-57.8191547779837,-101.897520060605,
178.936396423256));
#26294=CARTESIAN_POINT('Ctrl Pts',(-56.5937963150808,-101.933870230683,
178.936396372111));
#26295=CARTESIAN_POINT('Ctrl Pts',(-55.7244262813026,-101.932269655896,
178.072094410988));
#26296=CARTESIAN_POINT('Ctrl Pts',(-54.8550562475244,-101.930669081108,
177.207792449865));
#26297=CARTESIAN_POINT('Ctrl Pts',(-54.8451182354642,-101.837447311031,
175.985484945604));
#26298=CARTESIAN_POINT('Ctrl Pts',(-54.8351802234041,-101.744225540954,
174.763177441344));
#26299=CARTESIAN_POINT('Ctrl Pts',(-55.6846742032707,-101.559382578764,
173.89887555255));
#26300=CARTESIAN_POINT('Ctrl Pts',(-56.5341681831374,-101.374539616573,
173.034573663757));
#26301=CARTESIAN_POINT('Ctrl Pts',(-57.7396505202062,-101.151745917184,
173.034573714903));
#26302=CARTESIAN_POINT('Ctrl Pts',(-58.9451328572751,-100.928952217795,
173.034573766048));
#26303=CARTESIAN_POINT('Ctrl Pts',(-59.7946267652193,-100.744109263272,
173.898875727171));
#26304=CARTESIAN_POINT('Ctrl Pts',(-60.6441206731635,-100.559266308748,
174.763177688294));
#26305=CARTESIAN_POINT('Ctrl Pts',(-60.6341825593896,-100.466044549515,
175.985485192554));
#26306=CARTESIAN_POINT('Ctrl Pts',(-60.6242444456157,-100.372822790281,
177.207792696815));
#26307=CARTESIAN_POINT('Ctrl Pts',(-59.754874339915,-100.371222223161,178.072094585608));
#26308=CARTESIAN_POINT('Ctrl Pts',(-58.8855042342143,-100.369621656041,
178.936396474401));
#26309=CARTESIAN_POINT('Ctrl Pts',(-57.6601457713115,-100.405971826119,
178.936396423256));
#26310=CARTESIAN_POINT('Ctrl Pts',(-56.4347873084086,-100.442321996198,
178.936396372111));
#26311=CARTESIAN_POINT('Ctrl Pts',(-55.5654172746304,-100.44072142141,178.072094410988));
#26312=CARTESIAN_POINT('Ctrl Pts',(-54.6960472408521,-100.439120846623,
177.207792449865));
#26313=CARTESIAN_POINT('Ctrl Pts',(-54.686109228792,-100.345899076546,175.985484945604));
#26314=CARTESIAN_POINT('Ctrl Pts',(-54.6761712167318,-100.252677306469,
174.763177441344));
#26315=CARTESIAN_POINT('Ctrl Pts',(-55.5256651965985,-100.067834344278,
173.89887555255));
#26316=CARTESIAN_POINT('Ctrl Pts',(-56.3751591764652,-99.8829913820874,
173.034573663757));
#26317=CARTESIAN_POINT('Ctrl Pts',(-57.580641513534,-99.6601976826983,173.034573714903));
#26318=CARTESIAN_POINT('Ctrl Pts',(-58.7861238506028,-99.4374039833093,
173.034573766048));
#26319=CARTESIAN_POINT('Ctrl Pts',(-59.635617758547,-99.252561028786,173.898875727171));
#26320=CARTESIAN_POINT('Ctrl Pts',(-60.4851116664912,-99.0677180742627,
174.763177688294));
#26321=CARTESIAN_POINT('Ctrl Pts',(-60.4751735527174,-98.9744963150291,
175.985485192554));
#26322=CARTESIAN_POINT('Ctrl Pts',(-60.4652354389435,-98.8812745557954,
177.207792696815));
#26323=CARTESIAN_POINT('Ctrl Pts',(-59.5958653332428,-98.8796739886754,
178.072094585608));
#26324=CARTESIAN_POINT('Ctrl Pts',(-58.7264952275421,-98.8780734215554,
178.936396474401));
#26325=CARTESIAN_POINT('Ctrl Pts',(-57.5011367646392,-98.9144235916337,
178.936396423256));
#26326=CARTESIAN_POINT('Ctrl Pts',(-56.2757783017364,-98.9507737617121,
178.936396372111));
#26327=CARTESIAN_POINT('Ctrl Pts',(-55.4064082679581,-98.9491731869247,
178.072094410988));
#26328=CARTESIAN_POINT('Ctrl Pts',(-61.7066176068137,-108.90712070075,178.485485069079));
#26329=CARTESIAN_POINT('Ctrl Pts',(-61.568045402457,-108.908835218628,178.657813499464));
#26330=CARTESIAN_POINT('Ctrl Pts',(-61.4115019827808,-108.91296188691,178.813912312176));
#26331=CARTESIAN_POINT('Ctrl Pts',(-60.2365922353472,-108.943933886877,
179.985485138407));
#26332=CARTESIAN_POINT('Ctrl Pts',(-58.5791354853433,-109.026348621163,
179.985485069079));
#26333=CARTESIAN_POINT('Ctrl Pts',(-56.9216787353394,-109.108763355449,
179.985484999752));
#26334=CARTESIAN_POINT('Ctrl Pts',(-55.7467690853976,-109.139735345023,
178.813912075476));
#26335=CARTESIAN_POINT('Ctrl Pts',(-54.5718594354559,-109.170707334596,
177.6423391512));
#26336=CARTESIAN_POINT('Ctrl Pts',(-54.561921441476,-109.077485562592,175.985484901707));
#26337=CARTESIAN_POINT('Ctrl Pts',(-54.5519834474962,-108.984263790587,
174.328630652215));
#26338=CARTESIAN_POINT('Ctrl Pts',(-55.7070170690958,-108.76684826131,173.157057825983));
#26339=CARTESIAN_POINT('Ctrl Pts',(-56.8620506906954,-108.549432732032,
171.985484999752));
#26340=CARTESIAN_POINT('Ctrl Pts',(-58.4996313148652,-108.280574468435,
171.985485069079));
#26341=CARTESIAN_POINT('Ctrl Pts',(-60.1372119390351,-108.011716204838,
171.985485138407));
#26342=CARTESIAN_POINT('Ctrl Pts',(-61.2922454631428,-107.794300685954,
173.157058062683));
#26343=CARTESIAN_POINT('Ctrl Pts',(-61.446140484096,-107.765332552012,173.313156769748));
#26344=CARTESIAN_POINT('Ctrl Pts',(-61.5819596880668,-107.737795122829,
173.485485069079));
#26345=CARTESIAN_POINT('Ctrl Pts',(-56.8733667677527,-112.709647553905,
178.072094410988));
#26346=CARTESIAN_POINT('Ctrl Pts',(-56.0039967339745,-112.708046979118,
177.207792449865));
#26347=CARTESIAN_POINT('Ctrl Pts',(-55.9940587219143,-112.614825209041,
175.985484945604));
#26348=CARTESIAN_POINT('Ctrl Pts',(-55.9841207098542,-112.521603438964,
174.763177441344));
#26349=CARTESIAN_POINT('Ctrl Pts',(-56.8336146897208,-112.336760476773,
173.89887555255));
#26350=CARTESIAN_POINT('Ctrl Pts',(-57.6831086695875,-112.151917514582,
173.034573663757));
#26351=CARTESIAN_POINT('Ctrl Pts',(-58.8885910066563,-111.929123815193,
173.034573714903));
#26352=CARTESIAN_POINT('Ctrl Pts',(-60.0940733437252,-111.706330115804,
173.034573766048));
#26353=CARTESIAN_POINT('Ctrl Pts',(-60.9435672516694,-111.521487161281,
173.898875727171));
#26354=CARTESIAN_POINT('Ctrl Pts',(-61.7930611596136,-111.336644206758,
174.763177688294));
#26355=CARTESIAN_POINT('Ctrl Pts',(-61.7831230458397,-111.243422447524,
175.985485192554));
#26356=CARTESIAN_POINT('Ctrl Pts',(-61.7731849320658,-111.15020068829,177.207792696815));
#26357=CARTESIAN_POINT('Ctrl Pts',(-60.9038148263651,-111.14860012117,178.072094585608));
#26358=CARTESIAN_POINT('Ctrl Pts',(-60.0344447206644,-111.14699955405,178.936396474401));
#26359=CARTESIAN_POINT('Ctrl Pts',(-58.8090862577616,-111.183349724129,
178.936396423256));
#26360=CARTESIAN_POINT('Ctrl Pts',(-57.5837277948587,-111.219699894207,
178.936396372111));
#26361=CARTESIAN_POINT('Ctrl Pts',(-56.7143577610805,-111.21809931942,178.072094410988));
#26362=CARTESIAN_POINT('Ctrl Pts',(-55.8449877273022,-111.216498744632,
177.207792449865));
#26363=CARTESIAN_POINT('Ctrl Pts',(-55.8350497152421,-111.123276974555,
175.985484945604));
#26364=CARTESIAN_POINT('Ctrl Pts',(-55.8251117031819,-111.030055204478,
174.763177441344));
#26365=CARTESIAN_POINT('Ctrl Pts',(-56.6746056830486,-110.845212242287,
173.89887555255));
#26366=CARTESIAN_POINT('Ctrl Pts',(-57.5240996629153,-110.660369280097,
173.034573663757));
#26367=CARTESIAN_POINT('Ctrl Pts',(-58.7295819999841,-110.437575580708,
173.034573714903));
#26368=CARTESIAN_POINT('Ctrl Pts',(-59.9350643370529,-110.214781881319,
173.034573766048));
#26369=CARTESIAN_POINT('Ctrl Pts',(-60.7845582449971,-110.029938926795,
173.898875727171));
#26370=CARTESIAN_POINT('Ctrl Pts',(-61.6340521529414,-109.845095972272,
174.763177688294));
#26371=CARTESIAN_POINT('Ctrl Pts',(-61.6241140391675,-109.751874213038,
175.985485192554));
#26372=CARTESIAN_POINT('Ctrl Pts',(-61.6141759253936,-109.658652453805,
177.207792696815));
#26373=CARTESIAN_POINT('Ctrl Pts',(-60.7448058196929,-109.657051886685,
178.072094585608));
#26374=CARTESIAN_POINT('Ctrl Pts',(-59.8754357139922,-109.655451319565,
178.936396474401));
#26375=CARTESIAN_POINT('Ctrl Pts',(-58.6500772510893,-109.691801489643,
178.936396423256));
#26376=CARTESIAN_POINT('Ctrl Pts',(-57.4247187881865,-109.728151659721,
178.936396372111));
#26377=CARTESIAN_POINT('Ctrl Pts',(-56.5553487544082,-109.726551084934,
178.072094410988));
#26378=CARTESIAN_POINT('Ctrl Pts',(-55.68597872063,-109.724950510147,177.207792449865));
#26379=CARTESIAN_POINT('Ctrl Pts',(-55.6760407085698,-109.63172874007,175.985484945604));
#26380=CARTESIAN_POINT('Ctrl Pts',(-55.6661026965097,-109.538506969993,
174.763177441344));
#26381=CARTESIAN_POINT('Ctrl Pts',(-56.5155966763764,-109.353664007802,
173.89887555255));
#26382=CARTESIAN_POINT('Ctrl Pts',(-57.365090656243,-109.168821045611,173.034573663757));
#26383=CARTESIAN_POINT('Ctrl Pts',(-58.5705729933119,-108.946027346222,
173.034573714903));
#26384=CARTESIAN_POINT('Ctrl Pts',(-59.7760553303807,-108.723233646833,
173.034573766048));
#26385=CARTESIAN_POINT('Ctrl Pts',(-60.6255492383249,-108.53839069231,173.898875727171));
#26386=CARTESIAN_POINT('Ctrl Pts',(-61.4750431462691,-108.353547737786,
174.763177688294));
#26387=CARTESIAN_POINT('Ctrl Pts',(-61.4651050324952,-108.260325978553,
175.985485192554));
#26388=CARTESIAN_POINT('Ctrl Pts',(-61.4551669187214,-108.167104219319,
177.207792696815));
#26389=CARTESIAN_POINT('Ctrl Pts',(-60.5857968130207,-108.165503652199,
178.072094585608));
#26390=CARTESIAN_POINT('Ctrl Pts',(-59.71642670732,-108.163903085079,178.936396474401));
#26391=CARTESIAN_POINT('Ctrl Pts',(-58.4910682444171,-108.200253255158,
178.936396423256));
#26392=CARTESIAN_POINT('Ctrl Pts',(-57.2657097815143,-108.236603425236,
178.936396372111));
#26393=CARTESIAN_POINT('Ctrl Pts',(-56.396339747736,-108.235002850448,178.072094410988));
#26394=CARTESIAN_POINT('Ctrl Pts',(-55.5269697139578,-108.233402275661,
177.207792449865));
#26395=CARTESIAN_POINT('Ctrl Pts',(-55.5170317018976,-108.140180505584,
175.985484945604));
#26396=CARTESIAN_POINT('Ctrl Pts',(-55.5070936898375,-108.046958735507,
174.763177441344));
#26397=CARTESIAN_POINT('Ctrl Pts',(-56.3565876697041,-107.862115773316,
173.89887555255));
#26398=CARTESIAN_POINT('Ctrl Pts',(-57.2060816495708,-107.677272811126,
173.034573663757));
#26399=CARTESIAN_POINT('Ctrl Pts',(-58.4115639866396,-107.454479111736,
173.034573714903));
#26400=CARTESIAN_POINT('Ctrl Pts',(-59.6170463237085,-107.231685412347,
173.034573766048));
#26401=CARTESIAN_POINT('Ctrl Pts',(-60.4665402316527,-107.046842457824,
173.898875727171));
#26402=CARTESIAN_POINT('Ctrl Pts',(-61.3160341395969,-106.861999503301,
174.763177688294));
#26403=CARTESIAN_POINT('Ctrl Pts',(-61.306096025823,-106.768777744067,175.985485192554));
#26404=CARTESIAN_POINT('Ctrl Pts',(-61.2961579120492,-106.675555984834,
177.207792696815));
#26405=CARTESIAN_POINT('Ctrl Pts',(-60.4267878063484,-106.673955417714,
178.072094585608));
#26406=CARTESIAN_POINT('Ctrl Pts',(-59.5574177006478,-106.672354850594,
178.936396474401));
#26407=CARTESIAN_POINT('Ctrl Pts',(-58.3320592377449,-106.708705020672,
178.936396423256));
#26408=CARTESIAN_POINT('Ctrl Pts',(-57.106700774842,-106.74505519075,178.936396372111));
#26409=CARTESIAN_POINT('Ctrl Pts',(-56.2373307410638,-106.743454615963,
178.072094410988));
#26410=CARTESIAN_POINT('Ctrl Pts',(-55.3679607072856,-106.741854041175,
177.207792449865));
#26411=CARTESIAN_POINT('Ctrl Pts',(-55.3580226952254,-106.648632271098,
175.985484945604));
#26412=CARTESIAN_POINT('Ctrl Pts',(-55.3480846831652,-106.555410501021,
174.763177441344));
#26413=CARTESIAN_POINT('Ctrl Pts',(-56.1975786630319,-106.370567538831,
173.89887555255));
#26414=CARTESIAN_POINT('Ctrl Pts',(-57.0470726428986,-106.18572457664,173.034573663757));
#26415=CARTESIAN_POINT('Ctrl Pts',(-58.2525549799674,-105.962930877251,
173.034573714903));
#26416=CARTESIAN_POINT('Ctrl Pts',(-59.4580373170363,-105.740137177862,
173.034573766048));
#26417=CARTESIAN_POINT('Ctrl Pts',(-60.3075312249805,-105.555294223339,
173.898875727171));
#26418=CARTESIAN_POINT('Ctrl Pts',(-61.1570251329247,-105.370451268815,
174.763177688294));
#26419=CARTESIAN_POINT('Ctrl Pts',(-61.1470870191508,-105.277229509582,
175.985485192554));
#26420=CARTESIAN_POINT('Ctrl Pts',(-61.1371489053769,-105.184007750348,
177.207792696815));
#26421=CARTESIAN_POINT('Ctrl Pts',(-60.2677787996762,-105.182407183228,
178.072094585608));
#26422=CARTESIAN_POINT('Ctrl Pts',(-59.3984086939755,-105.180806616108,
178.936396474401));
#26423=CARTESIAN_POINT('Ctrl Pts',(-58.1730502310727,-105.217156786186,
178.936396423256));
#26424=CARTESIAN_POINT('Ctrl Pts',(-56.9476917681698,-105.253506956265,
178.936396372111));
#26425=CARTESIAN_POINT('Ctrl Pts',(-56.0783217343916,-105.251906381477,
178.072094410988));
#26426=CARTESIAN_POINT('Ctrl Pts',(-55.2089517006133,-105.25030580669,177.207792449865));
#26427=CARTESIAN_POINT('Ctrl Pts',(-55.1990136885532,-105.157084036613,
175.985484945604));
#26428=CARTESIAN_POINT('Ctrl Pts',(-55.189075676493,-105.063862266536,174.763177441344));
#26429=CARTESIAN_POINT('Ctrl Pts',(-56.0385696563597,-104.879019304345,
173.89887555255));
#26430=CARTESIAN_POINT('Ctrl Pts',(-56.8880636362264,-104.694176342154,
173.034573663757));
#26431=CARTESIAN_POINT('Ctrl Pts',(-58.0935459732952,-104.471382642765,
173.034573714903));
#26432=CARTESIAN_POINT('Ctrl Pts',(-59.299028310364,-104.248588943376,173.034573766048));
#26433=CARTESIAN_POINT('Ctrl Pts',(-60.1485222183082,-104.063745988853,
173.898875727171));
#26434=CARTESIAN_POINT('Ctrl Pts',(-60.9980161262524,-103.87890303433,174.763177688294));
#26435=CARTESIAN_POINT('Ctrl Pts',(-60.9880780124786,-103.785681275096,
175.985485192554));
#26436=CARTESIAN_POINT('Ctrl Pts',(-60.9781398987047,-103.692459515862,
177.207792696815));
#26437=CARTESIAN_POINT('Ctrl Pts',(-60.108769793004,-103.690858948742,178.072094585608));
#26438=CARTESIAN_POINT('Ctrl Pts',(-59.2393996873033,-103.689258381622,
178.936396474401));
#26439=CARTESIAN_POINT('Ctrl Pts',(-58.0140412244004,-103.725608551701,
178.936396423256));
#26440=CARTESIAN_POINT('Ctrl Pts',(-56.7886827614976,-103.761958721779,
178.936396372111));
#26441=CARTESIAN_POINT('Ctrl Pts',(-55.9193127277193,-103.760358146992,
178.072094410988));
#26442=CARTESIAN_POINT('Ctrl Pts',(-55.0499426939411,-103.758757572204,
177.207792449865));
#26443=CARTESIAN_POINT('Ctrl Pts',(-55.0400046818809,-103.665535802127,
175.985484945604));
#26444=CARTESIAN_POINT('Ctrl Pts',(-55.0300666698208,-103.57231403205,174.763177441344));
#26445=CARTESIAN_POINT('Ctrl Pts',(-55.8795606496874,-103.387471069859,
173.89887555255));
#26446=CARTESIAN_POINT('Ctrl Pts',(-56.7290546295541,-103.202628107669,
173.034573663757));
#26447=CARTESIAN_POINT('Ctrl Pts',(-57.934536966623,-102.97983440828,173.034573714903));
#26448=CARTESIAN_POINT('Ctrl Pts',(-59.1400193036918,-102.757040708891,
173.034573766048));
#26449=CARTESIAN_POINT('Ctrl Pts',(-59.989513211636,-102.572197754367,173.898875727171));
#26450=CARTESIAN_POINT('Ctrl Pts',(-60.8390071195802,-102.387354799844,
174.763177688294));
#26451=CARTESIAN_POINT('Ctrl Pts',(-60.8290690058063,-102.29413304061,175.985485192554));
#26452=CARTESIAN_POINT('Ctrl Pts',(-60.8191308920325,-102.200911281377,
177.207792696815));
#26453=CARTESIAN_POINT('Ctrl Pts',(-59.9497607863318,-102.199310714257,
178.072094585608));
#26454=CARTESIAN_POINT('Ctrl Pts',(-59.0803906806311,-102.197710147137,
178.936396474401));
#26455=CARTESIAN_POINT('Ctrl Pts',(-57.8550322177282,-102.234060317215,
178.936396423256));
#26456=CARTESIAN_POINT('Ctrl Pts',(-56.6296737548253,-102.270410487293,
178.936396372111));
#26457=CARTESIAN_POINT('Ctrl Pts',(-55.7603037210471,-102.268809912506,
178.072094410988));
#26458=CARTESIAN_POINT('Ctrl Pts',(-54.8909336872689,-102.267209337719,
177.207792449865));
#26459=CARTESIAN_POINT('Ctrl Pts',(-54.8809956752087,-102.173987567642,
175.985484945604));
#26460=CARTESIAN_POINT('Ctrl Pts',(-54.8710576631486,-102.080765797565,
174.763177441344));
#26461=CARTESIAN_POINT('Ctrl Pts',(-55.7205516430152,-101.895922835374,
173.89887555255));
#26462=CARTESIAN_POINT('Ctrl Pts',(-56.5700456228819,-101.711079873183,
173.034573663757));
#26463=CARTESIAN_POINT('Ctrl Pts',(-57.7755279599507,-101.488286173794,
173.034573714903));
#26464=CARTESIAN_POINT('Ctrl Pts',(-58.9810102970196,-101.265492474405,
173.034573766048));
#26465=CARTESIAN_POINT('Ctrl Pts',(-59.8305042049638,-101.080649519882,
173.898875727171));
#26466=CARTESIAN_POINT('Ctrl Pts',(-60.679998112908,-100.895806565358,174.763177688294));
#26467=CARTESIAN_POINT('Ctrl Pts',(-60.6700599991341,-100.802584806125,
175.985485192554));
#26468=CARTESIAN_POINT('Ctrl Pts',(-60.6601218853602,-100.709363046891,
177.207792696815));
#26469=CARTESIAN_POINT('Ctrl Pts',(-59.7907517796595,-100.707762479771,
178.072094585608));
#26470=CARTESIAN_POINT('Ctrl Pts',(-58.9213816739588,-100.706161912651,
178.936396474401));
#26471=CARTESIAN_POINT('Ctrl Pts',(-57.696023211056,-100.742512082729,178.936396423256));
#26472=CARTESIAN_POINT('Ctrl Pts',(-56.4706647481531,-100.778862252808,
178.936396372111));
#26473=CARTESIAN_POINT('Ctrl Pts',(-55.6012947143749,-100.77726167802,178.072094410988));
#26474=CARTESIAN_POINT('Ctrl Pts',(-54.7319246805966,-100.775661103233,
177.207792449865));
#26475=CARTESIAN_POINT('Ctrl Pts',(-54.7219866685365,-100.682439333156,
175.985484945604));
#26476=CARTESIAN_POINT('Ctrl Pts',(-54.7120486564763,-100.589217563079,
174.763177441344));
#26477=CARTESIAN_POINT('Ctrl Pts',(-55.561542636343,-100.404374600888,173.89887555255));
#26478=CARTESIAN_POINT('Ctrl Pts',(-56.4110366162097,-100.219531638698,
173.034573663757));
#26479=CARTESIAN_POINT('Ctrl Pts',(-57.6165189532785,-99.9967379393085,
173.034573714903));
#26480=CARTESIAN_POINT('Ctrl Pts',(-58.8220012903473,-99.7739442399195,
173.034573766048));
#26481=CARTESIAN_POINT('Ctrl Pts',(-59.6714951982915,-99.5891012853962,
173.898875727171));
#26482=CARTESIAN_POINT('Ctrl Pts',(-60.5209891062358,-99.4042583308729,
174.763177688294));
#26483=CARTESIAN_POINT('Ctrl Pts',(-60.5110509924619,-99.3110365716392,
175.985485192554));
#26484=CARTESIAN_POINT('Ctrl Pts',(-60.501112878688,-99.2178148124055,177.207792696815));
#26485=CARTESIAN_POINT('Ctrl Pts',(-59.6317427729873,-99.2162142452855,
178.072094585608));
#26486=CARTESIAN_POINT('Ctrl Pts',(-58.7623726672866,-99.2146136781656,
178.936396474401));
#26487=CARTESIAN_POINT('Ctrl Pts',(-57.5370142043838,-99.2509638482439,
178.936396423256));
#26488=CARTESIAN_POINT('Ctrl Pts',(-56.3116557414809,-99.2873140183222,
178.936396372111));
#26489=CARTESIAN_POINT('Ctrl Pts',(-55.4422857077027,-99.2857134435348,
178.072094410988));
#26490=CARTESIAN_POINT('Ctrl Pts',(-54.5729156739244,-99.2841128687474,
177.207792449865));
#26491=CARTESIAN_POINT('Ctrl Pts',(-54.5629776618643,-99.1908910986704,
175.985484945604));
#26492=CARTESIAN_POINT('Ctrl Pts',(-54.5530396498041,-99.0976693285933,
174.763177441344));
#26493=CARTESIAN_POINT('Ctrl Pts',(-55.4025336296708,-98.9128263664026,
173.89887555255));
#26494=CARTESIAN_POINT('Ctrl Pts',(-56.2520276095374,-98.727983404212,173.034573663757));
#26495=CARTESIAN_POINT('Ctrl Pts',(-57.4575099466063,-98.5051897048229,
173.034573714903));
#26496=CARTESIAN_POINT('Ctrl Pts',(-58.6629922836751,-98.2823960054338,
173.034573766048));
#26497=CARTESIAN_POINT('Ctrl Pts',(-59.5124861916193,-98.0975530509106,
173.898875727171));
#26498=CARTESIAN_POINT('Ctrl Pts',(-60.3619800995635,-97.9127100963873,
174.763177688294));
#26499=CARTESIAN_POINT('Ctrl Pts',(-60.3520419857897,-97.8194883371536,
175.985485192554));
#26500=CARTESIAN_POINT('Ctrl Pts',(-60.3421038720158,-97.7262665779199,
177.207792696815));
#26501=CARTESIAN_POINT('Ctrl Pts',(-59.4727337663151,-97.7246660108,178.072094585608));
#26502=CARTESIAN_POINT('Ctrl Pts',(-58.6033636606144,-97.72306544368,178.936396474401));
#26503=CARTESIAN_POINT('Ctrl Pts',(-57.3780051977115,-97.7594156137583,
178.936396423256));
#26504=CARTESIAN_POINT('Ctrl Pts',(-56.1526467348087,-97.7957657838366,
178.936396372111));
#26505=CARTESIAN_POINT('Ctrl Pts',(-55.2832767010304,-97.7941652090492,
178.072094410988));
#26506=CARTESIAN_POINT('Ctrl Pts',(-56.1707931031902,-113.117197303651,
178.813912075476));
#26507=CARTESIAN_POINT('Ctrl Pts',(-54.9958834532485,-113.148169293224,
177.6423391512));
#26508=CARTESIAN_POINT('Ctrl Pts',(-54.9859454592686,-113.05494752122,175.985484901707));
#26509=CARTESIAN_POINT('Ctrl Pts',(-54.9760074652888,-112.961725749215,
174.328630652215));
#26510=CARTESIAN_POINT('Ctrl Pts',(-56.1310410868884,-112.744310219938,
173.157057825983));
#26511=CARTESIAN_POINT('Ctrl Pts',(-57.286074708488,-112.52689469066,171.985484999752));
#26512=CARTESIAN_POINT('Ctrl Pts',(-58.9236553326579,-112.258036427063,
171.985485069079));
#26513=CARTESIAN_POINT('Ctrl Pts',(-60.5612359568277,-111.989178163466,
171.985485138407));
#26514=CARTESIAN_POINT('Ctrl Pts',(-61.7162694809355,-111.771762644582,
173.157058062683));
#26515=CARTESIAN_POINT('Ctrl Pts',(-62.8713030050432,-111.554347125698,
174.328630986959));
#26516=CARTESIAN_POINT('Ctrl Pts',(-62.861364873189,-111.461125368392,175.985485236451));
#26517=CARTESIAN_POINT('Ctrl Pts',(-62.8514267413349,-111.367903611086,
177.642339485944));
#26518=CARTESIAN_POINT('Ctrl Pts',(-61.6765169939012,-111.398875611052,
178.813912312176));
#26519=CARTESIAN_POINT('Ctrl Pts',(-60.5016072464676,-111.429847611019,
179.985485138407));
#26520=CARTESIAN_POINT('Ctrl Pts',(-58.8441504964637,-111.512262345305,
179.985485069079));
#26521=CARTESIAN_POINT('Ctrl Pts',(-57.1866937464598,-111.594677079592,
179.985484999752));
#26522=CARTESIAN_POINT('Ctrl Pts',(-56.011784096518,-111.625649069165,178.813912075476));
#26523=CARTESIAN_POINT('Ctrl Pts',(-54.8368744465762,-111.656621058739,
177.6423391512));
#26524=CARTESIAN_POINT('Ctrl Pts',(-54.8269364525964,-111.563399286734,
175.985484901707));
#26525=CARTESIAN_POINT('Ctrl Pts',(-54.8169984586165,-111.47017751473,174.328630652215));
#26526=CARTESIAN_POINT('Ctrl Pts',(-55.9720320802161,-111.252761985452,
173.157057825983));
#26527=CARTESIAN_POINT('Ctrl Pts',(-57.1270657018158,-111.035346456175,
171.985484999752));
#26528=CARTESIAN_POINT('Ctrl Pts',(-58.7646463259856,-110.766488192578,
171.985485069079));
#26529=CARTESIAN_POINT('Ctrl Pts',(-60.4022269501555,-110.497629928981,
171.985485138407));
#26530=CARTESIAN_POINT('Ctrl Pts',(-61.5572604742632,-110.280214410097,
173.157058062683));
#26531=CARTESIAN_POINT('Ctrl Pts',(-62.712293998371,-110.062798891212,174.328630986959));
#26532=CARTESIAN_POINT('Ctrl Pts',(-62.7023558665168,-109.969577133906,
175.985485236451));
#26533=CARTESIAN_POINT('Ctrl Pts',(-62.6924177346626,-109.8763553766,177.642339485944));
#26534=CARTESIAN_POINT('Ctrl Pts',(-61.517507987229,-109.907327376567,178.813912312176));
#26535=CARTESIAN_POINT('Ctrl Pts',(-60.3425982397954,-109.938299376534,
179.985485138407));
#26536=CARTESIAN_POINT('Ctrl Pts',(-58.6851414897915,-110.02071411082,179.985485069079));
#26537=CARTESIAN_POINT('Ctrl Pts',(-57.0276847397876,-110.103128845106,
179.985484999752));
#26538=CARTESIAN_POINT('Ctrl Pts',(-55.8527750898458,-110.13410083468,178.813912075476));
#26539=CARTESIAN_POINT('Ctrl Pts',(-54.677865439904,-110.165072824253,177.6423391512));
#26540=CARTESIAN_POINT('Ctrl Pts',(-54.6679274459242,-110.071851052249,
175.985484901707));
#26541=CARTESIAN_POINT('Ctrl Pts',(-54.6579894519443,-109.978629280244,
174.328630652215));
#26542=CARTESIAN_POINT('Ctrl Pts',(-55.8130230735439,-109.761213750967,
173.157057825983));
#26543=CARTESIAN_POINT('Ctrl Pts',(-56.9680566951435,-109.543798221689,
171.985484999752));
#26544=CARTESIAN_POINT('Ctrl Pts',(-58.6056373193134,-109.274939958092,
171.985485069079));
#26545=CARTESIAN_POINT('Ctrl Pts',(-60.2432179434833,-109.006081694495,
171.985485138407));
#26546=CARTESIAN_POINT('Ctrl Pts',(-61.398251467591,-108.788666175611,173.157058062683));
#26547=CARTESIAN_POINT('Ctrl Pts',(-62.5532849916988,-108.571250656727,
174.328630986959));
#26548=CARTESIAN_POINT('Ctrl Pts',(-62.5433468598446,-108.478028899421,
175.985485236451));
#26549=CARTESIAN_POINT('Ctrl Pts',(-62.5334087279904,-108.384807142114,
177.642339485944));
#26550=CARTESIAN_POINT('Ctrl Pts',(-61.3584989805568,-108.415779142081,
178.813912312176));
#26551=CARTESIAN_POINT('Ctrl Pts',(-60.1835892331231,-108.446751142048,
179.985485138407));
#26552=CARTESIAN_POINT('Ctrl Pts',(-58.5261324831192,-108.529165876334,
179.985485069079));
#26553=CARTESIAN_POINT('Ctrl Pts',(-56.8686757331153,-108.611580610621,
179.985484999752));
#26554=CARTESIAN_POINT('Ctrl Pts',(-55.6937660831736,-108.642552600194,
178.813912075476));
#26555=CARTESIAN_POINT('Ctrl Pts',(-54.5188564332318,-108.673524589768,
177.6423391512));
#26556=CARTESIAN_POINT('Ctrl Pts',(-54.5089184392519,-108.580302817763,
175.985484901707));
#26557=CARTESIAN_POINT('Ctrl Pts',(-54.4989804452721,-108.487081045759,
174.328630652215));
#26558=CARTESIAN_POINT('Ctrl Pts',(-55.6540140668717,-108.269665516481,
173.157057825983));
#26559=CARTESIAN_POINT('Ctrl Pts',(-56.8090476884713,-108.052249987204,
171.985484999752));
#26560=CARTESIAN_POINT('Ctrl Pts',(-58.4466283126412,-107.783391723607,
171.985485069079));
#26561=CARTESIAN_POINT('Ctrl Pts',(-60.084208936811,-107.51453346001,171.985485138407));
#26562=CARTESIAN_POINT('Ctrl Pts',(-61.2392424609188,-107.297117941125,
173.157058062683));
#26563=CARTESIAN_POINT('Ctrl Pts',(-62.3942759850265,-107.079702422241,
174.328630986959));
#26564=CARTESIAN_POINT('Ctrl Pts',(-62.3843378531723,-106.986480664935,
175.985485236451));
#26565=CARTESIAN_POINT('Ctrl Pts',(-62.3743997213182,-106.893258907629,
177.642339485944));
#26566=CARTESIAN_POINT('Ctrl Pts',(-61.1994899738845,-106.924230907596,
178.813912312176));
#26567=CARTESIAN_POINT('Ctrl Pts',(-60.0245802264509,-106.955202907562,
179.985485138407));
#26568=CARTESIAN_POINT('Ctrl Pts',(-58.367123476447,-107.037617641849,179.985485069079));
#26569=CARTESIAN_POINT('Ctrl Pts',(-56.7096667264431,-107.120032376135,
179.985484999752));
#26570=CARTESIAN_POINT('Ctrl Pts',(-55.5347570765013,-107.151004365708,
178.813912075476));
#26571=CARTESIAN_POINT('Ctrl Pts',(-54.3598474265596,-107.181976355282,
177.6423391512));
#26572=CARTESIAN_POINT('Ctrl Pts',(-54.3499094325797,-107.088754583277,
175.985484901707));
#26573=CARTESIAN_POINT('Ctrl Pts',(-54.3399714385998,-106.995532811273,
174.328630652215));
#26574=CARTESIAN_POINT('Ctrl Pts',(-55.4950050601995,-106.778117281995,
173.157057825983));
#26575=CARTESIAN_POINT('Ctrl Pts',(-56.6500386817991,-106.560701752718,
171.985484999752));
#26576=CARTESIAN_POINT('Ctrl Pts',(-58.2876193059689,-106.291843489121,
171.985485069079));
#26577=CARTESIAN_POINT('Ctrl Pts',(-59.9251999301388,-106.022985225524,
171.985485138407));
#26578=CARTESIAN_POINT('Ctrl Pts',(-61.0802334542465,-105.80556970664,173.157058062683));
#26579=CARTESIAN_POINT('Ctrl Pts',(-62.2352669783543,-105.588154187756,
174.328630986959));
#26580=CARTESIAN_POINT('Ctrl Pts',(-62.2253288465001,-105.494932430449,
175.985485236451));
#26581=CARTESIAN_POINT('Ctrl Pts',(-62.2153907146459,-105.401710673143,
177.642339485944));
#26582=CARTESIAN_POINT('Ctrl Pts',(-61.0404809672123,-105.43268267311,178.813912312176));
#26583=CARTESIAN_POINT('Ctrl Pts',(-59.8655712197787,-105.463654673077,
179.985485138407));
#26584=CARTESIAN_POINT('Ctrl Pts',(-58.2081144697748,-105.546069407363,
179.985485069079));
#26585=CARTESIAN_POINT('Ctrl Pts',(-56.5506577197709,-105.628484141649,
179.985484999752));
#26586=CARTESIAN_POINT('Ctrl Pts',(-55.3757480698291,-105.659456131223,
178.813912075476));
#26587=CARTESIAN_POINT('Ctrl Pts',(-54.2008384198873,-105.690428120796,
177.6423391512));
#26588=CARTESIAN_POINT('Ctrl Pts',(-54.1909004259075,-105.597206348792,
175.985484901707));
#26589=CARTESIAN_POINT('Ctrl Pts',(-54.1809624319276,-105.503984576787,
174.328630652215));
#26590=CARTESIAN_POINT('Ctrl Pts',(-55.3359960535272,-105.28656904751,173.157057825983));
#26591=CARTESIAN_POINT('Ctrl Pts',(-56.4910296751268,-105.069153518232,
171.985484999752));
#26592=CARTESIAN_POINT('Ctrl Pts',(-58.1286102992967,-104.800295254635,
171.985485069079));
#26593=CARTESIAN_POINT('Ctrl Pts',(-59.7661909234666,-104.531436991038,
171.985485138407));
#26594=CARTESIAN_POINT('Ctrl Pts',(-60.9212244475743,-104.314021472154,
173.157058062683));
#26595=CARTESIAN_POINT('Ctrl Pts',(-62.0762579716821,-104.09660595327,174.328630986959));
#26596=CARTESIAN_POINT('Ctrl Pts',(-62.0663198398279,-104.003384195964,
175.985485236451));
#26597=CARTESIAN_POINT('Ctrl Pts',(-62.0563817079737,-103.910162438658,
177.642339485944));
#26598=CARTESIAN_POINT('Ctrl Pts',(-60.8814719605401,-103.941134438624,
178.813912312176));
#26599=CARTESIAN_POINT('Ctrl Pts',(-59.7065622131064,-103.972106438591,
179.985485138407));
#26600=CARTESIAN_POINT('Ctrl Pts',(-58.0491054631025,-104.054521172878,
179.985485069079));
#26601=CARTESIAN_POINT('Ctrl Pts',(-56.3916487130987,-104.136935907164,
179.985484999752));
#26602=CARTESIAN_POINT('Ctrl Pts',(-55.2167390631569,-104.167907896737,
178.813912075476));
#26603=CARTESIAN_POINT('Ctrl Pts',(-54.0418294132151,-104.198879886311,
177.6423391512));
#26604=CARTESIAN_POINT('Ctrl Pts',(-54.0318914192353,-104.105658114306,
175.985484901707));
#26605=CARTESIAN_POINT('Ctrl Pts',(-54.0219534252554,-104.012436342302,
174.328630652215));
#26606=CARTESIAN_POINT('Ctrl Pts',(-55.176987046855,-103.795020813024,173.157057825983));
#26607=CARTESIAN_POINT('Ctrl Pts',(-56.3320206684546,-103.577605283747,
171.985484999752));
#26608=CARTESIAN_POINT('Ctrl Pts',(-57.9696012926245,-103.30874702015,171.985485069079));
#26609=CARTESIAN_POINT('Ctrl Pts',(-59.6071819167943,-103.039888756553,
171.985485138407));
#26610=CARTESIAN_POINT('Ctrl Pts',(-60.7622154409021,-102.822473237669,
173.157058062683));
#26611=CARTESIAN_POINT('Ctrl Pts',(-61.9172489650099,-102.605057718784,
174.328630986959));
#26612=CARTESIAN_POINT('Ctrl Pts',(-61.9073108331557,-102.511835961478,
175.985485236451));
#26613=CARTESIAN_POINT('Ctrl Pts',(-61.8973727013015,-102.418614204172,
177.642339485944));
#26614=CARTESIAN_POINT('Ctrl Pts',(-60.7224629538678,-102.449586204139,
178.813912312176));
#26615=CARTESIAN_POINT('Ctrl Pts',(-59.5475532064342,-102.480558204106,
179.985485138407));
#26616=CARTESIAN_POINT('Ctrl Pts',(-57.8900964564303,-102.562972938392,
179.985485069079));
#26617=CARTESIAN_POINT('Ctrl Pts',(-56.2326397064264,-102.645387672678,
179.985484999752));
#26618=CARTESIAN_POINT('Ctrl Pts',(-55.0577300564847,-102.676359662252,
178.813912075476));
#26619=CARTESIAN_POINT('Ctrl Pts',(-53.8828204065429,-102.707331651825,
177.6423391512));
#26620=CARTESIAN_POINT('Ctrl Pts',(-53.872882412563,-102.614109879821,175.985484901707));
#26621=CARTESIAN_POINT('Ctrl Pts',(-53.8629444185832,-102.520888107816,
174.328630652215));
#26622=CARTESIAN_POINT('Ctrl Pts',(-55.0179780401828,-102.303472578539,
173.157057825983));
#26623=CARTESIAN_POINT('Ctrl Pts',(-56.1730116617824,-102.086057049261,
171.985484999752));
#26624=CARTESIAN_POINT('Ctrl Pts',(-57.8105922859523,-101.817198785664,
171.985485069079));
#26625=CARTESIAN_POINT('Ctrl Pts',(-59.4481729101221,-101.548340522067,
171.985485138407));
#26626=CARTESIAN_POINT('Ctrl Pts',(-60.6032064342299,-101.330925003183,
173.157058062683));
#26627=CARTESIAN_POINT('Ctrl Pts',(-61.7582399583376,-101.113509484299,
174.328630986959));
#26628=CARTESIAN_POINT('Ctrl Pts',(-61.7483018264834,-101.020287726993,
175.985485236451));
#26629=CARTESIAN_POINT('Ctrl Pts',(-61.7383636946293,-100.927065969686,
177.642339485944));
#26630=CARTESIAN_POINT('Ctrl Pts',(-60.5634539471956,-100.958037969653,
178.813912312176));
#26631=CARTESIAN_POINT('Ctrl Pts',(-59.388544199762,-100.98900996962,179.985485138407));
#26632=CARTESIAN_POINT('Ctrl Pts',(-57.7310874497581,-101.071424703906,
179.985485069079));
#26633=CARTESIAN_POINT('Ctrl Pts',(-56.0736306997542,-101.153839438193,
179.985484999752));
#26634=CARTESIAN_POINT('Ctrl Pts',(-54.8987210498124,-101.184811427766,
178.813912075476));
#26635=CARTESIAN_POINT('Ctrl Pts',(-53.7238113998707,-101.21578341734,177.6423391512));
#26636=CARTESIAN_POINT('Ctrl Pts',(-53.7138734058908,-101.122561645335,
175.985484901707));
#26637=CARTESIAN_POINT('Ctrl Pts',(-53.7039354119109,-101.029339873331,
174.328630652215));
#26638=CARTESIAN_POINT('Ctrl Pts',(-54.8589690335105,-100.811924344053,
173.157057825983));
#26639=CARTESIAN_POINT('Ctrl Pts',(-56.0140026551102,-100.594508814776,
171.985484999752));
#26640=CARTESIAN_POINT('Ctrl Pts',(-57.65158327928,-100.325650551179,171.985485069079));
#26641=CARTESIAN_POINT('Ctrl Pts',(-59.2891639034499,-100.056792287582,
171.985485138407));
#26642=CARTESIAN_POINT('Ctrl Pts',(-60.4441974275576,-99.8393767686974,
173.157058062683));
#26643=CARTESIAN_POINT('Ctrl Pts',(-61.5992309516654,-99.6219612498133,
174.328630986959));
#26644=CARTESIAN_POINT('Ctrl Pts',(-61.5892928198112,-99.528739492507,175.985485236451));
#26645=CARTESIAN_POINT('Ctrl Pts',(-61.579354687957,-99.4355177352008,177.642339485944));
#26646=CARTESIAN_POINT('Ctrl Pts',(-60.4044449405234,-99.4664897351676,
178.813912312176));
#26647=CARTESIAN_POINT('Ctrl Pts',(-59.2295351930898,-99.4974617351344,
179.985485138407));
#26648=CARTESIAN_POINT('Ctrl Pts',(-57.5720784430859,-99.5798764694207,
179.985485069079));
#26649=CARTESIAN_POINT('Ctrl Pts',(-55.914621693082,-99.662291203707,179.985484999752));
#26650=CARTESIAN_POINT('Ctrl Pts',(-54.7397120431402,-99.6932631932805,
178.813912075476));
#26651=CARTESIAN_POINT('Ctrl Pts',(-53.5648023931984,-99.724235182854,177.6423391512));
#26652=CARTESIAN_POINT('Ctrl Pts',(-53.5548643992186,-99.6310134108495,
175.985484901707));
#26653=CARTESIAN_POINT('Ctrl Pts',(-53.5449264052387,-99.5377916388449,
174.328630652215));
#26654=CARTESIAN_POINT('Ctrl Pts',(-54.6999600268383,-99.3203761095675,
173.157057825983));
#26655=CARTESIAN_POINT('Ctrl Pts',(-55.8549936484379,-99.10296058029,171.985484999752));
#26656=CARTESIAN_POINT('Ctrl Pts',(-57.4925742726078,-98.834102316693,171.985485069079));
#26657=CARTESIAN_POINT('Ctrl Pts',(-59.1301548967777,-98.565244053096,171.985485138407));
#26658=CARTESIAN_POINT('Ctrl Pts',(-60.2851884208854,-98.3478285342118,
173.157058062683));
#26659=CARTESIAN_POINT('Ctrl Pts',(-61.4402219449932,-98.1304130153276,
174.328630986959));
#26660=CARTESIAN_POINT('Ctrl Pts',(-61.430283813139,-98.0371912580215,175.985485236451));
#26661=CARTESIAN_POINT('Ctrl Pts',(-61.4203456812848,-97.9439695007152,
177.642339485944));
#26662=CARTESIAN_POINT('Ctrl Pts',(-60.2454359338512,-97.974941500682,178.813912312176));
#26663=CARTESIAN_POINT('Ctrl Pts',(-59.0705261864175,-98.0059135006488,
179.985485138407));
#26664=CARTESIAN_POINT('Ctrl Pts',(-57.4130694364136,-98.0883282349351,
179.985485069079));
#26665=CARTESIAN_POINT('Ctrl Pts',(-55.7556126864097,-98.1707429692214,
179.985484999752));
#26666=CARTESIAN_POINT('Ctrl Pts',(-54.580703036468,-98.2017149587949,178.813912075476));
#26667=CARTESIAN_POINT('Ctrl Pts',(-61.6536146045897,-108.409937955922,
178.485485069079));
#26668=CARTESIAN_POINT('Ctrl Pts',(-61.5150424002329,-108.411652473799,
178.657813499464));
#26669=CARTESIAN_POINT('Ctrl Pts',(-61.3584989805568,-108.415779142081,
178.813912312176));
#26670=CARTESIAN_POINT('Ctrl Pts',(-60.1835892331231,-108.446751142048,
179.985485138407));
#26671=CARTESIAN_POINT('Ctrl Pts',(-58.5261324831192,-108.529165876334,
179.985485069079));
#26672=CARTESIAN_POINT('Ctrl Pts',(-56.8686757331153,-108.611580610621,
179.985484999752));
#26673=CARTESIAN_POINT('Ctrl Pts',(-55.6937660831736,-108.642552600194,
178.813912075476));
#26674=CARTESIAN_POINT('Ctrl Pts',(-54.5188564332318,-108.673524589768,
177.6423391512));
#26675=CARTESIAN_POINT('Ctrl Pts',(-54.5089184392519,-108.580302817763,
175.985484901707));
#26676=CARTESIAN_POINT('Ctrl Pts',(-54.4989804452721,-108.487081045759,
174.328630652215));
#26677=CARTESIAN_POINT('Ctrl Pts',(-55.6540140668717,-108.269665516481,
173.157057825983));
#26678=CARTESIAN_POINT('Ctrl Pts',(-56.8090476884713,-108.052249987204,
171.985484999752));
#26679=CARTESIAN_POINT('Ctrl Pts',(-58.4466283126412,-107.783391723607,
171.985485069079));
#26680=CARTESIAN_POINT('Ctrl Pts',(-60.084208936811,-107.51453346001,171.985485138407));
#26681=CARTESIAN_POINT('Ctrl Pts',(-61.2392424609188,-107.297117941125,
173.157058062683));
#26682=CARTESIAN_POINT('Ctrl Pts',(-61.3931374818719,-107.268149807183,
173.313156769748));
#26683=CARTESIAN_POINT('Ctrl Pts',(-61.5289566858427,-107.240612378001,
173.485485069079));
#26684=CARTESIAN_POINT('Ctrl Pts',(-56.1707931031902,-113.117197303651,
178.813912075476));
#26685=CARTESIAN_POINT('Ctrl Pts',(-54.9958834532485,-113.148169293224,
177.6423391512));
#26686=CARTESIAN_POINT('Ctrl Pts',(-54.9859454592686,-113.05494752122,175.985484901707));
#26687=CARTESIAN_POINT('Ctrl Pts',(-54.9760074652888,-112.961725749215,
174.328630652215));
#26688=CARTESIAN_POINT('Ctrl Pts',(-56.1310410868884,-112.744310219938,
173.157057825983));
#26689=CARTESIAN_POINT('Ctrl Pts',(-57.286074708488,-112.52689469066,171.985484999752));
#26690=CARTESIAN_POINT('Ctrl Pts',(-58.9236553326578,-112.258036427063,
171.985485069079));
#26691=CARTESIAN_POINT('Ctrl Pts',(-60.5612359568277,-111.989178163466,
171.985485138407));
#26692=CARTESIAN_POINT('Ctrl Pts',(-61.7162694809355,-111.771762644582,
173.157058062683));
#26693=CARTESIAN_POINT('Ctrl Pts',(-62.8713030050432,-111.554347125698,
174.328630986959));
#26694=CARTESIAN_POINT('Ctrl Pts',(-62.861364873189,-111.461125368392,175.985485236451));
#26695=CARTESIAN_POINT('Ctrl Pts',(-62.8514267413349,-111.367903611086,
177.642339485944));
#26696=CARTESIAN_POINT('Ctrl Pts',(-61.6765169939012,-111.398875611052,
178.813912312176));
#26697=CARTESIAN_POINT('Ctrl Pts',(-60.5016072464676,-111.429847611019,
179.985485138407));
#26698=CARTESIAN_POINT('Ctrl Pts',(-58.8441504964637,-111.512262345305,
179.985485069079));
#26699=CARTESIAN_POINT('Ctrl Pts',(-57.1866937464598,-111.594677079592,
179.985484999752));
#26700=CARTESIAN_POINT('Ctrl Pts',(-56.011784096518,-111.625649069165,178.813912075476));
#26701=CARTESIAN_POINT('Ctrl Pts',(-54.8368744465763,-111.656621058739,
177.6423391512));
#26702=CARTESIAN_POINT('Ctrl Pts',(-54.8269364525964,-111.563399286734,
175.985484901707));
#26703=CARTESIAN_POINT('Ctrl Pts',(-54.8169984586165,-111.47017751473,174.328630652215));
#26704=CARTESIAN_POINT('Ctrl Pts',(-55.9720320802161,-111.252761985452,
173.157057825983));
#26705=CARTESIAN_POINT('Ctrl Pts',(-57.1270657018158,-111.035346456175,
171.985484999752));
#26706=CARTESIAN_POINT('Ctrl Pts',(-58.7646463259856,-110.766488192578,
171.985485069079));
#26707=CARTESIAN_POINT('Ctrl Pts',(-60.4022269501555,-110.497629928981,
171.985485138407));
#26708=CARTESIAN_POINT('Ctrl Pts',(-61.5572604742632,-110.280214410097,
173.157058062683));
#26709=CARTESIAN_POINT('Ctrl Pts',(-62.712293998371,-110.062798891212,174.328630986959));
#26710=CARTESIAN_POINT('Ctrl Pts',(-62.7023558665168,-109.969577133906,
175.985485236451));
#26711=CARTESIAN_POINT('Ctrl Pts',(-62.6924177346626,-109.8763553766,177.642339485944));
#26712=CARTESIAN_POINT('Ctrl Pts',(-61.517507987229,-109.907327376567,178.813912312176));
#26713=CARTESIAN_POINT('Ctrl Pts',(-60.3425982397954,-109.938299376534,
179.985485138407));
#26714=CARTESIAN_POINT('Ctrl Pts',(-58.6851414897915,-110.02071411082,179.985485069079));
#26715=CARTESIAN_POINT('Ctrl Pts',(-57.0276847397876,-110.103128845106,
179.985484999752));
#26716=CARTESIAN_POINT('Ctrl Pts',(-55.8527750898458,-110.13410083468,178.813912075476));
#26717=CARTESIAN_POINT('Ctrl Pts',(-54.677865439904,-110.165072824253,177.6423391512));
#26718=CARTESIAN_POINT('Ctrl Pts',(-54.6679274459242,-110.071851052249,
175.985484901707));
#26719=CARTESIAN_POINT('Ctrl Pts',(-54.6579894519443,-109.978629280244,
174.328630652215));
#26720=CARTESIAN_POINT('Ctrl Pts',(-55.8130230735439,-109.761213750967,
173.157057825983));
#26721=CARTESIAN_POINT('Ctrl Pts',(-56.9680566951435,-109.543798221689,
171.985484999752));
#26722=CARTESIAN_POINT('Ctrl Pts',(-58.6056373193134,-109.274939958092,
171.985485069079));
#26723=CARTESIAN_POINT('Ctrl Pts',(-60.2432179434833,-109.006081694495,
171.985485138407));
#26724=CARTESIAN_POINT('Ctrl Pts',(-61.398251467591,-108.788666175611,173.157058062683));
#26725=CARTESIAN_POINT('Ctrl Pts',(-62.5532849916988,-108.571250656727,
174.328630986959));
#26726=CARTESIAN_POINT('Ctrl Pts',(-62.5433468598446,-108.478028899421,
175.985485236451));
#26727=CARTESIAN_POINT('Ctrl Pts',(-62.5334087279904,-108.384807142114,
177.642339485944));
#26728=CARTESIAN_POINT('Ctrl Pts',(-61.3584989805568,-108.415779142081,
178.813912312176));
#26729=CARTESIAN_POINT('Ctrl Pts',(-60.1835892331231,-108.446751142048,
179.985485138407));
#26730=CARTESIAN_POINT('Ctrl Pts',(-58.5261324831192,-108.529165876334,
179.985485069079));
#26731=CARTESIAN_POINT('Ctrl Pts',(-56.8686757331153,-108.611580610621,
179.985484999752));
#26732=CARTESIAN_POINT('Ctrl Pts',(-55.6937660831736,-108.642552600194,
178.813912075476));
#26733=CARTESIAN_POINT('Ctrl Pts',(-54.5188564332318,-108.673524589768,
177.6423391512));
#26734=CARTESIAN_POINT('Ctrl Pts',(-54.5089184392519,-108.580302817763,
175.985484901707));
#26735=CARTESIAN_POINT('Ctrl Pts',(-54.4989804452721,-108.487081045759,
174.328630652215));
#26736=CARTESIAN_POINT('Ctrl Pts',(-55.6540140668717,-108.269665516481,
173.157057825983));
#26737=CARTESIAN_POINT('Ctrl Pts',(-56.8090476884713,-108.052249987204,
171.985484999752));
#26738=CARTESIAN_POINT('Ctrl Pts',(-58.4466283126412,-107.783391723607,
171.985485069079));
#26739=CARTESIAN_POINT('Ctrl Pts',(-60.084208936811,-107.51453346001,171.985485138407));
#26740=CARTESIAN_POINT('Ctrl Pts',(-61.2392424609188,-107.297117941125,
173.157058062683));
#26741=CARTESIAN_POINT('Ctrl Pts',(-62.3942759850265,-107.079702422241,
174.328630986959));
#26742=CARTESIAN_POINT('Ctrl Pts',(-62.3843378531723,-106.986480664935,
175.985485236451));
#26743=CARTESIAN_POINT('Ctrl Pts',(-62.3743997213182,-106.893258907629,
177.642339485944));
#26744=CARTESIAN_POINT('Ctrl Pts',(-61.1994899738845,-106.924230907596,
178.813912312176));
#26745=CARTESIAN_POINT('Ctrl Pts',(-60.0245802264509,-106.955202907562,
179.985485138407));
#26746=CARTESIAN_POINT('Ctrl Pts',(-58.367123476447,-107.037617641849,179.985485069079));
#26747=CARTESIAN_POINT('Ctrl Pts',(-56.7096667264431,-107.120032376135,
179.985484999752));
#26748=CARTESIAN_POINT('Ctrl Pts',(-55.5347570765013,-107.151004365708,
178.813912075476));
#26749=CARTESIAN_POINT('Ctrl Pts',(-54.3598474265596,-107.181976355282,
177.6423391512));
#26750=CARTESIAN_POINT('Ctrl Pts',(-54.3499094325797,-107.088754583277,
175.985484901707));
#26751=CARTESIAN_POINT('Ctrl Pts',(-54.3399714385998,-106.995532811273,
174.328630652215));
#26752=CARTESIAN_POINT('Ctrl Pts',(-55.4950050601995,-106.778117281995,
173.157057825983));
#26753=CARTESIAN_POINT('Ctrl Pts',(-56.6500386817991,-106.560701752718,
171.985484999752));
#26754=CARTESIAN_POINT('Ctrl Pts',(-58.2876193059689,-106.291843489121,
171.985485069079));
#26755=CARTESIAN_POINT('Ctrl Pts',(-59.9251999301388,-106.022985225524,
171.985485138407));
#26756=CARTESIAN_POINT('Ctrl Pts',(-61.0802334542465,-105.80556970664,173.157058062683));
#26757=CARTESIAN_POINT('Ctrl Pts',(-62.2352669783543,-105.588154187756,
174.328630986959));
#26758=CARTESIAN_POINT('Ctrl Pts',(-62.2253288465001,-105.494932430449,
175.985485236451));
#26759=CARTESIAN_POINT('Ctrl Pts',(-62.2153907146459,-105.401710673143,
177.642339485944));
#26760=CARTESIAN_POINT('Ctrl Pts',(-61.0404809672123,-105.43268267311,178.813912312176));
#26761=CARTESIAN_POINT('Ctrl Pts',(-59.8655712197787,-105.463654673077,
179.985485138407));
#26762=CARTESIAN_POINT('Ctrl Pts',(-58.2081144697748,-105.546069407363,
179.985485069079));
#26763=CARTESIAN_POINT('Ctrl Pts',(-56.5506577197709,-105.628484141649,
179.985484999752));
#26764=CARTESIAN_POINT('Ctrl Pts',(-55.3757480698291,-105.659456131223,
178.813912075476));
#26765=CARTESIAN_POINT('Ctrl Pts',(-54.2008384198873,-105.690428120796,
177.6423391512));
#26766=CARTESIAN_POINT('Ctrl Pts',(-54.1909004259075,-105.597206348792,
175.985484901707));
#26767=CARTESIAN_POINT('Ctrl Pts',(-54.1809624319276,-105.503984576787,
174.328630652215));
#26768=CARTESIAN_POINT('Ctrl Pts',(-55.3359960535272,-105.28656904751,173.157057825983));
#26769=CARTESIAN_POINT('Ctrl Pts',(-56.4910296751268,-105.069153518232,
171.985484999752));
#26770=CARTESIAN_POINT('Ctrl Pts',(-58.1286102992967,-104.800295254635,
171.985485069079));
#26771=CARTESIAN_POINT('Ctrl Pts',(-59.7661909234666,-104.531436991038,
171.985485138407));
#26772=CARTESIAN_POINT('Ctrl Pts',(-60.9212244475743,-104.314021472154,
173.157058062683));
#26773=CARTESIAN_POINT('Ctrl Pts',(-62.0762579716821,-104.09660595327,174.328630986959));
#26774=CARTESIAN_POINT('Ctrl Pts',(-62.0663198398279,-104.003384195964,
175.985485236451));
#26775=CARTESIAN_POINT('Ctrl Pts',(-62.0563817079737,-103.910162438658,
177.642339485944));
#26776=CARTESIAN_POINT('Ctrl Pts',(-60.8814719605401,-103.941134438624,
178.813912312176));
#26777=CARTESIAN_POINT('Ctrl Pts',(-59.7065622131064,-103.972106438591,
179.985485138407));
#26778=CARTESIAN_POINT('Ctrl Pts',(-58.0491054631025,-104.054521172878,
179.985485069079));
#26779=CARTESIAN_POINT('Ctrl Pts',(-56.3916487130987,-104.136935907164,
179.985484999752));
#26780=CARTESIAN_POINT('Ctrl Pts',(-55.2167390631569,-104.167907896737,
178.813912075476));
#26781=CARTESIAN_POINT('Ctrl Pts',(-54.0418294132151,-104.198879886311,
177.6423391512));
#26782=CARTESIAN_POINT('Ctrl Pts',(-54.0318914192353,-104.105658114306,
175.985484901707));
#26783=CARTESIAN_POINT('Ctrl Pts',(-54.0219534252554,-104.012436342302,
174.328630652215));
#26784=CARTESIAN_POINT('Ctrl Pts',(-55.176987046855,-103.795020813024,173.157057825983));
#26785=CARTESIAN_POINT('Ctrl Pts',(-56.3320206684546,-103.577605283747,
171.985484999752));
#26786=CARTESIAN_POINT('Ctrl Pts',(-57.9696012926245,-103.30874702015,171.985485069079));
#26787=CARTESIAN_POINT('Ctrl Pts',(-59.6071819167943,-103.039888756553,
171.985485138407));
#26788=CARTESIAN_POINT('Ctrl Pts',(-60.7622154409021,-102.822473237669,
173.157058062683));
#26789=CARTESIAN_POINT('Ctrl Pts',(-61.9172489650099,-102.605057718784,
174.328630986959));
#26790=CARTESIAN_POINT('Ctrl Pts',(-61.9073108331557,-102.511835961478,
175.985485236451));
#26791=CARTESIAN_POINT('Ctrl Pts',(-61.8973727013015,-102.418614204172,
177.642339485944));
#26792=CARTESIAN_POINT('Ctrl Pts',(-60.7224629538678,-102.449586204139,
178.813912312176));
#26793=CARTESIAN_POINT('Ctrl Pts',(-59.5475532064342,-102.480558204106,
179.985485138407));
#26794=CARTESIAN_POINT('Ctrl Pts',(-57.8900964564303,-102.562972938392,
179.985485069079));
#26795=CARTESIAN_POINT('Ctrl Pts',(-56.2326397064264,-102.645387672678,
179.985484999752));
#26796=CARTESIAN_POINT('Ctrl Pts',(-55.0577300564847,-102.676359662252,
178.813912075476));
#26797=CARTESIAN_POINT('Ctrl Pts',(-53.8828204065429,-102.707331651825,
177.6423391512));
#26798=CARTESIAN_POINT('Ctrl Pts',(-53.872882412563,-102.614109879821,175.985484901707));
#26799=CARTESIAN_POINT('Ctrl Pts',(-53.8629444185832,-102.520888107816,
174.328630652215));
#26800=CARTESIAN_POINT('Ctrl Pts',(-55.0179780401828,-102.303472578539,
173.157057825983));
#26801=CARTESIAN_POINT('Ctrl Pts',(-56.1730116617824,-102.086057049261,
171.985484999752));
#26802=CARTESIAN_POINT('Ctrl Pts',(-57.8105922859523,-101.817198785664,
171.985485069079));
#26803=CARTESIAN_POINT('Ctrl Pts',(-59.4481729101221,-101.548340522067,
171.985485138407));
#26804=CARTESIAN_POINT('Ctrl Pts',(-60.6032064342299,-101.330925003183,
173.157058062683));
#26805=CARTESIAN_POINT('Ctrl Pts',(-61.7582399583376,-101.113509484299,
174.328630986959));
#26806=CARTESIAN_POINT('Ctrl Pts',(-61.7483018264834,-101.020287726993,
175.985485236451));
#26807=CARTESIAN_POINT('Ctrl Pts',(-61.7383636946293,-100.927065969686,
177.642339485944));
#26808=CARTESIAN_POINT('Ctrl Pts',(-60.5634539471956,-100.958037969653,
178.813912312176));
#26809=CARTESIAN_POINT('Ctrl Pts',(-59.388544199762,-100.98900996962,179.985485138407));
#26810=CARTESIAN_POINT('Ctrl Pts',(-57.7310874497581,-101.071424703906,
179.985485069079));
#26811=CARTESIAN_POINT('Ctrl Pts',(-56.0736306997542,-101.153839438193,
179.985484999752));
#26812=CARTESIAN_POINT('Ctrl Pts',(-54.8987210498124,-101.184811427766,
178.813912075476));
#26813=CARTESIAN_POINT('Ctrl Pts',(-53.7238113998707,-101.21578341734,177.6423391512));
#26814=CARTESIAN_POINT('Ctrl Pts',(-53.7138734058908,-101.122561645335,
175.985484901707));
#26815=CARTESIAN_POINT('Ctrl Pts',(-53.7039354119109,-101.029339873331,
174.328630652215));
#26816=CARTESIAN_POINT('Ctrl Pts',(-54.8589690335105,-100.811924344053,
173.157057825983));
#26817=CARTESIAN_POINT('Ctrl Pts',(-56.0140026551102,-100.594508814776,
171.985484999752));
#26818=CARTESIAN_POINT('Ctrl Pts',(-57.65158327928,-100.325650551179,171.985485069079));
#26819=CARTESIAN_POINT('Ctrl Pts',(-59.2891639034499,-100.056792287582,
171.985485138407));
#26820=CARTESIAN_POINT('Ctrl Pts',(-60.4441974275576,-99.8393767686974,
173.157058062683));
#26821=CARTESIAN_POINT('Ctrl Pts',(-61.5992309516654,-99.6219612498133,
174.328630986959));
#26822=CARTESIAN_POINT('Ctrl Pts',(-61.5892928198112,-99.528739492507,175.985485236451));
#26823=CARTESIAN_POINT('Ctrl Pts',(-61.579354687957,-99.4355177352008,177.642339485944));
#26824=CARTESIAN_POINT('Ctrl Pts',(-60.4044449405234,-99.4664897351676,
178.813912312176));
#26825=CARTESIAN_POINT('Ctrl Pts',(-59.2295351930898,-99.4974617351344,
179.985485138407));
#26826=CARTESIAN_POINT('Ctrl Pts',(-57.5720784430859,-99.5798764694207,
179.985485069079));
#26827=CARTESIAN_POINT('Ctrl Pts',(-55.914621693082,-99.662291203707,179.985484999752));
#26828=CARTESIAN_POINT('Ctrl Pts',(-54.7397120431402,-99.6932631932805,
178.813912075476));
#26829=CARTESIAN_POINT('Ctrl Pts',(-53.5648023931984,-99.724235182854,177.6423391512));
#26830=CARTESIAN_POINT('Ctrl Pts',(-53.5548643992186,-99.6310134108495,
175.985484901707));
#26831=CARTESIAN_POINT('Ctrl Pts',(-53.5449264052387,-99.5377916388449,
174.328630652215));
#26832=CARTESIAN_POINT('Ctrl Pts',(-54.6999600268383,-99.3203761095675,
173.157057825983));
#26833=CARTESIAN_POINT('Ctrl Pts',(-55.8549936484379,-99.10296058029,171.985484999752));
#26834=CARTESIAN_POINT('Ctrl Pts',(-57.4925742726078,-98.834102316693,171.985485069079));
#26835=CARTESIAN_POINT('Ctrl Pts',(-59.1301548967777,-98.5652440530961,
171.985485138407));
#26836=CARTESIAN_POINT('Ctrl Pts',(-60.2851884208854,-98.3478285342118,
173.157058062683));
#26837=CARTESIAN_POINT('Ctrl Pts',(-61.4402219449932,-98.1304130153276,
174.328630986959));
#26838=CARTESIAN_POINT('Ctrl Pts',(-61.430283813139,-98.0371912580215,175.985485236451));
#26839=CARTESIAN_POINT('Ctrl Pts',(-61.4203456812848,-97.9439695007152,
177.642339485944));
#26840=CARTESIAN_POINT('Ctrl Pts',(-60.2454359338512,-97.974941500682,178.813912312176));
#26841=CARTESIAN_POINT('Ctrl Pts',(-59.0705261864175,-98.0059135006488,
179.985485138407));
#26842=CARTESIAN_POINT('Ctrl Pts',(-57.4130694364136,-98.0883282349351,
179.985485069079));
#26843=CARTESIAN_POINT('Ctrl Pts',(-55.7556126864097,-98.1707429692214,
179.985484999752));
#26844=CARTESIAN_POINT('Ctrl Pts',(-54.580703036468,-98.2017149587949,178.813912075476));
#26845=CARTESIAN_POINT('Ctrl Pts',(-56.181115489574,-113.283598570176,178.821287383467));
#26846=CARTESIAN_POINT('Ctrl Pts',(-55.0031681001975,-113.314894403068,
177.646659506339));
#26847=CARTESIAN_POINT('Ctrl Pts',(-54.9932301063974,-113.221672631044,
175.985484901271));
#26848=CARTESIAN_POINT('Ctrl Pts',(-54.9832921125973,-113.12845085902,174.324310296203));
#26849=CARTESIAN_POINT('Ctrl Pts',(-56.1413634738858,-112.910711486397,
173.149682517375));
#26850=CARTESIAN_POINT('Ctrl Pts',(-57.2994348351743,-112.692972113774,
171.975054738546));
#26851=CARTESIAN_POINT('Ctrl Pts',(-58.9413114718314,-112.423655866545,
171.975054808055));
#26852=CARTESIAN_POINT('Ctrl Pts',(-60.5831881084886,-112.154339619316,
171.975054877564));
#26853=CARTESIAN_POINT('Ctrl Pts',(-61.741259372031,-111.936600257113,173.149682754692));
#26854=CARTESIAN_POINT('Ctrl Pts',(-62.8993306355734,-111.71886089491,174.32431063182));
#26855=CARTESIAN_POINT('Ctrl Pts',(-62.8893925035395,-111.625639137623,
175.985485236888));
#26856=CARTESIAN_POINT('Ctrl Pts',(-62.8794543715055,-111.532417380336,
177.646659841956));
#26857=CARTESIAN_POINT('Ctrl Pts',(-61.701506884383,-111.563713223648,178.821287620784));
#26858=CARTESIAN_POINT('Ctrl Pts',(-60.5235593972605,-111.595009066961,
179.995915399612));
#26859=CARTESIAN_POINT('Ctrl Pts',(-58.8618066347693,-111.677881784879,
179.995915330104));
#26860=CARTESIAN_POINT('Ctrl Pts',(-57.2000538722782,-111.760754502798,
179.995915260595));
#26861=CARTESIAN_POINT('Ctrl Pts',(-56.0221064829017,-111.79205033569,178.821287383467));
#26862=CARTESIAN_POINT('Ctrl Pts',(-54.8441590935253,-111.823346168582,
177.646659506339));
#26863=CARTESIAN_POINT('Ctrl Pts',(-54.8342210997252,-111.730124396559,
175.985484901271));
#26864=CARTESIAN_POINT('Ctrl Pts',(-54.8242831059251,-111.636902624535,
174.324310296203));
#26865=CARTESIAN_POINT('Ctrl Pts',(-55.9823544672136,-111.419163251912,
173.149682517375));
#26866=CARTESIAN_POINT('Ctrl Pts',(-57.1404258285021,-111.201423879289,
171.975054738546));
#26867=CARTESIAN_POINT('Ctrl Pts',(-58.7823024651592,-110.932107632059,
171.975054808055));
#26868=CARTESIAN_POINT('Ctrl Pts',(-60.4241791018163,-110.66279138483,171.975054877564));
#26869=CARTESIAN_POINT('Ctrl Pts',(-61.5822503653587,-110.445052022627,
173.149682754692));
#26870=CARTESIAN_POINT('Ctrl Pts',(-62.7403216289012,-110.227312660424,
174.32431063182));
#26871=CARTESIAN_POINT('Ctrl Pts',(-62.7303834968672,-110.134090903137,
175.985485236888));
#26872=CARTESIAN_POINT('Ctrl Pts',(-62.7204453648333,-110.04086914585,177.646659841956));
#26873=CARTESIAN_POINT('Ctrl Pts',(-61.5424978777108,-110.072164989163,
178.821287620784));
#26874=CARTESIAN_POINT('Ctrl Pts',(-60.3645503905882,-110.103460832475,
179.995915399612));
#26875=CARTESIAN_POINT('Ctrl Pts',(-58.7027976280971,-110.186333550394,
179.995915330104));
#26876=CARTESIAN_POINT('Ctrl Pts',(-57.041044865606,-110.269206268313,179.995915260595));
#26877=CARTESIAN_POINT('Ctrl Pts',(-55.8630974762295,-110.300502101205,
178.821287383467));
#26878=CARTESIAN_POINT('Ctrl Pts',(-54.6851500868531,-110.331797934097,
177.646659506339));
#26879=CARTESIAN_POINT('Ctrl Pts',(-54.675212093053,-110.238576162073,175.985484901271));
#26880=CARTESIAN_POINT('Ctrl Pts',(-54.6652740992529,-110.145354390049,
174.324310296203));
#26881=CARTESIAN_POINT('Ctrl Pts',(-55.8233454605414,-109.927615017426,
173.149682517375));
#26882=CARTESIAN_POINT('Ctrl Pts',(-56.9814168218299,-109.709875644803,
171.975054738546));
#26883=CARTESIAN_POINT('Ctrl Pts',(-58.623293458487,-109.440559397574,171.975054808055));
#26884=CARTESIAN_POINT('Ctrl Pts',(-60.2651700951441,-109.171243150344,
171.975054877564));
#26885=CARTESIAN_POINT('Ctrl Pts',(-61.4232413586865,-108.953503788142,
173.149682754692));
#26886=CARTESIAN_POINT('Ctrl Pts',(-62.581312622229,-108.735764425939,174.32431063182));
#26887=CARTESIAN_POINT('Ctrl Pts',(-62.571374490195,-108.642542668652,175.985485236888));
#26888=CARTESIAN_POINT('Ctrl Pts',(-62.5614363581611,-108.549320911365,
177.646659841956));
#26889=CARTESIAN_POINT('Ctrl Pts',(-61.3834888710385,-108.580616754677,
178.821287620784));
#26890=CARTESIAN_POINT('Ctrl Pts',(-60.205541383916,-108.61191259799,179.995915399612));
#26891=CARTESIAN_POINT('Ctrl Pts',(-58.5437886214249,-108.694785315908,
179.995915330104));
#26892=CARTESIAN_POINT('Ctrl Pts',(-56.8820358589338,-108.777658033827,
179.995915260595));
#26893=CARTESIAN_POINT('Ctrl Pts',(-55.7040884695573,-108.808953866719,
178.821287383467));
#26894=CARTESIAN_POINT('Ctrl Pts',(-54.5261410801808,-108.840249699611,
177.646659506339));
#26895=CARTESIAN_POINT('Ctrl Pts',(-54.5162030863807,-108.747027927587,
175.985484901271));
#26896=CARTESIAN_POINT('Ctrl Pts',(-54.5062650925806,-108.653806155564,
174.324310296203));
#26897=CARTESIAN_POINT('Ctrl Pts',(-55.6643364538691,-108.436066782941,
173.149682517375));
#26898=CARTESIAN_POINT('Ctrl Pts',(-56.8224078151577,-108.218327410317,
171.975054738546));
#26899=CARTESIAN_POINT('Ctrl Pts',(-58.4642844518147,-107.949011163088,
171.975054808055));
#26900=CARTESIAN_POINT('Ctrl Pts',(-60.1061610884719,-107.679694915859,
171.975054877564));
#26901=CARTESIAN_POINT('Ctrl Pts',(-61.2642323520143,-107.461955553656,
173.149682754692));
#26902=CARTESIAN_POINT('Ctrl Pts',(-62.4223036155567,-107.244216191453,
174.32431063182));
#26903=CARTESIAN_POINT('Ctrl Pts',(-62.4123654835228,-107.150994434166,
175.985485236888));
#26904=CARTESIAN_POINT('Ctrl Pts',(-62.4024273514889,-107.057772676879,
177.646659841956));
#26905=CARTESIAN_POINT('Ctrl Pts',(-61.2244798643663,-107.089068520192,
178.821287620784));
#26906=CARTESIAN_POINT('Ctrl Pts',(-60.0465323772438,-107.120364363504,
179.995915399612));
#26907=CARTESIAN_POINT('Ctrl Pts',(-58.3847796147526,-107.203237081423,
179.995915330104));
#26908=CARTESIAN_POINT('Ctrl Pts',(-56.7230268522615,-107.286109799341,
179.995915260595));
#26909=CARTESIAN_POINT('Ctrl Pts',(-55.5450794628851,-107.317405632233,
178.821287383467));
#26910=CARTESIAN_POINT('Ctrl Pts',(-54.3671320735086,-107.348701465125,
177.646659506339));
#26911=CARTESIAN_POINT('Ctrl Pts',(-54.3571940797085,-107.255479693102,
175.985484901271));
#26912=CARTESIAN_POINT('Ctrl Pts',(-54.3472560859084,-107.162257921078,
174.324310296203));
#26913=CARTESIAN_POINT('Ctrl Pts',(-55.5053274471969,-106.944518548455,
173.149682517375));
#26914=CARTESIAN_POINT('Ctrl Pts',(-56.6633988084854,-106.726779175832,
171.975054738546));
#26915=CARTESIAN_POINT('Ctrl Pts',(-58.3052754451425,-106.457462928602,
171.975054808055));
#26916=CARTESIAN_POINT('Ctrl Pts',(-59.9471520817997,-106.188146681373,
171.975054877564));
#26917=CARTESIAN_POINT('Ctrl Pts',(-61.1052233453421,-105.97040731917,173.149682754692));
#26918=CARTESIAN_POINT('Ctrl Pts',(-62.2632946088845,-105.752667956968,
174.32431063182));
#26919=CARTESIAN_POINT('Ctrl Pts',(-62.2533564768505,-105.659446199681,
175.985485236888));
#26920=CARTESIAN_POINT('Ctrl Pts',(-62.2434183448166,-105.566224442394,
177.646659841956));
#26921=CARTESIAN_POINT('Ctrl Pts',(-61.0654708576941,-105.597520285706,
178.821287620784));
#26922=CARTESIAN_POINT('Ctrl Pts',(-59.8875233705716,-105.628816129018,
179.995915399612));
#26923=CARTESIAN_POINT('Ctrl Pts',(-58.2257706080804,-105.711688846937,
179.995915330104));
#26924=CARTESIAN_POINT('Ctrl Pts',(-56.5640178455893,-105.794561564856,
179.995915260595));
#26925=CARTESIAN_POINT('Ctrl Pts',(-55.3860704562128,-105.825857397748,
178.821287383467));
#26926=CARTESIAN_POINT('Ctrl Pts',(-54.2081230668364,-105.85715323064,177.646659506339));
#26927=CARTESIAN_POINT('Ctrl Pts',(-54.1981850730363,-105.763931458616,
175.985484901271));
#26928=CARTESIAN_POINT('Ctrl Pts',(-54.1882470792362,-105.670709686593,
174.324310296203));
#26929=CARTESIAN_POINT('Ctrl Pts',(-55.3463184405247,-105.452970313969,
173.149682517375));
#26930=CARTESIAN_POINT('Ctrl Pts',(-56.5043898018132,-105.235230941346,
171.975054738546));
#26931=CARTESIAN_POINT('Ctrl Pts',(-58.1462664384703,-104.965914694117,
171.975054808055));
#26932=CARTESIAN_POINT('Ctrl Pts',(-59.7881430751274,-104.696598446888,
171.975054877564));
#26933=CARTESIAN_POINT('Ctrl Pts',(-60.9462143386698,-104.478859084685,
173.149682754692));
#26934=CARTESIAN_POINT('Ctrl Pts',(-62.1042856022123,-104.261119722482,
174.32431063182));
#26935=CARTESIAN_POINT('Ctrl Pts',(-62.0943474701783,-104.167897965195,
175.985485236888));
#26936=CARTESIAN_POINT('Ctrl Pts',(-62.0844093381444,-104.074676207908,
177.646659841956));
#26937=CARTESIAN_POINT('Ctrl Pts',(-60.9064618510219,-104.10597205122,178.821287620784));
#26938=CARTESIAN_POINT('Ctrl Pts',(-59.7285143638993,-104.137267894533,
179.995915399612));
#26939=CARTESIAN_POINT('Ctrl Pts',(-58.0667616014082,-104.220140612451,
179.995915330104));
#26940=CARTESIAN_POINT('Ctrl Pts',(-56.4050088389171,-104.30301333037,179.995915260595));
#26941=CARTESIAN_POINT('Ctrl Pts',(-55.2270614495406,-104.334309163262,
178.821287383467));
#26942=CARTESIAN_POINT('Ctrl Pts',(-54.0491140601642,-104.365604996154,
177.646659506339));
#26943=CARTESIAN_POINT('Ctrl Pts',(-54.039176066364,-104.272383224131,175.985484901271));
#26944=CARTESIAN_POINT('Ctrl Pts',(-54.029238072564,-104.179161452107,174.324310296203));
#26945=CARTESIAN_POINT('Ctrl Pts',(-55.1873094338524,-103.961422079484,
173.149682517375));
#26946=CARTESIAN_POINT('Ctrl Pts',(-56.345380795141,-103.743682706861,171.975054738546));
#26947=CARTESIAN_POINT('Ctrl Pts',(-57.9872574317981,-103.474366459631,
171.975054808055));
#26948=CARTESIAN_POINT('Ctrl Pts',(-59.6291340684552,-103.205050212402,
171.975054877564));
#26949=CARTESIAN_POINT('Ctrl Pts',(-60.7872053319976,-102.987310850199,
173.149682754692));
#26950=CARTESIAN_POINT('Ctrl Pts',(-61.94527659554,-102.769571487996,174.32431063182));
#26951=CARTESIAN_POINT('Ctrl Pts',(-61.9353384635061,-102.676349730709,
175.985485236888));
#26952=CARTESIAN_POINT('Ctrl Pts',(-61.9254003314722,-102.583127973422,
177.646659841956));
#26953=CARTESIAN_POINT('Ctrl Pts',(-60.7474528443496,-102.614423816735,
178.821287620784));
#26954=CARTESIAN_POINT('Ctrl Pts',(-59.5695053572271,-102.645719660047,
179.995915399612));
#26955=CARTESIAN_POINT('Ctrl Pts',(-57.907752594736,-102.728592377966,179.995915330104));
#26956=CARTESIAN_POINT('Ctrl Pts',(-56.2459998322448,-102.811465095885,
179.995915260595));
#26957=CARTESIAN_POINT('Ctrl Pts',(-55.0680524428684,-102.842760928777,
178.821287383467));
#26958=CARTESIAN_POINT('Ctrl Pts',(-53.8901050534919,-102.874056761669,
177.646659506339));
#26959=CARTESIAN_POINT('Ctrl Pts',(-53.8801670596918,-102.780834989645,
175.985484901271));
#26960=CARTESIAN_POINT('Ctrl Pts',(-53.8702290658917,-102.687613217621,
174.324310296203));
#26961=CARTESIAN_POINT('Ctrl Pts',(-55.0283004271802,-102.469873844998,
173.149682517375));
#26962=CARTESIAN_POINT('Ctrl Pts',(-56.1863717884687,-102.252134472375,
171.975054738546));
#26963=CARTESIAN_POINT('Ctrl Pts',(-57.8282484251258,-101.982818225146,
171.975054808055));
#26964=CARTESIAN_POINT('Ctrl Pts',(-59.470125061783,-101.713501977916,171.975054877564));
#26965=CARTESIAN_POINT('Ctrl Pts',(-60.6281963253254,-101.495762615714,
173.149682754692));
#26966=CARTESIAN_POINT('Ctrl Pts',(-61.7862675888678,-101.278023253511,
174.32431063182));
#26967=CARTESIAN_POINT('Ctrl Pts',(-61.7763294568339,-101.184801496224,
175.985485236888));
#26968=CARTESIAN_POINT('Ctrl Pts',(-61.7663913247999,-101.091579738937,
177.646659841956));
#26969=CARTESIAN_POINT('Ctrl Pts',(-60.5884438376774,-101.122875582249,
178.821287620784));
#26970=CARTESIAN_POINT('Ctrl Pts',(-59.4104963505549,-101.154171425562,
179.995915399612));
#26971=CARTESIAN_POINT('Ctrl Pts',(-57.7487435880637,-101.23704414348,179.995915330104));
#26972=CARTESIAN_POINT('Ctrl Pts',(-56.0869908255726,-101.319916861399,
179.995915260595));
#26973=CARTESIAN_POINT('Ctrl Pts',(-54.9090434361961,-101.351212694291,
178.821287383467));
#26974=CARTESIAN_POINT('Ctrl Pts',(-53.7310960468197,-101.382508527183,
177.646659506339));
#26975=CARTESIAN_POINT('Ctrl Pts',(-53.7211580530196,-101.289286755159,
175.985484901271));
#26976=CARTESIAN_POINT('Ctrl Pts',(-53.7112200592195,-101.196064983136,
174.324310296203));
#26977=CARTESIAN_POINT('Ctrl Pts',(-54.869291420508,-100.978325610513,173.149682517375));
#26978=CARTESIAN_POINT('Ctrl Pts',(-56.0273627817965,-100.760586237889,
171.975054738546));
#26979=CARTESIAN_POINT('Ctrl Pts',(-57.6692394184536,-100.49126999066,171.975054808055));
#26980=CARTESIAN_POINT('Ctrl Pts',(-59.3111160551107,-100.221953743431,
171.975054877564));
#26981=CARTESIAN_POINT('Ctrl Pts',(-60.4691873186531,-100.004214381228,
173.149682754692));
#26982=CARTESIAN_POINT('Ctrl Pts',(-61.6272585821956,-99.7864750190253,
174.32431063182));
#26983=CARTESIAN_POINT('Ctrl Pts',(-61.6173204501616,-99.6932532617382,
175.985485236888));
#26984=CARTESIAN_POINT('Ctrl Pts',(-61.6073823181277,-99.6000315044512,
177.646659841956));
#26985=CARTESIAN_POINT('Ctrl Pts',(-60.4294348310052,-99.6313273477637,
178.821287620784));
#26986=CARTESIAN_POINT('Ctrl Pts',(-59.2514873438827,-99.6626231910761,
179.995915399612));
#26987=CARTESIAN_POINT('Ctrl Pts',(-57.5897345813915,-99.7454959089947,
179.995915330104));
#26988=CARTESIAN_POINT('Ctrl Pts',(-55.9279818189004,-99.8283686269133,
179.995915260595));
#26989=CARTESIAN_POINT('Ctrl Pts',(-54.7500344295239,-99.8596644598054,
178.821287383467));
#26990=CARTESIAN_POINT('Ctrl Pts',(-53.5720870401475,-99.8909602926975,
177.646659506339));
#26991=CARTESIAN_POINT('Ctrl Pts',(-53.5621490463474,-99.7977385206737,
175.985484901271));
#26992=CARTESIAN_POINT('Ctrl Pts',(-53.5522110525473,-99.7045167486501,
174.324310296203));
#26993=CARTESIAN_POINT('Ctrl Pts',(-54.7102824138358,-99.4867773760269,
173.149682517375));
#26994=CARTESIAN_POINT('Ctrl Pts',(-55.8683537751243,-99.2690380034038,
171.975054738546));
#26995=CARTESIAN_POINT('Ctrl Pts',(-57.5102304117814,-98.9997217561745,
171.975054808055));
#26996=CARTESIAN_POINT('Ctrl Pts',(-59.1521070484385,-98.7304055089452,
171.975054877564));
#26997=CARTESIAN_POINT('Ctrl Pts',(-60.3101783119809,-98.5126661467424,
173.149682754692));
#26998=CARTESIAN_POINT('Ctrl Pts',(-61.4682495755234,-98.2949267845397,
174.32431063182));
#26999=CARTESIAN_POINT('Ctrl Pts',(-61.4583114434894,-98.2017050272526,
175.985485236888));
#27000=CARTESIAN_POINT('Ctrl Pts',(-61.4483733114555,-98.1084832699656,
177.646659841956));
#27001=CARTESIAN_POINT('Ctrl Pts',(-60.2704258243329,-98.139779113278,178.821287620784));
#27002=CARTESIAN_POINT('Ctrl Pts',(-59.0924783372104,-98.1710749565905,
179.995915399612));
#27003=CARTESIAN_POINT('Ctrl Pts',(-57.4307255747193,-98.2539476745091,
179.995915330104));
#27004=CARTESIAN_POINT('Ctrl Pts',(-55.7689728122282,-98.3368203924277,
179.995915260595));
#27005=CARTESIAN_POINT('Ctrl Pts',(-54.5910254228517,-98.3681162253198,
178.821287383467));
#27006=CARTESIAN_POINT('Ctrl Pts',(-56.1988062143188,-113.449542435949,
178.821287383467));
#27007=CARTESIAN_POINT('Ctrl Pts',(-55.0208588249424,-113.480838268841,
177.646659506339));
#27008=CARTESIAN_POINT('Ctrl Pts',(-55.0109208311422,-113.387616496817,
175.985484901271));
#27009=CARTESIAN_POINT('Ctrl Pts',(-55.0009828373422,-113.294394724794,
174.324310296203));
#27010=CARTESIAN_POINT('Ctrl Pts',(-56.1590541986307,-113.07665535217,173.149682517375));
#27011=CARTESIAN_POINT('Ctrl Pts',(-57.3171255599192,-112.858915979547,
171.975054738546));
#27012=CARTESIAN_POINT('Ctrl Pts',(-58.9590021965763,-112.589599732318,
171.975054808055));
#27013=CARTESIAN_POINT('Ctrl Pts',(-60.6008788332334,-112.320283485089,
171.975054877564));
#27014=CARTESIAN_POINT('Ctrl Pts',(-61.7589500967758,-112.102544122886,
173.149682754692));
#27015=CARTESIAN_POINT('Ctrl Pts',(-62.9170213603182,-111.884804760683,
174.32431063182));
#27016=CARTESIAN_POINT('Ctrl Pts',(-62.9070832282843,-111.791583003396,
175.985485236888));
#27017=CARTESIAN_POINT('Ctrl Pts',(-62.8971450962504,-111.698361246109,
177.646659841956));
#27018=CARTESIAN_POINT('Ctrl Pts',(-61.7191976091278,-111.729657089422,
178.821287620784));
#27019=CARTESIAN_POINT('Ctrl Pts',(-60.5412501220053,-111.760952932734,
179.995915399612));
#27020=CARTESIAN_POINT('Ctrl Pts',(-58.8794973595142,-111.843825650653,
179.995915330104));
#27021=CARTESIAN_POINT('Ctrl Pts',(-57.217744597023,-111.926698368571,179.995915260595));
#27022=CARTESIAN_POINT('Ctrl Pts',(-56.0397972076466,-111.957994201463,
178.821287383467));
#27023=CARTESIAN_POINT('Ctrl Pts',(-54.8618498182701,-111.989290034355,
177.646659506339));
#27024=CARTESIAN_POINT('Ctrl Pts',(-54.85191182447,-111.896068262332,175.985484901271));
#27025=CARTESIAN_POINT('Ctrl Pts',(-54.8419738306699,-111.802846490308,
174.324310296203));
#27026=CARTESIAN_POINT('Ctrl Pts',(-56.0000451919584,-111.585107117685,
173.149682517375));
#27027=CARTESIAN_POINT('Ctrl Pts',(-57.158116553247,-111.367367745062,171.975054738546));
#27028=CARTESIAN_POINT('Ctrl Pts',(-58.799993189904,-111.098051497832,171.975054808055));
#27029=CARTESIAN_POINT('Ctrl Pts',(-60.4418698265612,-110.828735250603,
171.975054877564));
#27030=CARTESIAN_POINT('Ctrl Pts',(-61.5999410901036,-110.6109958884,173.149682754692));
#27031=CARTESIAN_POINT('Ctrl Pts',(-62.758012353646,-110.393256526198,174.32431063182));
#27032=CARTESIAN_POINT('Ctrl Pts',(-62.7480742216121,-110.30003476891,175.985485236888));
#27033=CARTESIAN_POINT('Ctrl Pts',(-62.7381360895782,-110.206813011623,
177.646659841956));
#27034=CARTESIAN_POINT('Ctrl Pts',(-61.5601886024556,-110.238108854936,
178.821287620784));
#27035=CARTESIAN_POINT('Ctrl Pts',(-60.3822411153331,-110.269404698248,
179.995915399612));
#27036=CARTESIAN_POINT('Ctrl Pts',(-58.7204883528419,-110.352277416167,
179.995915330104));
#27037=CARTESIAN_POINT('Ctrl Pts',(-57.0587355903508,-110.435150134086,
179.995915260595));
#27038=CARTESIAN_POINT('Ctrl Pts',(-55.8807882009743,-110.466445966978,
178.821287383467));
#27039=CARTESIAN_POINT('Ctrl Pts',(-54.7028408115979,-110.49774179987,177.646659506339));
#27040=CARTESIAN_POINT('Ctrl Pts',(-54.6929028177978,-110.404520027846,
175.985484901271));
#27041=CARTESIAN_POINT('Ctrl Pts',(-54.6829648239977,-110.311298255822,
174.324310296203));
#27042=CARTESIAN_POINT('Ctrl Pts',(-55.8410361852862,-110.093558883199,
173.149682517375));
#27043=CARTESIAN_POINT('Ctrl Pts',(-56.9991075465747,-109.875819510576,
171.975054738546));
#27044=CARTESIAN_POINT('Ctrl Pts',(-58.6409841832318,-109.606503263347,
171.975054808055));
#27045=CARTESIAN_POINT('Ctrl Pts',(-60.2828608198889,-109.337187016117,
171.975054877564));
#27046=CARTESIAN_POINT('Ctrl Pts',(-61.4409320834313,-109.119447653915,
173.149682754692));
#27047=CARTESIAN_POINT('Ctrl Pts',(-62.5990033469738,-108.901708291712,
174.32431063182));
#27048=CARTESIAN_POINT('Ctrl Pts',(-62.5890652149398,-108.808486534425,
175.985485236888));
#27049=CARTESIAN_POINT('Ctrl Pts',(-62.5791270829059,-108.715264777138,
177.646659841956));
#27050=CARTESIAN_POINT('Ctrl Pts',(-61.4011795957834,-108.74656062045,178.821287620784));
#27051=CARTESIAN_POINT('Ctrl Pts',(-60.2232321086609,-108.777856463763,
179.995915399612));
#27052=CARTESIAN_POINT('Ctrl Pts',(-58.5614793461697,-108.860729181681,
179.995915330104));
#27053=CARTESIAN_POINT('Ctrl Pts',(-56.8997265836786,-108.9436018996,179.995915260595));
#27054=CARTESIAN_POINT('Ctrl Pts',(-55.7217791943021,-108.974897732492,
178.821287383467));
#27055=CARTESIAN_POINT('Ctrl Pts',(-54.5438318049257,-109.006193565384,
177.646659506339));
#27056=CARTESIAN_POINT('Ctrl Pts',(-54.5338938111256,-108.91297179336,175.985484901271));
#27057=CARTESIAN_POINT('Ctrl Pts',(-54.5239558173255,-108.819750021337,
174.324310296203));
#27058=CARTESIAN_POINT('Ctrl Pts',(-55.682027178614,-108.602010648714,173.149682517375));
#27059=CARTESIAN_POINT('Ctrl Pts',(-56.8400985399025,-108.384271276091,
171.975054738546));
#27060=CARTESIAN_POINT('Ctrl Pts',(-58.4819751765596,-108.114955028861,
171.975054808055));
#27061=CARTESIAN_POINT('Ctrl Pts',(-60.1238518132167,-107.845638781632,
171.975054877564));
#27062=CARTESIAN_POINT('Ctrl Pts',(-61.2819230767591,-107.627899419429,
173.149682754692));
#27063=CARTESIAN_POINT('Ctrl Pts',(-62.4399943403016,-107.410160057226,
174.32431063182));
#27064=CARTESIAN_POINT('Ctrl Pts',(-62.4300562082676,-107.316938299939,
175.985485236888));
#27065=CARTESIAN_POINT('Ctrl Pts',(-62.4201180762337,-107.223716542652,
177.646659841956));
#27066=CARTESIAN_POINT('Ctrl Pts',(-61.2421705891111,-107.255012385965,
178.821287620784));
#27067=CARTESIAN_POINT('Ctrl Pts',(-60.0642231019886,-107.286308229277,
179.995915399612));
#27068=CARTESIAN_POINT('Ctrl Pts',(-58.4024703394975,-107.369180947196,
179.995915330104));
#27069=CARTESIAN_POINT('Ctrl Pts',(-56.7407175770064,-107.452053665114,
179.995915260595));
#27070=CARTESIAN_POINT('Ctrl Pts',(-55.5627701876299,-107.483349498006,
178.821287383467));
#27071=CARTESIAN_POINT('Ctrl Pts',(-54.3848227982534,-107.514645330899,
177.646659506339));
#27072=CARTESIAN_POINT('Ctrl Pts',(-54.3748848044533,-107.421423558875,
175.985484901271));
#27073=CARTESIAN_POINT('Ctrl Pts',(-54.3649468106533,-107.328201786851,
174.324310296203));
#27074=CARTESIAN_POINT('Ctrl Pts',(-55.5230181719417,-107.110462414228,
173.149682517375));
#27075=CARTESIAN_POINT('Ctrl Pts',(-56.6810895332303,-106.892723041605,
171.975054738546));
#27076=CARTESIAN_POINT('Ctrl Pts',(-58.3229661698874,-106.623406794376,
171.975054808055));
#27077=CARTESIAN_POINT('Ctrl Pts',(-59.9648428065445,-106.354090547146,
171.975054877564));
#27078=CARTESIAN_POINT('Ctrl Pts',(-61.1229140700869,-106.136351184943,
173.149682754692));
#27079=CARTESIAN_POINT('Ctrl Pts',(-62.2809853336293,-105.918611822741,
174.32431063182));
#27080=CARTESIAN_POINT('Ctrl Pts',(-62.2710472015954,-105.825390065454,
175.985485236888));
#27081=CARTESIAN_POINT('Ctrl Pts',(-62.2611090695615,-105.732168308167,
177.646659841956));
#27082=CARTESIAN_POINT('Ctrl Pts',(-61.0831615824389,-105.763464151479,
178.821287620784));
#27083=CARTESIAN_POINT('Ctrl Pts',(-59.9052140953164,-105.794759994792,
179.995915399612));
#27084=CARTESIAN_POINT('Ctrl Pts',(-58.2434613328252,-105.87763271271,179.995915330104));
#27085=CARTESIAN_POINT('Ctrl Pts',(-56.5817085703341,-105.960505430629,
179.995915260595));
#27086=CARTESIAN_POINT('Ctrl Pts',(-55.4037611809577,-105.991801263521,
178.821287383467));
#27087=CARTESIAN_POINT('Ctrl Pts',(-54.2258137915812,-106.023097096413,
177.646659506339));
#27088=CARTESIAN_POINT('Ctrl Pts',(-54.2158757977811,-105.929875324389,
175.985484901271));
#27089=CARTESIAN_POINT('Ctrl Pts',(-54.205937803981,-105.836653552366,174.324310296203));
#27090=CARTESIAN_POINT('Ctrl Pts',(-55.3640091652695,-105.618914179742,
173.149682517375));
#27091=CARTESIAN_POINT('Ctrl Pts',(-56.522080526558,-105.401174807119,171.975054738546));
#27092=CARTESIAN_POINT('Ctrl Pts',(-58.1639571632151,-105.13185855989,171.975054808055));
#27093=CARTESIAN_POINT('Ctrl Pts',(-59.8058337998722,-104.862542312661,
171.975054877564));
#27094=CARTESIAN_POINT('Ctrl Pts',(-60.9639050634147,-104.644802950458,
173.149682754692));
#27095=CARTESIAN_POINT('Ctrl Pts',(-62.1219763269571,-104.427063588255,
174.32431063182));
#27096=CARTESIAN_POINT('Ctrl Pts',(-62.1120381949232,-104.333841830968,
175.985485236888));
#27097=CARTESIAN_POINT('Ctrl Pts',(-62.1021000628892,-104.240620073681,
177.646659841956));
#27098=CARTESIAN_POINT('Ctrl Pts',(-60.9241525757667,-104.271915916993,
178.821287620784));
#27099=CARTESIAN_POINT('Ctrl Pts',(-59.7462050886442,-104.303211760306,
179.995915399612));
#27100=CARTESIAN_POINT('Ctrl Pts',(-58.084452326153,-104.386084478225,179.995915330104));
#27101=CARTESIAN_POINT('Ctrl Pts',(-56.4226995636619,-104.468957196143,
179.995915260595));
#27102=CARTESIAN_POINT('Ctrl Pts',(-55.2447521742854,-104.500253029035,
178.821287383467));
#27103=CARTESIAN_POINT('Ctrl Pts',(-54.066804784909,-104.531548861927,177.646659506339));
#27104=CARTESIAN_POINT('Ctrl Pts',(-54.0568667911089,-104.438327089904,
175.985484901271));
#27105=CARTESIAN_POINT('Ctrl Pts',(-54.0469287973088,-104.34510531788,174.324310296203));
#27106=CARTESIAN_POINT('Ctrl Pts',(-55.2050001585973,-104.127365945257,
173.149682517375));
#27107=CARTESIAN_POINT('Ctrl Pts',(-56.3630715198858,-103.909626572634,
171.975054738546));
#27108=CARTESIAN_POINT('Ctrl Pts',(-58.0049481565429,-103.640310325404,
171.975054808055));
#27109=CARTESIAN_POINT('Ctrl Pts',(-59.6468247932,-103.370994078175,171.975054877564));
#27110=CARTESIAN_POINT('Ctrl Pts',(-60.8048960567424,-103.153254715972,
173.149682754692));
#27111=CARTESIAN_POINT('Ctrl Pts',(-61.9629673202849,-102.93551535377,174.32431063182));
#27112=CARTESIAN_POINT('Ctrl Pts',(-61.9530291882509,-102.842293596483,
175.985485236888));
#27113=CARTESIAN_POINT('Ctrl Pts',(-61.943091056217,-102.749071839196,177.646659841956));
#27114=CARTESIAN_POINT('Ctrl Pts',(-60.7651435690945,-102.780367682508,
178.821287620784));
#27115=CARTESIAN_POINT('Ctrl Pts',(-59.587196081972,-102.81166352582,179.995915399612));
#27116=CARTESIAN_POINT('Ctrl Pts',(-57.9254433194808,-102.894536243739,
179.995915330104));
#27117=CARTESIAN_POINT('Ctrl Pts',(-56.2636905569897,-102.977408961658,
179.995915260595));
#27118=CARTESIAN_POINT('Ctrl Pts',(-55.0857431676132,-103.00870479455,178.821287383467));
#27119=CARTESIAN_POINT('Ctrl Pts',(-53.9077957782368,-103.040000627442,
177.646659506339));
#27120=CARTESIAN_POINT('Ctrl Pts',(-53.8978577844367,-102.946778855418,
175.985484901271));
#27121=CARTESIAN_POINT('Ctrl Pts',(-53.8879197906366,-102.853557083394,
174.324310296203));
#27122=CARTESIAN_POINT('Ctrl Pts',(-55.0459911519251,-102.635817710771,
173.149682517375));
#27123=CARTESIAN_POINT('Ctrl Pts',(-56.2040625132136,-102.418078338148,
171.975054738546));
#27124=CARTESIAN_POINT('Ctrl Pts',(-57.8459391498707,-102.148762090919,
171.975054808055));
#27125=CARTESIAN_POINT('Ctrl Pts',(-59.4878157865278,-101.879445843689,
171.975054877564));
#27126=CARTESIAN_POINT('Ctrl Pts',(-60.6458870500702,-101.661706481487,
173.149682754692));
#27127=CARTESIAN_POINT('Ctrl Pts',(-61.8039583136126,-101.443967119284,
174.32431063182));
#27128=CARTESIAN_POINT('Ctrl Pts',(-61.7940201815787,-101.350745361997,
175.985485236888));
#27129=CARTESIAN_POINT('Ctrl Pts',(-61.7840820495448,-101.25752360471,177.646659841956));
#27130=CARTESIAN_POINT('Ctrl Pts',(-60.6061345624222,-101.288819448022,
178.821287620784));
#27131=CARTESIAN_POINT('Ctrl Pts',(-59.4281870752997,-101.320115291335,
179.995915399612));
#27132=CARTESIAN_POINT('Ctrl Pts',(-57.7664343128086,-101.402988009253,
179.995915330104));
#27133=CARTESIAN_POINT('Ctrl Pts',(-56.1046815503175,-101.485860727172,
179.995915260595));
#27134=CARTESIAN_POINT('Ctrl Pts',(-54.926734160941,-101.517156560064,178.821287383467));
#27135=CARTESIAN_POINT('Ctrl Pts',(-53.7487867715645,-101.548452392956,
177.646659506339));
#27136=CARTESIAN_POINT('Ctrl Pts',(-53.7388487777644,-101.455230620932,
175.985484901271));
#27137=CARTESIAN_POINT('Ctrl Pts',(-53.7289107839643,-101.362008848909,
174.324310296203));
#27138=CARTESIAN_POINT('Ctrl Pts',(-54.8869821452528,-101.144269476286,
173.149682517375));
#27139=CARTESIAN_POINT('Ctrl Pts',(-56.0450535065414,-100.926530103662,
171.975054738546));
#27140=CARTESIAN_POINT('Ctrl Pts',(-57.6869301431984,-100.657213856433,
171.975054808055));
#27141=CARTESIAN_POINT('Ctrl Pts',(-59.3288067798556,-100.387897609204,
171.975054877564));
#27142=CARTESIAN_POINT('Ctrl Pts',(-60.486878043398,-100.170158247001,173.149682754692));
#27143=CARTESIAN_POINT('Ctrl Pts',(-61.6449493069404,-99.9524188847983,
174.32431063182));
#27144=CARTESIAN_POINT('Ctrl Pts',(-61.6350111749065,-99.8591971275113,
175.985485236888));
#27145=CARTESIAN_POINT('Ctrl Pts',(-61.6250730428726,-99.7659753702243,
177.646659841956));
#27146=CARTESIAN_POINT('Ctrl Pts',(-60.44712555575,-99.7972712135367,178.821287620784));
#27147=CARTESIAN_POINT('Ctrl Pts',(-59.2691780686275,-99.8285670568492,
179.995915399612));
#27148=CARTESIAN_POINT('Ctrl Pts',(-57.6074253061363,-99.9114397747677,
179.995915330104));
#27149=CARTESIAN_POINT('Ctrl Pts',(-55.9456725436452,-99.9943124926864,
179.995915260595));
#27150=CARTESIAN_POINT('Ctrl Pts',(-54.7677251542687,-100.025608325578,
178.821287383467));
#27151=CARTESIAN_POINT('Ctrl Pts',(-53.5897777648923,-100.05690415847,177.646659506339));
#27152=CARTESIAN_POINT('Ctrl Pts',(-53.5798397710922,-99.9636823864468,
175.985484901271));
#27153=CARTESIAN_POINT('Ctrl Pts',(-53.5699017772921,-99.8704606144232,
174.324310296203));
#27154=CARTESIAN_POINT('Ctrl Pts',(-54.7279731385806,-99.6527212418,173.149682517375));
#27155=CARTESIAN_POINT('Ctrl Pts',(-55.8860444998691,-99.4349818691769,
171.975054738546));
#27156=CARTESIAN_POINT('Ctrl Pts',(-57.5279211365262,-99.1656656219475,
171.975054808055));
#27157=CARTESIAN_POINT('Ctrl Pts',(-59.1697977731833,-98.8963493747183,
171.975054877564));
#27158=CARTESIAN_POINT('Ctrl Pts',(-60.3278690367257,-98.6786100125155,
173.149682754692));
#27159=CARTESIAN_POINT('Ctrl Pts',(-61.4859403002682,-98.4608706503128,
174.32431063182));
#27160=CARTESIAN_POINT('Ctrl Pts',(-61.4760021682342,-98.3676488930257,
175.985485236888));
#27161=CARTESIAN_POINT('Ctrl Pts',(-61.4660640362003,-98.2744271357387,
177.646659841956));
#27162=CARTESIAN_POINT('Ctrl Pts',(-60.2881165490778,-98.3057229790511,
178.821287620784));
#27163=CARTESIAN_POINT('Ctrl Pts',(-59.1101690619552,-98.3370188223636,
179.995915399612));
#27164=CARTESIAN_POINT('Ctrl Pts',(-57.4484162994641,-98.4198915402821,
179.995915330104));
#27165=CARTESIAN_POINT('Ctrl Pts',(-55.786663536973,-98.5027642582008,179.995915260595));
#27166=CARTESIAN_POINT('Ctrl Pts',(-54.6087161475965,-98.5340600910929,
178.821287383467));
#27167=CARTESIAN_POINT('Ctrl Pts',(-56.2237961054143,-113.614380048479,
178.813912075476));
#27168=CARTESIAN_POINT('Ctrl Pts',(-55.0488864554725,-113.645352038053,
177.6423391512));
#27169=CARTESIAN_POINT('Ctrl Pts',(-55.0389484614927,-113.552130266048,
175.985484901707));
#27170=CARTESIAN_POINT('Ctrl Pts',(-55.0290104675128,-113.458908494044,
174.328630652215));
#27171=CARTESIAN_POINT('Ctrl Pts',(-56.1840440891124,-113.241492964766,
173.157057825983));
#27172=CARTESIAN_POINT('Ctrl Pts',(-57.3390777107121,-113.024077435489,
171.985484999752));
#27173=CARTESIAN_POINT('Ctrl Pts',(-58.9766583348819,-112.755219171892,
171.985485069079));
#27174=CARTESIAN_POINT('Ctrl Pts',(-60.6142389590518,-112.486360908295,
171.985485138407));
#27175=CARTESIAN_POINT('Ctrl Pts',(-61.7692724831595,-112.268945389411,
173.157058062683));
#27176=CARTESIAN_POINT('Ctrl Pts',(-62.9243060072673,-112.051529870527,
174.328630986959));
#27177=CARTESIAN_POINT('Ctrl Pts',(-62.9143678754131,-111.95830811322,175.985485236451));
#27178=CARTESIAN_POINT('Ctrl Pts',(-62.9044297435589,-111.865086355914,
177.642339485944));
#27179=CARTESIAN_POINT('Ctrl Pts',(-61.7295199961253,-111.896058355881,
178.813912312176));
#27180=CARTESIAN_POINT('Ctrl Pts',(-60.5546102486917,-111.927030355848,
179.985485138407));
#27181=CARTESIAN_POINT('Ctrl Pts',(-58.8971534986878,-112.009445090134,
179.985485069079));
#27182=CARTESIAN_POINT('Ctrl Pts',(-57.2396967486839,-112.09185982442,179.985484999752));
#27183=CARTESIAN_POINT('Ctrl Pts',(-56.0647870987421,-112.122831813994,
178.813912075476));
#27184=CARTESIAN_POINT('Ctrl Pts',(-54.8898774488003,-112.153803803567,
177.6423391512));
#27185=CARTESIAN_POINT('Ctrl Pts',(-54.8799394548205,-112.060582031563,
175.985484901707));
#27186=CARTESIAN_POINT('Ctrl Pts',(-54.8700014608406,-111.967360259558,
174.328630652215));
#27187=CARTESIAN_POINT('Ctrl Pts',(-56.0250350824402,-111.749944730281,
173.157057825983));
#27188=CARTESIAN_POINT('Ctrl Pts',(-57.1800687040398,-111.532529201003,
171.985484999752));
#27189=CARTESIAN_POINT('Ctrl Pts',(-58.8176493282097,-111.263670937406,
171.985485069079));
#27190=CARTESIAN_POINT('Ctrl Pts',(-60.4552299523796,-110.994812673809,
171.985485138407));
#27191=CARTESIAN_POINT('Ctrl Pts',(-61.6102634764873,-110.777397154925,
173.157058062683));
#27192=CARTESIAN_POINT('Ctrl Pts',(-62.7652970005951,-110.559981636041,
174.328630986959));
#27193=CARTESIAN_POINT('Ctrl Pts',(-62.7553588687409,-110.466759878735,
175.985485236451));
#27194=CARTESIAN_POINT('Ctrl Pts',(-62.7454207368867,-110.373538121429,
177.642339485944));
#27195=CARTESIAN_POINT('Ctrl Pts',(-61.5705109894531,-110.404510121395,
178.813912312176));
#27196=CARTESIAN_POINT('Ctrl Pts',(-60.3956012420194,-110.435482121362,
179.985485138407));
#27197=CARTESIAN_POINT('Ctrl Pts',(-58.7381444920155,-110.517896855648,
179.985485069079));
#27198=CARTESIAN_POINT('Ctrl Pts',(-57.0806877420116,-110.600311589935,
179.985484999752));
#27199=CARTESIAN_POINT('Ctrl Pts',(-55.9057780920699,-110.631283579508,
178.813912075476));
#27200=CARTESIAN_POINT('Ctrl Pts',(-54.7308684421281,-110.662255569082,
177.6423391512));
#27201=CARTESIAN_POINT('Ctrl Pts',(-54.7209304481482,-110.569033797077,
175.985484901707));
#27202=CARTESIAN_POINT('Ctrl Pts',(-54.7109924541684,-110.475812025073,
174.328630652215));
#27203=CARTESIAN_POINT('Ctrl Pts',(-55.866026075768,-110.258396495795,173.157057825983));
#27204=CARTESIAN_POINT('Ctrl Pts',(-57.0210596973676,-110.040980966518,
171.985484999752));
#27205=CARTESIAN_POINT('Ctrl Pts',(-58.6586403215375,-109.772122702921,
171.985485069079));
#27206=CARTESIAN_POINT('Ctrl Pts',(-60.2962209457073,-109.503264439324,
171.985485138407));
#27207=CARTESIAN_POINT('Ctrl Pts',(-61.4512544698151,-109.28584892044,173.157058062683));
#27208=CARTESIAN_POINT('Ctrl Pts',(-62.6062879939228,-109.068433401555,
174.328630986959));
#27209=CARTESIAN_POINT('Ctrl Pts',(-62.5963498620687,-108.975211644249,
175.985485236451));
#27210=CARTESIAN_POINT('Ctrl Pts',(-62.5864117302145,-108.881989886943,
177.642339485944));
#27211=CARTESIAN_POINT('Ctrl Pts',(-61.4115019827808,-108.91296188691,178.813912312176));
#27212=CARTESIAN_POINT('Ctrl Pts',(-60.2365922353472,-108.943933886877,
179.985485138407));
#27213=CARTESIAN_POINT('Ctrl Pts',(-58.5791354853433,-109.026348621163,
179.985485069079));
#27214=CARTESIAN_POINT('Ctrl Pts',(-56.9216787353394,-109.108763355449,
179.985484999752));
#27215=CARTESIAN_POINT('Ctrl Pts',(-55.7467690853976,-109.139735345023,
178.813912075476));
#27216=CARTESIAN_POINT('Ctrl Pts',(-54.5718594354559,-109.170707334596,
177.6423391512));
#27217=CARTESIAN_POINT('Ctrl Pts',(-54.561921441476,-109.077485562592,175.985484901707));
#27218=CARTESIAN_POINT('Ctrl Pts',(-54.5519834474962,-108.984263790587,
174.328630652215));
#27219=CARTESIAN_POINT('Ctrl Pts',(-55.7070170690958,-108.76684826131,173.157057825983));
#27220=CARTESIAN_POINT('Ctrl Pts',(-56.8620506906954,-108.549432732032,
171.985484999752));
#27221=CARTESIAN_POINT('Ctrl Pts',(-58.4996313148652,-108.280574468435,
171.985485069079));
#27222=CARTESIAN_POINT('Ctrl Pts',(-60.1372119390351,-108.011716204838,
171.985485138407));
#27223=CARTESIAN_POINT('Ctrl Pts',(-61.2922454631428,-107.794300685954,
173.157058062683));
#27224=CARTESIAN_POINT('Ctrl Pts',(-62.4472789872506,-107.57688516707,174.328630986959));
#27225=CARTESIAN_POINT('Ctrl Pts',(-62.4373408553964,-107.483663409764,
175.985485236451));
#27226=CARTESIAN_POINT('Ctrl Pts',(-62.4274027235423,-107.390441652457,
177.642339485944));
#27227=CARTESIAN_POINT('Ctrl Pts',(-61.2524929761086,-107.421413652424,
178.813912312176));
#27228=CARTESIAN_POINT('Ctrl Pts',(-60.077583228675,-107.452385652391,179.985485138407));
#27229=CARTESIAN_POINT('Ctrl Pts',(-58.4201264786711,-107.534800386677,
179.985485069079));
#27230=CARTESIAN_POINT('Ctrl Pts',(-56.7626697286672,-107.617215120964,
179.985484999752));
#27231=CARTESIAN_POINT('Ctrl Pts',(-55.5877600787254,-107.648187110537,
178.813912075476));
#27232=CARTESIAN_POINT('Ctrl Pts',(-54.4128504287836,-107.67915910011,177.6423391512));
#27233=CARTESIAN_POINT('Ctrl Pts',(-54.4029124348038,-107.585937328106,
175.985484901707));
#27234=CARTESIAN_POINT('Ctrl Pts',(-54.3929744408239,-107.492715556102,
174.328630652215));
#27235=CARTESIAN_POINT('Ctrl Pts',(-55.5480080624235,-107.275300026824,
173.157057825983));
#27236=CARTESIAN_POINT('Ctrl Pts',(-56.7030416840231,-107.057884497547,
171.985484999752));
#27237=CARTESIAN_POINT('Ctrl Pts',(-58.340622308193,-106.78902623395,171.985485069079));
#27238=CARTESIAN_POINT('Ctrl Pts',(-59.9782029323629,-106.520167970353,
171.985485138407));
#27239=CARTESIAN_POINT('Ctrl Pts',(-61.1332364564706,-106.302752451468,
173.157058062683));
#27240=CARTESIAN_POINT('Ctrl Pts',(-62.2882699805784,-106.085336932584,
174.328630986959));
#27241=CARTESIAN_POINT('Ctrl Pts',(-62.2783318487242,-105.992115175278,
175.985485236451));
#27242=CARTESIAN_POINT('Ctrl Pts',(-62.26839371687,-105.898893417972,177.642339485944));
#27243=CARTESIAN_POINT('Ctrl Pts',(-61.0934839694364,-105.929865417939,
178.813912312176));
#27244=CARTESIAN_POINT('Ctrl Pts',(-59.9185742220028,-105.960837417905,
179.985485138407));
#27245=CARTESIAN_POINT('Ctrl Pts',(-58.2611174719989,-106.043252152192,
179.985485069079));
#27246=CARTESIAN_POINT('Ctrl Pts',(-56.603660721995,-106.125666886478,179.985484999752));
#27247=CARTESIAN_POINT('Ctrl Pts',(-55.4287510720532,-106.156638876051,
178.813912075476));
#27248=CARTESIAN_POINT('Ctrl Pts',(-54.2538414221114,-106.187610865625,
177.6423391512));
#27249=CARTESIAN_POINT('Ctrl Pts',(-54.2439034281315,-106.09438909362,175.985484901707));
#27250=CARTESIAN_POINT('Ctrl Pts',(-54.2339654341517,-106.001167321616,
174.328630652215));
#27251=CARTESIAN_POINT('Ctrl Pts',(-55.3889990557513,-105.783751792338,
173.157057825983));
#27252=CARTESIAN_POINT('Ctrl Pts',(-56.5440326773509,-105.566336263061,
171.985484999752));
#27253=CARTESIAN_POINT('Ctrl Pts',(-58.1816133015208,-105.297477999464,
171.985485069079));
#27254=CARTESIAN_POINT('Ctrl Pts',(-59.8191939256906,-105.028619735867,
171.985485138407));
#27255=CARTESIAN_POINT('Ctrl Pts',(-60.9742274497984,-104.811204216983,
173.157058062683));
#27256=CARTESIAN_POINT('Ctrl Pts',(-62.1292609739061,-104.593788698099,
174.328630986959));
#27257=CARTESIAN_POINT('Ctrl Pts',(-62.119322842052,-104.500566940792,175.985485236451));
#27258=CARTESIAN_POINT('Ctrl Pts',(-62.1093847101978,-104.407345183486,
177.642339485944));
#27259=CARTESIAN_POINT('Ctrl Pts',(-60.9344749627642,-104.438317183453,
178.813912312176));
#27260=CARTESIAN_POINT('Ctrl Pts',(-59.7595652153305,-104.46928918342,179.985485138407));
#27261=CARTESIAN_POINT('Ctrl Pts',(-58.1021084653266,-104.551703917706,
179.985485069079));
#27262=CARTESIAN_POINT('Ctrl Pts',(-56.4446517153227,-104.634118651992,
179.985484999752));
#27263=CARTESIAN_POINT('Ctrl Pts',(-55.269742065381,-104.665090641566,178.813912075476));
#27264=CARTESIAN_POINT('Ctrl Pts',(-54.0948324154392,-104.696062631139,
177.6423391512));
#27265=CARTESIAN_POINT('Ctrl Pts',(-54.0848944214593,-104.602840859135,
175.985484901707));
#27266=CARTESIAN_POINT('Ctrl Pts',(-54.0749564274795,-104.50961908713,174.328630652215));
#27267=CARTESIAN_POINT('Ctrl Pts',(-55.2299900490791,-104.292203557853,
173.157057825983));
#27268=CARTESIAN_POINT('Ctrl Pts',(-56.3850236706787,-104.074788028575,
171.985484999752));
#27269=CARTESIAN_POINT('Ctrl Pts',(-58.0226042948486,-103.805929764978,
171.985485069079));
#27270=CARTESIAN_POINT('Ctrl Pts',(-59.6601849190184,-103.537071501381,
171.985485138407));
#27271=CARTESIAN_POINT('Ctrl Pts',(-60.8152184431262,-103.319655982497,
173.157058062683));
#27272=CARTESIAN_POINT('Ctrl Pts',(-61.9702519672339,-103.102240463613,
174.328630986959));
#27273=CARTESIAN_POINT('Ctrl Pts',(-61.9603138353797,-103.009018706307,
175.985485236451));
#27274=CARTESIAN_POINT('Ctrl Pts',(-61.9503757035256,-102.915796949001,
177.642339485944));
#27275=CARTESIAN_POINT('Ctrl Pts',(-60.7754659560919,-102.946768948967,
178.813912312176));
#27276=CARTESIAN_POINT('Ctrl Pts',(-59.6005562086583,-102.977740948934,
179.985485138407));
#27277=CARTESIAN_POINT('Ctrl Pts',(-57.9430994586544,-103.06015568322,179.985485069079));
#27278=CARTESIAN_POINT('Ctrl Pts',(-56.2856427086505,-103.142570417507,
179.985484999752));
#27279=CARTESIAN_POINT('Ctrl Pts',(-55.1107330587087,-103.17354240708,178.813912075476));
#27280=CARTESIAN_POINT('Ctrl Pts',(-53.935823408767,-103.204514396654,177.6423391512));
#27281=CARTESIAN_POINT('Ctrl Pts',(-53.9258854147871,-103.111292624649,
175.985484901707));
#27282=CARTESIAN_POINT('Ctrl Pts',(-53.9159474208072,-103.018070852645,
174.328630652215));
#27283=CARTESIAN_POINT('Ctrl Pts',(-55.0709810424069,-102.800655323367,
173.157057825983));
#27284=CARTESIAN_POINT('Ctrl Pts',(-56.2260146640065,-102.58323979409,171.985484999752));
#27285=CARTESIAN_POINT('Ctrl Pts',(-57.8635952881763,-102.314381530493,
171.985485069079));
#27286=CARTESIAN_POINT('Ctrl Pts',(-59.5011759123462,-102.045523266896,
171.985485138407));
#27287=CARTESIAN_POINT('Ctrl Pts',(-60.6562094364539,-101.828107748012,
173.157058062683));
#27288=CARTESIAN_POINT('Ctrl Pts',(-61.8112429605617,-101.610692229127,
174.328630986959));
#27289=CARTESIAN_POINT('Ctrl Pts',(-61.8013048287075,-101.517470471821,
175.985485236451));
#27290=CARTESIAN_POINT('Ctrl Pts',(-61.7913666968533,-101.424248714515,
177.642339485944));
#27291=CARTESIAN_POINT('Ctrl Pts',(-60.6164569494197,-101.455220714482,
178.813912312176));
#27292=CARTESIAN_POINT('Ctrl Pts',(-59.4415472019861,-101.486192714449,
179.985485138407));
#27293=CARTESIAN_POINT('Ctrl Pts',(-57.7840904519822,-101.568607448735,
179.985485069079));
#27294=CARTESIAN_POINT('Ctrl Pts',(-56.1266337019783,-101.651022183021,
179.985484999752));
#27295=CARTESIAN_POINT('Ctrl Pts',(-54.9517240520365,-101.681994172595,
178.813912075476));
#27296=CARTESIAN_POINT('Ctrl Pts',(-53.7768144020947,-101.712966162168,
177.6423391512));
#27297=CARTESIAN_POINT('Ctrl Pts',(-53.7668764081149,-101.619744390164,
175.985484901707));
#27298=CARTESIAN_POINT('Ctrl Pts',(-53.756938414135,-101.526522618159,174.328630652215));
#27299=CARTESIAN_POINT('Ctrl Pts',(-54.9119720357346,-101.309107088882,
173.157057825983));
#27300=CARTESIAN_POINT('Ctrl Pts',(-56.0670056573342,-101.091691559604,
171.985484999752));
#27301=CARTESIAN_POINT('Ctrl Pts',(-57.7045862815041,-100.822833296007,
171.985485069079));
#27302=CARTESIAN_POINT('Ctrl Pts',(-59.342166905674,-100.55397503241,171.985485138407));
#27303=CARTESIAN_POINT('Ctrl Pts',(-60.4972004297817,-100.336559513526,
173.157058062683));
#27304=CARTESIAN_POINT('Ctrl Pts',(-61.6522339538895,-100.119143994642,
174.328630986959));
#27305=CARTESIAN_POINT('Ctrl Pts',(-61.6422958220353,-100.025922237336,
175.985485236451));
#27306=CARTESIAN_POINT('Ctrl Pts',(-61.6323576901811,-99.9327004800294,
177.642339485944));
#27307=CARTESIAN_POINT('Ctrl Pts',(-60.4574479427475,-99.9636724799962,
178.813912312176));
#27308=CARTESIAN_POINT('Ctrl Pts',(-59.2825381953138,-99.994644479963,179.985485138407));
#27309=CARTESIAN_POINT('Ctrl Pts',(-57.6250814453099,-100.077059214249,
179.985485069079));
#27310=CARTESIAN_POINT('Ctrl Pts',(-55.9676246953061,-100.159473948536,
179.985484999752));
#27311=CARTESIAN_POINT('Ctrl Pts',(-54.7927150453643,-100.190445938109,
178.813912075476));
#27312=CARTESIAN_POINT('Ctrl Pts',(-53.6178053954225,-100.221417927683,
177.6423391512));
#27313=CARTESIAN_POINT('Ctrl Pts',(-53.6078674014426,-100.128196155678,
175.985484901707));
#27314=CARTESIAN_POINT('Ctrl Pts',(-53.5979294074628,-100.034974383673,
174.328630652215));
#27315=CARTESIAN_POINT('Ctrl Pts',(-54.7529630290624,-99.817558854396,173.157057825983));
#27316=CARTESIAN_POINT('Ctrl Pts',(-55.907996650662,-99.6001433251185,171.985484999752));
#27317=CARTESIAN_POINT('Ctrl Pts',(-57.5455772748319,-99.3312850615215,
171.985485069079));
#27318=CARTESIAN_POINT('Ctrl Pts',(-59.1831578990017,-99.0624267979246,
171.985485138407));
#27319=CARTESIAN_POINT('Ctrl Pts',(-60.3381914231095,-98.8450112790404,
173.157058062683));
#27320=CARTESIAN_POINT('Ctrl Pts',(-61.4932249472172,-98.6275957601562,
174.328630986959));
#27321=CARTESIAN_POINT('Ctrl Pts',(-61.4832868153631,-98.53437400285,175.985485236451));
#27322=CARTESIAN_POINT('Ctrl Pts',(-61.4733486835089,-98.4411522455438,
177.642339485944));
#27323=CARTESIAN_POINT('Ctrl Pts',(-60.2984389360752,-98.4721242455106,
178.813912312176));
#27324=CARTESIAN_POINT('Ctrl Pts',(-59.1235291886416,-98.5030962454774,
179.985485138407));
#27325=CARTESIAN_POINT('Ctrl Pts',(-57.4660724386377,-98.5855109797636,
179.985485069079));
#27326=CARTESIAN_POINT('Ctrl Pts',(-55.8086156886338,-98.6679257140499,
179.985484999752));
#27327=CARTESIAN_POINT('Ctrl Pts',(-54.633706038692,-98.6988977036234,178.813912075476));
#27328=CARTESIAN_POINT('Ctrl Pts',(-56.2237961054143,-113.614380048479,
178.813912075476));
#27329=CARTESIAN_POINT('Ctrl Pts',(-55.0488864554725,-113.645352038053,
177.6423391512));
#27330=CARTESIAN_POINT('Ctrl Pts',(-55.0389484614927,-113.552130266048,
175.985484901707));
#27331=CARTESIAN_POINT('Ctrl Pts',(-55.0290104675128,-113.458908494044,
174.328630652215));
#27332=CARTESIAN_POINT('Ctrl Pts',(-56.1840440891124,-113.241492964766,
173.157057825983));
#27333=CARTESIAN_POINT('Ctrl Pts',(-57.3390777107121,-113.024077435489,
171.985484999752));
#27334=CARTESIAN_POINT('Ctrl Pts',(-58.9766583348819,-112.755219171892,
171.985485069079));
#27335=CARTESIAN_POINT('Ctrl Pts',(-60.6142389590518,-112.486360908295,
171.985485138407));
#27336=CARTESIAN_POINT('Ctrl Pts',(-61.7692724831595,-112.268945389411,
173.157058062683));
#27337=CARTESIAN_POINT('Ctrl Pts',(-62.9243060072673,-112.051529870527,
174.328630986959));
#27338=CARTESIAN_POINT('Ctrl Pts',(-62.9143678754131,-111.95830811322,175.985485236451));
#27339=CARTESIAN_POINT('Ctrl Pts',(-62.9044297435589,-111.865086355914,
177.642339485944));
#27340=CARTESIAN_POINT('Ctrl Pts',(-61.7295199961253,-111.896058355881,
178.813912312176));
#27341=CARTESIAN_POINT('Ctrl Pts',(-60.5546102486917,-111.927030355848,
179.985485138407));
#27342=CARTESIAN_POINT('Ctrl Pts',(-58.8971534986878,-112.009445090134,
179.985485069079));
#27343=CARTESIAN_POINT('Ctrl Pts',(-57.2396967486839,-112.09185982442,179.985484999752));
#27344=CARTESIAN_POINT('Ctrl Pts',(-56.0647870987421,-112.122831813994,
178.813912075476));
#27345=CARTESIAN_POINT('Ctrl Pts',(-54.8898774488003,-112.153803803567,
177.6423391512));
#27346=CARTESIAN_POINT('Ctrl Pts',(-54.8799394548205,-112.060582031563,
175.985484901707));
#27347=CARTESIAN_POINT('Ctrl Pts',(-54.8700014608406,-111.967360259558,
174.328630652215));
#27348=CARTESIAN_POINT('Ctrl Pts',(-56.0250350824402,-111.749944730281,
173.157057825983));
#27349=CARTESIAN_POINT('Ctrl Pts',(-57.1800687040398,-111.532529201003,
171.985484999752));
#27350=CARTESIAN_POINT('Ctrl Pts',(-58.8176493282097,-111.263670937406,
171.985485069079));
#27351=CARTESIAN_POINT('Ctrl Pts',(-60.4552299523796,-110.994812673809,
171.985485138407));
#27352=CARTESIAN_POINT('Ctrl Pts',(-61.6102634764873,-110.777397154925,
173.157058062683));
#27353=CARTESIAN_POINT('Ctrl Pts',(-62.7652970005951,-110.559981636041,
174.328630986959));
#27354=CARTESIAN_POINT('Ctrl Pts',(-62.7553588687409,-110.466759878735,
175.985485236451));
#27355=CARTESIAN_POINT('Ctrl Pts',(-62.7454207368867,-110.373538121429,
177.642339485944));
#27356=CARTESIAN_POINT('Ctrl Pts',(-61.5705109894531,-110.404510121395,
178.813912312176));
#27357=CARTESIAN_POINT('Ctrl Pts',(-60.3956012420194,-110.435482121362,
179.985485138407));
#27358=CARTESIAN_POINT('Ctrl Pts',(-58.7381444920155,-110.517896855648,
179.985485069079));
#27359=CARTESIAN_POINT('Ctrl Pts',(-57.0806877420116,-110.600311589935,
179.985484999752));
#27360=CARTESIAN_POINT('Ctrl Pts',(-55.9057780920699,-110.631283579508,
178.813912075476));
#27361=CARTESIAN_POINT('Ctrl Pts',(-54.7308684421281,-110.662255569082,
177.6423391512));
#27362=CARTESIAN_POINT('Ctrl Pts',(-54.7209304481482,-110.569033797077,
175.985484901707));
#27363=CARTESIAN_POINT('Ctrl Pts',(-54.7109924541684,-110.475812025073,
174.328630652215));
#27364=CARTESIAN_POINT('Ctrl Pts',(-55.866026075768,-110.258396495795,173.157057825983));
#27365=CARTESIAN_POINT('Ctrl Pts',(-57.0210596973676,-110.040980966518,
171.985484999752));
#27366=CARTESIAN_POINT('Ctrl Pts',(-58.6586403215375,-109.772122702921,
171.985485069079));
#27367=CARTESIAN_POINT('Ctrl Pts',(-60.2962209457073,-109.503264439324,
171.985485138407));
#27368=CARTESIAN_POINT('Ctrl Pts',(-61.4512544698151,-109.28584892044,173.157058062683));
#27369=CARTESIAN_POINT('Ctrl Pts',(-62.6062879939228,-109.068433401555,
174.328630986959));
#27370=CARTESIAN_POINT('Ctrl Pts',(-62.5963498620687,-108.975211644249,
175.985485236451));
#27371=CARTESIAN_POINT('Ctrl Pts',(-62.5864117302145,-108.881989886943,
177.642339485944));
#27372=CARTESIAN_POINT('Ctrl Pts',(-61.4115019827808,-108.91296188691,178.813912312176));
#27373=CARTESIAN_POINT('Ctrl Pts',(-60.2365922353472,-108.943933886877,
179.985485138407));
#27374=CARTESIAN_POINT('Ctrl Pts',(-58.5791354853433,-109.026348621163,
179.985485069079));
#27375=CARTESIAN_POINT('Ctrl Pts',(-56.9216787353394,-109.108763355449,
179.985484999752));
#27376=CARTESIAN_POINT('Ctrl Pts',(-55.7467690853976,-109.139735345023,
178.813912075476));
#27377=CARTESIAN_POINT('Ctrl Pts',(-54.5718594354559,-109.170707334596,
177.6423391512));
#27378=CARTESIAN_POINT('Ctrl Pts',(-54.561921441476,-109.077485562592,175.985484901707));
#27379=CARTESIAN_POINT('Ctrl Pts',(-54.5519834474962,-108.984263790587,
174.328630652215));
#27380=CARTESIAN_POINT('Ctrl Pts',(-55.7070170690958,-108.76684826131,173.157057825983));
#27381=CARTESIAN_POINT('Ctrl Pts',(-56.8620506906954,-108.549432732032,
171.985484999752));
#27382=CARTESIAN_POINT('Ctrl Pts',(-58.4996313148652,-108.280574468435,
171.985485069079));
#27383=CARTESIAN_POINT('Ctrl Pts',(-60.1372119390351,-108.011716204838,
171.985485138407));
#27384=CARTESIAN_POINT('Ctrl Pts',(-61.2922454631428,-107.794300685954,
173.157058062683));
#27385=CARTESIAN_POINT('Ctrl Pts',(-62.4472789872506,-107.57688516707,174.328630986959));
#27386=CARTESIAN_POINT('Ctrl Pts',(-62.4373408553964,-107.483663409764,
175.985485236451));
#27387=CARTESIAN_POINT('Ctrl Pts',(-62.4274027235423,-107.390441652457,
177.642339485944));
#27388=CARTESIAN_POINT('Ctrl Pts',(-61.2524929761086,-107.421413652424,
178.813912312176));
#27389=CARTESIAN_POINT('Ctrl Pts',(-60.077583228675,-107.452385652391,179.985485138407));
#27390=CARTESIAN_POINT('Ctrl Pts',(-58.4201264786711,-107.534800386677,
179.985485069079));
#27391=CARTESIAN_POINT('Ctrl Pts',(-56.7626697286672,-107.617215120964,
179.985484999752));
#27392=CARTESIAN_POINT('Ctrl Pts',(-55.5877600787254,-107.648187110537,
178.813912075476));
#27393=CARTESIAN_POINT('Ctrl Pts',(-54.4128504287836,-107.67915910011,177.6423391512));
#27394=CARTESIAN_POINT('Ctrl Pts',(-54.4029124348038,-107.585937328106,
175.985484901707));
#27395=CARTESIAN_POINT('Ctrl Pts',(-54.3929744408239,-107.492715556102,
174.328630652215));
#27396=CARTESIAN_POINT('Ctrl Pts',(-55.5480080624235,-107.275300026824,
173.157057825983));
#27397=CARTESIAN_POINT('Ctrl Pts',(-56.7030416840231,-107.057884497547,
171.985484999752));
#27398=CARTESIAN_POINT('Ctrl Pts',(-58.340622308193,-106.78902623395,171.985485069079));
#27399=CARTESIAN_POINT('Ctrl Pts',(-59.9782029323629,-106.520167970353,
171.985485138407));
#27400=CARTESIAN_POINT('Ctrl Pts',(-61.1332364564706,-106.302752451468,
173.157058062683));
#27401=CARTESIAN_POINT('Ctrl Pts',(-62.2882699805784,-106.085336932584,
174.328630986959));
#27402=CARTESIAN_POINT('Ctrl Pts',(-62.2783318487242,-105.992115175278,
175.985485236451));
#27403=CARTESIAN_POINT('Ctrl Pts',(-62.26839371687,-105.898893417972,177.642339485944));
#27404=CARTESIAN_POINT('Ctrl Pts',(-61.0934839694364,-105.929865417939,
178.813912312176));
#27405=CARTESIAN_POINT('Ctrl Pts',(-59.9185742220028,-105.960837417905,
179.985485138407));
#27406=CARTESIAN_POINT('Ctrl Pts',(-58.2611174719989,-106.043252152192,
179.985485069079));
#27407=CARTESIAN_POINT('Ctrl Pts',(-56.603660721995,-106.125666886478,179.985484999752));
#27408=CARTESIAN_POINT('Ctrl Pts',(-55.4287510720532,-106.156638876051,
178.813912075476));
#27409=CARTESIAN_POINT('Ctrl Pts',(-54.2538414221114,-106.187610865625,
177.6423391512));
#27410=CARTESIAN_POINT('Ctrl Pts',(-54.2439034281315,-106.09438909362,175.985484901707));
#27411=CARTESIAN_POINT('Ctrl Pts',(-54.2339654341517,-106.001167321616,
174.328630652215));
#27412=CARTESIAN_POINT('Ctrl Pts',(-55.3889990557513,-105.783751792338,
173.157057825983));
#27413=CARTESIAN_POINT('Ctrl Pts',(-56.5440326773509,-105.566336263061,
171.985484999752));
#27414=CARTESIAN_POINT('Ctrl Pts',(-58.1816133015208,-105.297477999464,
171.985485069079));
#27415=CARTESIAN_POINT('Ctrl Pts',(-59.8191939256906,-105.028619735867,
171.985485138407));
#27416=CARTESIAN_POINT('Ctrl Pts',(-60.9742274497984,-104.811204216983,
173.157058062683));
#27417=CARTESIAN_POINT('Ctrl Pts',(-62.1292609739061,-104.593788698099,
174.328630986959));
#27418=CARTESIAN_POINT('Ctrl Pts',(-62.119322842052,-104.500566940792,175.985485236451));
#27419=CARTESIAN_POINT('Ctrl Pts',(-62.1093847101978,-104.407345183486,
177.642339485944));
#27420=CARTESIAN_POINT('Ctrl Pts',(-60.9344749627642,-104.438317183453,
178.813912312176));
#27421=CARTESIAN_POINT('Ctrl Pts',(-59.7595652153305,-104.46928918342,179.985485138407));
#27422=CARTESIAN_POINT('Ctrl Pts',(-58.1021084653266,-104.551703917706,
179.985485069079));
#27423=CARTESIAN_POINT('Ctrl Pts',(-56.4446517153227,-104.634118651992,
179.985484999752));
#27424=CARTESIAN_POINT('Ctrl Pts',(-55.269742065381,-104.665090641566,178.813912075476));
#27425=CARTESIAN_POINT('Ctrl Pts',(-54.0948324154392,-104.696062631139,
177.6423391512));
#27426=CARTESIAN_POINT('Ctrl Pts',(-54.0848944214593,-104.602840859135,
175.985484901707));
#27427=CARTESIAN_POINT('Ctrl Pts',(-54.0749564274795,-104.50961908713,174.328630652215));
#27428=CARTESIAN_POINT('Ctrl Pts',(-55.2299900490791,-104.292203557853,
173.157057825983));
#27429=CARTESIAN_POINT('Ctrl Pts',(-56.3850236706787,-104.074788028575,
171.985484999752));
#27430=CARTESIAN_POINT('Ctrl Pts',(-58.0226042948486,-103.805929764978,
171.985485069079));
#27431=CARTESIAN_POINT('Ctrl Pts',(-59.6601849190184,-103.537071501381,
171.985485138407));
#27432=CARTESIAN_POINT('Ctrl Pts',(-60.8152184431262,-103.319655982497,
173.157058062683));
#27433=CARTESIAN_POINT('Ctrl Pts',(-61.9702519672339,-103.102240463613,
174.328630986959));
#27434=CARTESIAN_POINT('Ctrl Pts',(-61.9603138353797,-103.009018706307,
175.985485236451));
#27435=CARTESIAN_POINT('Ctrl Pts',(-61.9503757035256,-102.915796949001,
177.642339485944));
#27436=CARTESIAN_POINT('Ctrl Pts',(-60.7754659560919,-102.946768948967,
178.813912312176));
#27437=CARTESIAN_POINT('Ctrl Pts',(-59.6005562086583,-102.977740948934,
179.985485138407));
#27438=CARTESIAN_POINT('Ctrl Pts',(-57.9430994586544,-103.06015568322,179.985485069079));
#27439=CARTESIAN_POINT('Ctrl Pts',(-56.2856427086505,-103.142570417507,
179.985484999752));
#27440=CARTESIAN_POINT('Ctrl Pts',(-55.1107330587087,-103.17354240708,178.813912075476));
#27441=CARTESIAN_POINT('Ctrl Pts',(-53.935823408767,-103.204514396654,177.6423391512));
#27442=CARTESIAN_POINT('Ctrl Pts',(-53.9258854147871,-103.111292624649,
175.985484901707));
#27443=CARTESIAN_POINT('Ctrl Pts',(-53.9159474208072,-103.018070852645,
174.328630652215));
#27444=CARTESIAN_POINT('Ctrl Pts',(-55.0709810424069,-102.800655323367,
173.157057825983));
#27445=CARTESIAN_POINT('Ctrl Pts',(-56.2260146640065,-102.58323979409,171.985484999752));
#27446=CARTESIAN_POINT('Ctrl Pts',(-57.8635952881763,-102.314381530493,
171.985485069079));
#27447=CARTESIAN_POINT('Ctrl Pts',(-59.5011759123462,-102.045523266896,
171.985485138407));
#27448=CARTESIAN_POINT('Ctrl Pts',(-60.6562094364539,-101.828107748012,
173.157058062683));
#27449=CARTESIAN_POINT('Ctrl Pts',(-61.8112429605617,-101.610692229127,
174.328630986959));
#27450=CARTESIAN_POINT('Ctrl Pts',(-61.8013048287075,-101.517470471821,
175.985485236451));
#27451=CARTESIAN_POINT('Ctrl Pts',(-61.7913666968533,-101.424248714515,
177.642339485944));
#27452=CARTESIAN_POINT('Ctrl Pts',(-60.6164569494197,-101.455220714482,
178.813912312176));
#27453=CARTESIAN_POINT('Ctrl Pts',(-59.4415472019861,-101.486192714449,
179.985485138407));
#27454=CARTESIAN_POINT('Ctrl Pts',(-57.7840904519822,-101.568607448735,
179.985485069079));
#27455=CARTESIAN_POINT('Ctrl Pts',(-56.1266337019783,-101.651022183021,
179.985484999752));
#27456=CARTESIAN_POINT('Ctrl Pts',(-54.9517240520365,-101.681994172595,
178.813912075476));
#27457=CARTESIAN_POINT('Ctrl Pts',(-53.7768144020947,-101.712966162168,
177.6423391512));
#27458=CARTESIAN_POINT('Ctrl Pts',(-53.7668764081149,-101.619744390164,
175.985484901707));
#27459=CARTESIAN_POINT('Ctrl Pts',(-53.756938414135,-101.526522618159,174.328630652215));
#27460=CARTESIAN_POINT('Ctrl Pts',(-54.9119720357346,-101.309107088882,
173.157057825983));
#27461=CARTESIAN_POINT('Ctrl Pts',(-56.0670056573342,-101.091691559604,
171.985484999752));
#27462=CARTESIAN_POINT('Ctrl Pts',(-57.7045862815041,-100.822833296007,
171.985485069079));
#27463=CARTESIAN_POINT('Ctrl Pts',(-59.342166905674,-100.55397503241,171.985485138407));
#27464=CARTESIAN_POINT('Ctrl Pts',(-60.4972004297817,-100.336559513526,
173.157058062683));
#27465=CARTESIAN_POINT('Ctrl Pts',(-61.6522339538895,-100.119143994642,
174.328630986959));
#27466=CARTESIAN_POINT('Ctrl Pts',(-61.6422958220353,-100.025922237336,
175.985485236451));
#27467=CARTESIAN_POINT('Ctrl Pts',(-61.6323576901811,-99.9327004800294,
177.642339485944));
#27468=CARTESIAN_POINT('Ctrl Pts',(-60.4574479427475,-99.9636724799962,
178.813912312176));
#27469=CARTESIAN_POINT('Ctrl Pts',(-59.2825381953138,-99.994644479963,179.985485138407));
#27470=CARTESIAN_POINT('Ctrl Pts',(-57.6250814453099,-100.077059214249,
179.985485069079));
#27471=CARTESIAN_POINT('Ctrl Pts',(-55.9676246953061,-100.159473948536,
179.985484999752));
#27472=CARTESIAN_POINT('Ctrl Pts',(-54.7927150453643,-100.190445938109,
178.813912075476));
#27473=CARTESIAN_POINT('Ctrl Pts',(-53.6178053954225,-100.221417927683,
177.6423391512));
#27474=CARTESIAN_POINT('Ctrl Pts',(-53.6078674014426,-100.128196155678,
175.985484901707));
#27475=CARTESIAN_POINT('Ctrl Pts',(-53.5979294074628,-100.034974383673,
174.328630652215));
#27476=CARTESIAN_POINT('Ctrl Pts',(-54.7529630290624,-99.817558854396,173.157057825983));
#27477=CARTESIAN_POINT('Ctrl Pts',(-55.907996650662,-99.6001433251185,171.985484999752));
#27478=CARTESIAN_POINT('Ctrl Pts',(-57.5455772748319,-99.3312850615215,
171.985485069079));
#27479=CARTESIAN_POINT('Ctrl Pts',(-59.1831578990017,-99.0624267979246,
171.985485138407));
#27480=CARTESIAN_POINT('Ctrl Pts',(-60.3381914231095,-98.8450112790404,
173.157058062683));
#27481=CARTESIAN_POINT('Ctrl Pts',(-61.4932249472172,-98.6275957601562,
174.328630986959));
#27482=CARTESIAN_POINT('Ctrl Pts',(-61.4832868153631,-98.53437400285,175.985485236451));
#27483=CARTESIAN_POINT('Ctrl Pts',(-61.4733486835089,-98.4411522455438,
177.642339485944));
#27484=CARTESIAN_POINT('Ctrl Pts',(-60.2984389360752,-98.4721242455106,
178.813912312176));
#27485=CARTESIAN_POINT('Ctrl Pts',(-59.1235291886416,-98.5030962454774,
179.985485138407));
#27486=CARTESIAN_POINT('Ctrl Pts',(-57.4660724386377,-98.5855109797636,
179.985485069079));
#27487=CARTESIAN_POINT('Ctrl Pts',(-55.8086156886338,-98.6679257140499,
179.985484999752));
#27488=CARTESIAN_POINT('Ctrl Pts',(-54.633706038692,-98.6988977036234,178.813912075476));
#27489=CARTESIAN_POINT('Ctrl Pts',(-56.9964983346804,-113.864655531781,
178.072094410988));
#27490=CARTESIAN_POINT('Ctrl Pts',(-56.1271283009022,-113.863054956993,
177.207792449865));
#27491=CARTESIAN_POINT('Ctrl Pts',(-56.117190288842,-113.769833186916,175.985484945604));
#27492=CARTESIAN_POINT('Ctrl Pts',(-56.1072522767819,-113.676611416839,
174.763177441344));
#27493=CARTESIAN_POINT('Ctrl Pts',(-56.9567462566485,-113.491768454648,
173.89887555255));
#27494=CARTESIAN_POINT('Ctrl Pts',(-57.8062402365152,-113.306925492458,
173.034573663757));
#27495=CARTESIAN_POINT('Ctrl Pts',(-59.011722573584,-113.084131793069,173.034573714903));
#27496=CARTESIAN_POINT('Ctrl Pts',(-60.2172049106529,-112.86133809368,173.034573766048));
#27497=CARTESIAN_POINT('Ctrl Pts',(-61.0666988185971,-112.676495139156,
173.898875727171));
#27498=CARTESIAN_POINT('Ctrl Pts',(-61.9161927265413,-112.491652184633,
174.763177688294));
#27499=CARTESIAN_POINT('Ctrl Pts',(-61.9062546127674,-112.398430425399,
175.985485192554));
#27500=CARTESIAN_POINT('Ctrl Pts',(-61.8963164989935,-112.305208666166,
177.207792696815));
#27501=CARTESIAN_POINT('Ctrl Pts',(-61.0269463932928,-112.303608099046,
178.072094585608));
#27502=CARTESIAN_POINT('Ctrl Pts',(-60.1575762875921,-112.302007531926,
178.936396474401));
#27503=CARTESIAN_POINT('Ctrl Pts',(-58.9322178246893,-112.338357702004,
178.936396423256));
#27504=CARTESIAN_POINT('Ctrl Pts',(-57.7068593617864,-112.374707872082,
178.936396372111));
#27505=CARTESIAN_POINT('Ctrl Pts',(-56.8374893280082,-112.373107297295,
178.072094410988));
#27506=CARTESIAN_POINT('Ctrl Pts',(-55.9681192942299,-112.371506722508,
177.207792449865));
#27507=CARTESIAN_POINT('Ctrl Pts',(-55.9581812821698,-112.278284952431,
175.985484945604));
#27508=CARTESIAN_POINT('Ctrl Pts',(-55.9482432701096,-112.185063182354,
174.763177441344));
#27509=CARTESIAN_POINT('Ctrl Pts',(-56.7977372499763,-112.000220220163,
173.89887555255));
#27510=CARTESIAN_POINT('Ctrl Pts',(-57.647231229843,-111.815377257972,173.034573663757));
#27511=CARTESIAN_POINT('Ctrl Pts',(-58.8527135669118,-111.592583558583,
173.034573714903));
#27512=CARTESIAN_POINT('Ctrl Pts',(-60.0581959039807,-111.369789859194,
173.034573766048));
#27513=CARTESIAN_POINT('Ctrl Pts',(-60.9076898119249,-111.184946904671,
173.898875727171));
#27514=CARTESIAN_POINT('Ctrl Pts',(-61.7571837198691,-111.000103950148,
174.763177688294));
#27515=CARTESIAN_POINT('Ctrl Pts',(-61.7472456060952,-110.906882190914,
175.985485192554));
#27516=CARTESIAN_POINT('Ctrl Pts',(-61.7373074923213,-110.81366043168,177.207792696815));
#27517=CARTESIAN_POINT('Ctrl Pts',(-60.8679373866206,-110.81205986456,178.072094585608));
#27518=CARTESIAN_POINT('Ctrl Pts',(-59.9985672809199,-110.81045929744,178.936396474401));
#27519=CARTESIAN_POINT('Ctrl Pts',(-58.7732088180171,-110.846809467519,
178.936396423256));
#27520=CARTESIAN_POINT('Ctrl Pts',(-57.5478503551142,-110.883159637597,
178.936396372111));
#27521=CARTESIAN_POINT('Ctrl Pts',(-56.6784803213359,-110.881559062809,
178.072094410988));
#27522=CARTESIAN_POINT('Ctrl Pts',(-55.8091102875577,-110.879958488022,
177.207792449865));
#27523=CARTESIAN_POINT('Ctrl Pts',(-55.7991722754976,-110.786736717945,
175.985484945604));
#27524=CARTESIAN_POINT('Ctrl Pts',(-55.7892342634374,-110.693514947868,
174.763177441344));
#27525=CARTESIAN_POINT('Ctrl Pts',(-56.6387282433041,-110.508671985677,
173.89887555255));
#27526=CARTESIAN_POINT('Ctrl Pts',(-57.4882222231708,-110.323829023487,
173.034573663757));
#27527=CARTESIAN_POINT('Ctrl Pts',(-58.6937045602396,-110.101035324098,
173.034573714903));
#27528=CARTESIAN_POINT('Ctrl Pts',(-59.8991868973084,-109.878241624709,
173.034573766048));
#27529=CARTESIAN_POINT('Ctrl Pts',(-60.7486808052526,-109.693398670185,
173.898875727171));
#27530=CARTESIAN_POINT('Ctrl Pts',(-61.5981747131968,-109.508555715662,
174.763177688294));
#27531=CARTESIAN_POINT('Ctrl Pts',(-61.588236599423,-109.415333956428,175.985485192554));
#27532=CARTESIAN_POINT('Ctrl Pts',(-61.5782984856491,-109.322112197195,
177.207792696815));
#27533=CARTESIAN_POINT('Ctrl Pts',(-60.7089283799484,-109.320511630075,
178.072094585608));
#27534=CARTESIAN_POINT('Ctrl Pts',(-59.8395582742477,-109.318911062955,
178.936396474401));
#27535=CARTESIAN_POINT('Ctrl Pts',(-58.6141998113448,-109.355261233033,
178.936396423256));
#27536=CARTESIAN_POINT('Ctrl Pts',(-57.388841348442,-109.391611403111,178.936396372111));
#27537=CARTESIAN_POINT('Ctrl Pts',(-56.5194713146637,-109.390010828324,
178.072094410988));
#27538=CARTESIAN_POINT('Ctrl Pts',(-55.6501012808855,-109.388410253536,
177.207792449865));
#27539=CARTESIAN_POINT('Ctrl Pts',(-55.6401632688253,-109.295188483459,
175.985484945604));
#27540=CARTESIAN_POINT('Ctrl Pts',(-55.6302252567652,-109.201966713382,
174.763177441344));
#27541=CARTESIAN_POINT('Ctrl Pts',(-56.4797192366319,-109.017123751192,
173.89887555255));
#27542=CARTESIAN_POINT('Ctrl Pts',(-57.3292132164985,-108.832280789001,
173.034573663757));
#27543=CARTESIAN_POINT('Ctrl Pts',(-58.5346955535674,-108.609487089612,
173.034573714903));
#27544=CARTESIAN_POINT('Ctrl Pts',(-59.7401778906362,-108.386693390223,
173.034573766048));
#27545=CARTESIAN_POINT('Ctrl Pts',(-60.5896717985804,-108.2018504357,173.898875727171));
#27546=CARTESIAN_POINT('Ctrl Pts',(-61.4391657065246,-108.017007481176,
174.763177688294));
#27547=CARTESIAN_POINT('Ctrl Pts',(-61.4292275927507,-107.923785721943,
175.985485192554));
#27548=CARTESIAN_POINT('Ctrl Pts',(-61.4192894789769,-107.830563962709,
177.207792696815));
#27549=CARTESIAN_POINT('Ctrl Pts',(-60.5499193732762,-107.828963395589,
178.072094585608));
#27550=CARTESIAN_POINT('Ctrl Pts',(-59.6805492675755,-107.827362828469,
178.936396474401));
#27551=CARTESIAN_POINT('Ctrl Pts',(-58.4551908046726,-107.863712998547,
178.936396423256));
#27552=CARTESIAN_POINT('Ctrl Pts',(-57.2298323417698,-107.900063168626,
178.936396372111));
#27553=CARTESIAN_POINT('Ctrl Pts',(-56.3604623079915,-107.898462593838,
178.072094410988));
#27554=CARTESIAN_POINT('Ctrl Pts',(-55.4910922742133,-107.896862019051,
177.207792449865));
#27555=CARTESIAN_POINT('Ctrl Pts',(-55.4811542621531,-107.803640248974,
175.985484945604));
#27556=CARTESIAN_POINT('Ctrl Pts',(-55.471216250093,-107.710418478897,174.763177441344));
#27557=CARTESIAN_POINT('Ctrl Pts',(-56.3207102299596,-107.525575516706,
173.89887555255));
#27558=CARTESIAN_POINT('Ctrl Pts',(-57.1702042098263,-107.340732554515,
173.034573663757));
#27559=CARTESIAN_POINT('Ctrl Pts',(-58.3756865468951,-107.117938855126,
173.034573714903));
#27560=CARTESIAN_POINT('Ctrl Pts',(-59.581168883964,-106.895145155737,173.034573766048));
#27561=CARTESIAN_POINT('Ctrl Pts',(-60.4306627919082,-106.710302201214,
173.898875727171));
#27562=CARTESIAN_POINT('Ctrl Pts',(-61.2801566998524,-106.525459246691,
174.763177688294));
#27563=CARTESIAN_POINT('Ctrl Pts',(-61.2702185860785,-106.432237487457,
175.985485192554));
#27564=CARTESIAN_POINT('Ctrl Pts',(-61.2602804723046,-106.339015728223,
177.207792696815));
#27565=CARTESIAN_POINT('Ctrl Pts',(-60.3909103666039,-106.337415161103,
178.072094585608));
#27566=CARTESIAN_POINT('Ctrl Pts',(-59.5215402609032,-106.335814593983,
178.936396474401));
#27567=CARTESIAN_POINT('Ctrl Pts',(-58.2961817980004,-106.372164764062,
178.936396423256));
#27568=CARTESIAN_POINT('Ctrl Pts',(-57.0708233350975,-106.40851493414,178.936396372111));
#27569=CARTESIAN_POINT('Ctrl Pts',(-56.2014533013193,-106.406914359353,
178.072094410988));
#27570=CARTESIAN_POINT('Ctrl Pts',(-55.332083267541,-106.405313784565,177.207792449865));
#27571=CARTESIAN_POINT('Ctrl Pts',(-55.3221452554809,-106.312092014488,
175.985484945604));
#27572=CARTESIAN_POINT('Ctrl Pts',(-55.3122072434207,-106.218870244411,
174.763177441344));
#27573=CARTESIAN_POINT('Ctrl Pts',(-56.1617012232874,-106.034027282221,
173.89887555255));
#27574=CARTESIAN_POINT('Ctrl Pts',(-57.0111952031541,-105.84918432003,173.034573663757));
#27575=CARTESIAN_POINT('Ctrl Pts',(-58.2166775402229,-105.626390620641,
173.034573714903));
#27576=CARTESIAN_POINT('Ctrl Pts',(-59.4221598772917,-105.403596921252,
173.034573766048));
#27577=CARTESIAN_POINT('Ctrl Pts',(-60.2716537852359,-105.218753966728,
173.898875727171));
#27578=CARTESIAN_POINT('Ctrl Pts',(-61.1211476931802,-105.033911012205,
174.763177688294));
#27579=CARTESIAN_POINT('Ctrl Pts',(-61.1112095794063,-104.940689252971,
175.985485192554));
#27580=CARTESIAN_POINT('Ctrl Pts',(-61.1012714656324,-104.847467493738,
177.207792696815));
#27581=CARTESIAN_POINT('Ctrl Pts',(-60.2319013599317,-104.845866926618,
178.072094585608));
#27582=CARTESIAN_POINT('Ctrl Pts',(-59.362531254231,-104.844266359498,178.936396474401));
#27583=CARTESIAN_POINT('Ctrl Pts',(-58.1371727913281,-104.880616529576,
178.936396423256));
#27584=CARTESIAN_POINT('Ctrl Pts',(-56.9118143284253,-104.916966699654,
178.936396372111));
#27585=CARTESIAN_POINT('Ctrl Pts',(-56.042444294647,-104.915366124867,178.072094410988));
#27586=CARTESIAN_POINT('Ctrl Pts',(-55.1730742608688,-104.91376555008,177.207792449865));
#27587=CARTESIAN_POINT('Ctrl Pts',(-55.1631362488087,-104.820543780003,
175.985484945604));
#27588=CARTESIAN_POINT('Ctrl Pts',(-55.1531982367485,-104.727322009926,
174.763177441344));
#27589=CARTESIAN_POINT('Ctrl Pts',(-56.0026922166152,-104.542479047735,
173.89887555255));
#27590=CARTESIAN_POINT('Ctrl Pts',(-56.8521861964818,-104.357636085544,
173.034573663757));
#27591=CARTESIAN_POINT('Ctrl Pts',(-58.0576685335507,-104.134842386155,
173.034573714903));
#27592=CARTESIAN_POINT('Ctrl Pts',(-59.2631508706195,-103.912048686766,
173.034573766048));
#27593=CARTESIAN_POINT('Ctrl Pts',(-60.1126447785637,-103.727205732243,
173.898875727171));
#27594=CARTESIAN_POINT('Ctrl Pts',(-60.9621386865079,-103.54236277772,174.763177688294));
#27595=CARTESIAN_POINT('Ctrl Pts',(-60.952200572734,-103.449141018486,175.985485192554));
#27596=CARTESIAN_POINT('Ctrl Pts',(-60.9422624589602,-103.355919259252,
177.207792696815));
#27597=CARTESIAN_POINT('Ctrl Pts',(-60.0728923532595,-103.354318692132,
178.072094585608));
#27598=CARTESIAN_POINT('Ctrl Pts',(-59.2035222475588,-103.352718125012,
178.936396474401));
#27599=CARTESIAN_POINT('Ctrl Pts',(-57.9781637846559,-103.389068295091,
178.936396423256));
#27600=CARTESIAN_POINT('Ctrl Pts',(-56.7528053217531,-103.425418465169,
178.936396372111));
#27601=CARTESIAN_POINT('Ctrl Pts',(-55.8834352879748,-103.423817890381,
178.072094410988));
#27602=CARTESIAN_POINT('Ctrl Pts',(-55.0140652541966,-103.422217315594,
177.207792449865));
#27603=CARTESIAN_POINT('Ctrl Pts',(-55.0041272421364,-103.328995545517,
175.985484945604));
#27604=CARTESIAN_POINT('Ctrl Pts',(-54.9941892300763,-103.23577377544,174.763177441344));
#27605=CARTESIAN_POINT('Ctrl Pts',(-55.8436832099429,-103.050930813249,
173.89887555255));
#27606=CARTESIAN_POINT('Ctrl Pts',(-56.6931771898096,-102.866087851059,
173.034573663757));
#27607=CARTESIAN_POINT('Ctrl Pts',(-57.8986595268784,-102.64329415167,173.034573714903));
#27608=CARTESIAN_POINT('Ctrl Pts',(-59.1041418639473,-102.420500452281,
173.034573766048));
#27609=CARTESIAN_POINT('Ctrl Pts',(-59.9536357718915,-102.235657497757,
173.898875727171));
#27610=CARTESIAN_POINT('Ctrl Pts',(-60.8031296798357,-102.050814543234,
174.763177688294));
#27611=CARTESIAN_POINT('Ctrl Pts',(-60.7931915660618,-101.957592784,175.985485192554));
#27612=CARTESIAN_POINT('Ctrl Pts',(-60.783253452288,-101.864371024767,177.207792696815));
#27613=CARTESIAN_POINT('Ctrl Pts',(-59.9138833465873,-101.862770457647,
178.072094585608));
#27614=CARTESIAN_POINT('Ctrl Pts',(-59.0445132408866,-101.861169890527,
178.936396474401));
#27615=CARTESIAN_POINT('Ctrl Pts',(-57.8191547779837,-101.897520060605,
178.936396423256));
#27616=CARTESIAN_POINT('Ctrl Pts',(-56.5937963150808,-101.933870230683,
178.936396372111));
#27617=CARTESIAN_POINT('Ctrl Pts',(-55.7244262813026,-101.932269655896,
178.072094410988));
#27618=CARTESIAN_POINT('Ctrl Pts',(-54.8550562475244,-101.930669081108,
177.207792449865));
#27619=CARTESIAN_POINT('Ctrl Pts',(-54.8451182354642,-101.837447311031,
175.985484945604));
#27620=CARTESIAN_POINT('Ctrl Pts',(-54.8351802234041,-101.744225540954,
174.763177441344));
#27621=CARTESIAN_POINT('Ctrl Pts',(-55.6846742032707,-101.559382578764,
173.89887555255));
#27622=CARTESIAN_POINT('Ctrl Pts',(-56.5341681831374,-101.374539616573,
173.034573663757));
#27623=CARTESIAN_POINT('Ctrl Pts',(-57.7396505202062,-101.151745917184,
173.034573714903));
#27624=CARTESIAN_POINT('Ctrl Pts',(-58.9451328572751,-100.928952217795,
173.034573766048));
#27625=CARTESIAN_POINT('Ctrl Pts',(-59.7946267652193,-100.744109263272,
173.898875727171));
#27626=CARTESIAN_POINT('Ctrl Pts',(-60.6441206731635,-100.559266308748,
174.763177688294));
#27627=CARTESIAN_POINT('Ctrl Pts',(-60.6341825593896,-100.466044549515,
175.985485192554));
#27628=CARTESIAN_POINT('Ctrl Pts',(-60.6242444456157,-100.372822790281,
177.207792696815));
#27629=CARTESIAN_POINT('Ctrl Pts',(-59.754874339915,-100.371222223161,178.072094585608));
#27630=CARTESIAN_POINT('Ctrl Pts',(-58.8855042342143,-100.369621656041,
178.936396474401));
#27631=CARTESIAN_POINT('Ctrl Pts',(-57.6601457713115,-100.405971826119,
178.936396423256));
#27632=CARTESIAN_POINT('Ctrl Pts',(-56.4347873084086,-100.442321996198,
178.936396372111));
#27633=CARTESIAN_POINT('Ctrl Pts',(-55.5654172746304,-100.44072142141,178.072094410988));
#27634=CARTESIAN_POINT('Ctrl Pts',(-54.6960472408521,-100.439120846623,
177.207792449865));
#27635=CARTESIAN_POINT('Ctrl Pts',(-54.686109228792,-100.345899076546,175.985484945604));
#27636=CARTESIAN_POINT('Ctrl Pts',(-54.6761712167318,-100.252677306469,
174.763177441344));
#27637=CARTESIAN_POINT('Ctrl Pts',(-55.5256651965985,-100.067834344278,
173.89887555255));
#27638=CARTESIAN_POINT('Ctrl Pts',(-56.3751591764652,-99.8829913820874,
173.034573663757));
#27639=CARTESIAN_POINT('Ctrl Pts',(-57.580641513534,-99.6601976826983,173.034573714903));
#27640=CARTESIAN_POINT('Ctrl Pts',(-58.7861238506028,-99.4374039833093,
173.034573766048));
#27641=CARTESIAN_POINT('Ctrl Pts',(-59.635617758547,-99.252561028786,173.898875727171));
#27642=CARTESIAN_POINT('Ctrl Pts',(-60.4851116664912,-99.0677180742627,
174.763177688294));
#27643=CARTESIAN_POINT('Ctrl Pts',(-60.4751735527174,-98.9744963150291,
175.985485192554));
#27644=CARTESIAN_POINT('Ctrl Pts',(-60.4652354389435,-98.8812745557954,
177.207792696815));
#27645=CARTESIAN_POINT('Ctrl Pts',(-59.5958653332428,-98.8796739886754,
178.072094585608));
#27646=CARTESIAN_POINT('Ctrl Pts',(-58.7264952275421,-98.8780734215554,
178.936396474401));
#27647=CARTESIAN_POINT('Ctrl Pts',(-57.5011367646392,-98.9144235916337,
178.936396423256));
#27648=CARTESIAN_POINT('Ctrl Pts',(-56.2757783017364,-98.9507737617121,
178.936396372111));
#27649=CARTESIAN_POINT('Ctrl Pts',(-55.4064082679581,-98.9491731869247,
178.072094410988));
#27650=CARTESIAN_POINT('Ctrl Pts',(-61.5476086001415,-107.415572466264,
178.485485069079));
#27651=CARTESIAN_POINT('Ctrl Pts',(-61.4090363957847,-107.417286984142,
178.657813499464));
#27652=CARTESIAN_POINT('Ctrl Pts',(-61.2524929761086,-107.421413652424,
178.813912312176));
#27653=CARTESIAN_POINT('Ctrl Pts',(-60.077583228675,-107.452385652391,179.985485138407));
#27654=CARTESIAN_POINT('Ctrl Pts',(-58.4201264786711,-107.534800386677,
179.985485069079));
#27655=CARTESIAN_POINT('Ctrl Pts',(-56.7626697286672,-107.617215120964,
179.985484999752));
#27656=CARTESIAN_POINT('Ctrl Pts',(-55.5877600787254,-107.648187110537,
178.813912075476));
#27657=CARTESIAN_POINT('Ctrl Pts',(-54.4128504287836,-107.67915910011,177.6423391512));
#27658=CARTESIAN_POINT('Ctrl Pts',(-54.4029124348038,-107.585937328106,
175.985484901707));
#27659=CARTESIAN_POINT('Ctrl Pts',(-54.3929744408239,-107.492715556101,
174.328630652215));
#27660=CARTESIAN_POINT('Ctrl Pts',(-55.5480080624235,-107.275300026824,
173.157057825983));
#27661=CARTESIAN_POINT('Ctrl Pts',(-56.7030416840231,-107.057884497547,
171.985484999752));
#27662=CARTESIAN_POINT('Ctrl Pts',(-58.340622308193,-106.78902623395,171.985485069079));
#27663=CARTESIAN_POINT('Ctrl Pts',(-59.9782029323629,-106.520167970353,
171.985485138407));
#27664=CARTESIAN_POINT('Ctrl Pts',(-61.1332364564706,-106.302752451468,
173.157058062683));
#27665=CARTESIAN_POINT('Ctrl Pts',(-61.2871314774238,-106.273784317526,
173.313156769748));
#27666=CARTESIAN_POINT('Ctrl Pts',(-61.4229506813946,-106.246246888344,
173.485485069079));
#27667=CARTESIAN_POINT('Ctrl Pts',(-56.8733667677527,-112.709647553905,
178.072094410988));
#27668=CARTESIAN_POINT('Ctrl Pts',(-56.0039967339745,-112.708046979118,
177.207792449865));
#27669=CARTESIAN_POINT('Ctrl Pts',(-55.9940587219143,-112.614825209041,
175.985484945604));
#27670=CARTESIAN_POINT('Ctrl Pts',(-55.9841207098542,-112.521603438964,
174.763177441344));
#27671=CARTESIAN_POINT('Ctrl Pts',(-56.8336146897208,-112.336760476773,
173.89887555255));
#27672=CARTESIAN_POINT('Ctrl Pts',(-57.6831086695875,-112.151917514582,
173.034573663757));
#27673=CARTESIAN_POINT('Ctrl Pts',(-58.8885910066563,-111.929123815193,
173.034573714903));
#27674=CARTESIAN_POINT('Ctrl Pts',(-60.0940733437252,-111.706330115804,
173.034573766048));
#27675=CARTESIAN_POINT('Ctrl Pts',(-60.9435672516694,-111.521487161281,
173.898875727171));
#27676=CARTESIAN_POINT('Ctrl Pts',(-61.7930611596136,-111.336644206758,
174.763177688294));
#27677=CARTESIAN_POINT('Ctrl Pts',(-61.7831230458397,-111.243422447524,
175.985485192554));
#27678=CARTESIAN_POINT('Ctrl Pts',(-61.7731849320658,-111.15020068829,177.207792696815));
#27679=CARTESIAN_POINT('Ctrl Pts',(-60.9038148263651,-111.14860012117,178.072094585608));
#27680=CARTESIAN_POINT('Ctrl Pts',(-60.0344447206644,-111.14699955405,178.936396474401));
#27681=CARTESIAN_POINT('Ctrl Pts',(-58.8090862577616,-111.183349724129,
178.936396423256));
#27682=CARTESIAN_POINT('Ctrl Pts',(-57.5837277948587,-111.219699894207,
178.936396372111));
#27683=CARTESIAN_POINT('Ctrl Pts',(-56.7143577610805,-111.21809931942,178.072094410988));
#27684=CARTESIAN_POINT('Ctrl Pts',(-55.8449877273022,-111.216498744632,
177.207792449865));
#27685=CARTESIAN_POINT('Ctrl Pts',(-55.8350497152421,-111.123276974555,
175.985484945604));
#27686=CARTESIAN_POINT('Ctrl Pts',(-55.8251117031819,-111.030055204478,
174.763177441344));
#27687=CARTESIAN_POINT('Ctrl Pts',(-56.6746056830486,-110.845212242287,
173.89887555255));
#27688=CARTESIAN_POINT('Ctrl Pts',(-57.5240996629153,-110.660369280097,
173.034573663757));
#27689=CARTESIAN_POINT('Ctrl Pts',(-58.7295819999841,-110.437575580708,
173.034573714903));
#27690=CARTESIAN_POINT('Ctrl Pts',(-59.9350643370529,-110.214781881319,
173.034573766048));
#27691=CARTESIAN_POINT('Ctrl Pts',(-60.7845582449971,-110.029938926795,
173.898875727171));
#27692=CARTESIAN_POINT('Ctrl Pts',(-61.6340521529414,-109.845095972272,
174.763177688294));
#27693=CARTESIAN_POINT('Ctrl Pts',(-61.6241140391675,-109.751874213038,
175.985485192554));
#27694=CARTESIAN_POINT('Ctrl Pts',(-61.6141759253936,-109.658652453805,
177.207792696815));
#27695=CARTESIAN_POINT('Ctrl Pts',(-60.7448058196929,-109.657051886685,
178.072094585608));
#27696=CARTESIAN_POINT('Ctrl Pts',(-59.8754357139922,-109.655451319565,
178.936396474401));
#27697=CARTESIAN_POINT('Ctrl Pts',(-58.6500772510893,-109.691801489643,
178.936396423256));
#27698=CARTESIAN_POINT('Ctrl Pts',(-57.4247187881865,-109.728151659721,
178.936396372111));
#27699=CARTESIAN_POINT('Ctrl Pts',(-56.5553487544082,-109.726551084934,
178.072094410988));
#27700=CARTESIAN_POINT('Ctrl Pts',(-55.68597872063,-109.724950510147,177.207792449865));
#27701=CARTESIAN_POINT('Ctrl Pts',(-55.6760407085698,-109.63172874007,175.985484945604));
#27702=CARTESIAN_POINT('Ctrl Pts',(-55.6661026965097,-109.538506969993,
174.763177441344));
#27703=CARTESIAN_POINT('Ctrl Pts',(-56.5155966763764,-109.353664007802,
173.89887555255));
#27704=CARTESIAN_POINT('Ctrl Pts',(-57.365090656243,-109.168821045611,173.034573663757));
#27705=CARTESIAN_POINT('Ctrl Pts',(-58.5705729933119,-108.946027346222,
173.034573714903));
#27706=CARTESIAN_POINT('Ctrl Pts',(-59.7760553303807,-108.723233646833,
173.034573766048));
#27707=CARTESIAN_POINT('Ctrl Pts',(-60.6255492383249,-108.53839069231,173.898875727171));
#27708=CARTESIAN_POINT('Ctrl Pts',(-61.4750431462691,-108.353547737786,
174.763177688294));
#27709=CARTESIAN_POINT('Ctrl Pts',(-61.4651050324952,-108.260325978553,
175.985485192554));
#27710=CARTESIAN_POINT('Ctrl Pts',(-61.4551669187214,-108.167104219319,
177.207792696815));
#27711=CARTESIAN_POINT('Ctrl Pts',(-60.5857968130207,-108.165503652199,
178.072094585608));
#27712=CARTESIAN_POINT('Ctrl Pts',(-59.71642670732,-108.163903085079,178.936396474401));
#27713=CARTESIAN_POINT('Ctrl Pts',(-58.4910682444171,-108.200253255158,
178.936396423256));
#27714=CARTESIAN_POINT('Ctrl Pts',(-57.2657097815143,-108.236603425236,
178.936396372111));
#27715=CARTESIAN_POINT('Ctrl Pts',(-56.396339747736,-108.235002850448,178.072094410988));
#27716=CARTESIAN_POINT('Ctrl Pts',(-55.5269697139578,-108.233402275661,
177.207792449865));
#27717=CARTESIAN_POINT('Ctrl Pts',(-55.5170317018976,-108.140180505584,
175.985484945604));
#27718=CARTESIAN_POINT('Ctrl Pts',(-55.5070936898375,-108.046958735507,
174.763177441344));
#27719=CARTESIAN_POINT('Ctrl Pts',(-56.3565876697041,-107.862115773316,
173.89887555255));
#27720=CARTESIAN_POINT('Ctrl Pts',(-57.2060816495708,-107.677272811126,
173.034573663757));
#27721=CARTESIAN_POINT('Ctrl Pts',(-58.4115639866396,-107.454479111736,
173.034573714903));
#27722=CARTESIAN_POINT('Ctrl Pts',(-59.6170463237085,-107.231685412347,
173.034573766048));
#27723=CARTESIAN_POINT('Ctrl Pts',(-60.4665402316527,-107.046842457824,
173.898875727171));
#27724=CARTESIAN_POINT('Ctrl Pts',(-61.3160341395969,-106.861999503301,
174.763177688294));
#27725=CARTESIAN_POINT('Ctrl Pts',(-61.306096025823,-106.768777744067,175.985485192554));
#27726=CARTESIAN_POINT('Ctrl Pts',(-61.2961579120492,-106.675555984834,
177.207792696815));
#27727=CARTESIAN_POINT('Ctrl Pts',(-60.4267878063484,-106.673955417714,
178.072094585608));
#27728=CARTESIAN_POINT('Ctrl Pts',(-59.5574177006478,-106.672354850594,
178.936396474401));
#27729=CARTESIAN_POINT('Ctrl Pts',(-58.3320592377449,-106.708705020672,
178.936396423256));
#27730=CARTESIAN_POINT('Ctrl Pts',(-57.106700774842,-106.74505519075,178.936396372111));
#27731=CARTESIAN_POINT('Ctrl Pts',(-56.2373307410638,-106.743454615963,
178.072094410988));
#27732=CARTESIAN_POINT('Ctrl Pts',(-55.3679607072856,-106.741854041175,
177.207792449865));
#27733=CARTESIAN_POINT('Ctrl Pts',(-55.3580226952254,-106.648632271098,
175.985484945604));
#27734=CARTESIAN_POINT('Ctrl Pts',(-55.3480846831652,-106.555410501021,
174.763177441344));
#27735=CARTESIAN_POINT('Ctrl Pts',(-56.1975786630319,-106.370567538831,
173.89887555255));
#27736=CARTESIAN_POINT('Ctrl Pts',(-57.0470726428986,-106.18572457664,173.034573663757));
#27737=CARTESIAN_POINT('Ctrl Pts',(-58.2525549799674,-105.962930877251,
173.034573714903));
#27738=CARTESIAN_POINT('Ctrl Pts',(-59.4580373170363,-105.740137177862,
173.034573766048));
#27739=CARTESIAN_POINT('Ctrl Pts',(-60.3075312249805,-105.555294223339,
173.898875727171));
#27740=CARTESIAN_POINT('Ctrl Pts',(-61.1570251329247,-105.370451268815,
174.763177688294));
#27741=CARTESIAN_POINT('Ctrl Pts',(-61.1470870191508,-105.277229509582,
175.985485192554));
#27742=CARTESIAN_POINT('Ctrl Pts',(-61.1371489053769,-105.184007750348,
177.207792696815));
#27743=CARTESIAN_POINT('Ctrl Pts',(-60.2677787996762,-105.182407183228,
178.072094585608));
#27744=CARTESIAN_POINT('Ctrl Pts',(-59.3984086939755,-105.180806616108,
178.936396474401));
#27745=CARTESIAN_POINT('Ctrl Pts',(-58.1730502310727,-105.217156786186,
178.936396423256));
#27746=CARTESIAN_POINT('Ctrl Pts',(-56.9476917681698,-105.253506956265,
178.936396372111));
#27747=CARTESIAN_POINT('Ctrl Pts',(-56.0783217343916,-105.251906381477,
178.072094410988));
#27748=CARTESIAN_POINT('Ctrl Pts',(-55.2089517006133,-105.25030580669,177.207792449865));
#27749=CARTESIAN_POINT('Ctrl Pts',(-55.1990136885532,-105.157084036613,
175.985484945604));
#27750=CARTESIAN_POINT('Ctrl Pts',(-55.189075676493,-105.063862266536,174.763177441344));
#27751=CARTESIAN_POINT('Ctrl Pts',(-56.0385696563597,-104.879019304345,
173.89887555255));
#27752=CARTESIAN_POINT('Ctrl Pts',(-56.8880636362264,-104.694176342154,
173.034573663757));
#27753=CARTESIAN_POINT('Ctrl Pts',(-58.0935459732952,-104.471382642765,
173.034573714903));
#27754=CARTESIAN_POINT('Ctrl Pts',(-59.299028310364,-104.248588943376,173.034573766048));
#27755=CARTESIAN_POINT('Ctrl Pts',(-60.1485222183082,-104.063745988853,
173.898875727171));
#27756=CARTESIAN_POINT('Ctrl Pts',(-60.9980161262524,-103.87890303433,174.763177688294));
#27757=CARTESIAN_POINT('Ctrl Pts',(-60.9880780124786,-103.785681275096,
175.985485192554));
#27758=CARTESIAN_POINT('Ctrl Pts',(-60.9781398987047,-103.692459515862,
177.207792696815));
#27759=CARTESIAN_POINT('Ctrl Pts',(-60.108769793004,-103.690858948742,178.072094585608));
#27760=CARTESIAN_POINT('Ctrl Pts',(-59.2393996873033,-103.689258381622,
178.936396474401));
#27761=CARTESIAN_POINT('Ctrl Pts',(-58.0140412244004,-103.725608551701,
178.936396423256));
#27762=CARTESIAN_POINT('Ctrl Pts',(-56.7886827614976,-103.761958721779,
178.936396372111));
#27763=CARTESIAN_POINT('Ctrl Pts',(-55.9193127277193,-103.760358146992,
178.072094410988));
#27764=CARTESIAN_POINT('Ctrl Pts',(-55.0499426939411,-103.758757572204,
177.207792449865));
#27765=CARTESIAN_POINT('Ctrl Pts',(-55.0400046818809,-103.665535802127,
175.985484945604));
#27766=CARTESIAN_POINT('Ctrl Pts',(-55.0300666698208,-103.57231403205,174.763177441344));
#27767=CARTESIAN_POINT('Ctrl Pts',(-55.8795606496874,-103.387471069859,
173.89887555255));
#27768=CARTESIAN_POINT('Ctrl Pts',(-56.7290546295541,-103.202628107669,
173.034573663757));
#27769=CARTESIAN_POINT('Ctrl Pts',(-57.934536966623,-102.97983440828,173.034573714903));
#27770=CARTESIAN_POINT('Ctrl Pts',(-59.1400193036918,-102.757040708891,
173.034573766048));
#27771=CARTESIAN_POINT('Ctrl Pts',(-59.989513211636,-102.572197754367,173.898875727171));
#27772=CARTESIAN_POINT('Ctrl Pts',(-60.8390071195802,-102.387354799844,
174.763177688294));
#27773=CARTESIAN_POINT('Ctrl Pts',(-60.8290690058063,-102.29413304061,175.985485192554));
#27774=CARTESIAN_POINT('Ctrl Pts',(-60.8191308920325,-102.200911281377,
177.207792696815));
#27775=CARTESIAN_POINT('Ctrl Pts',(-59.9497607863318,-102.199310714257,
178.072094585608));
#27776=CARTESIAN_POINT('Ctrl Pts',(-59.0803906806311,-102.197710147137,
178.936396474401));
#27777=CARTESIAN_POINT('Ctrl Pts',(-57.8550322177282,-102.234060317215,
178.936396423256));
#27778=CARTESIAN_POINT('Ctrl Pts',(-56.6296737548253,-102.270410487293,
178.936396372111));
#27779=CARTESIAN_POINT('Ctrl Pts',(-55.7603037210471,-102.268809912506,
178.072094410988));
#27780=CARTESIAN_POINT('Ctrl Pts',(-54.8909336872689,-102.267209337719,
177.207792449865));
#27781=CARTESIAN_POINT('Ctrl Pts',(-54.8809956752087,-102.173987567642,
175.985484945604));
#27782=CARTESIAN_POINT('Ctrl Pts',(-54.8710576631486,-102.080765797565,
174.763177441344));
#27783=CARTESIAN_POINT('Ctrl Pts',(-55.7205516430152,-101.895922835374,
173.89887555255));
#27784=CARTESIAN_POINT('Ctrl Pts',(-56.5700456228819,-101.711079873183,
173.034573663757));
#27785=CARTESIAN_POINT('Ctrl Pts',(-57.7755279599507,-101.488286173794,
173.034573714903));
#27786=CARTESIAN_POINT('Ctrl Pts',(-58.9810102970196,-101.265492474405,
173.034573766048));
#27787=CARTESIAN_POINT('Ctrl Pts',(-59.8305042049638,-101.080649519882,
173.898875727171));
#27788=CARTESIAN_POINT('Ctrl Pts',(-60.679998112908,-100.895806565358,174.763177688294));
#27789=CARTESIAN_POINT('Ctrl Pts',(-60.6700599991341,-100.802584806125,
175.985485192554));
#27790=CARTESIAN_POINT('Ctrl Pts',(-60.6601218853602,-100.709363046891,
177.207792696815));
#27791=CARTESIAN_POINT('Ctrl Pts',(-59.7907517796595,-100.707762479771,
178.072094585608));
#27792=CARTESIAN_POINT('Ctrl Pts',(-58.9213816739588,-100.706161912651,
178.936396474401));
#27793=CARTESIAN_POINT('Ctrl Pts',(-57.696023211056,-100.742512082729,178.936396423256));
#27794=CARTESIAN_POINT('Ctrl Pts',(-56.4706647481531,-100.778862252808,
178.936396372111));
#27795=CARTESIAN_POINT('Ctrl Pts',(-55.6012947143749,-100.77726167802,178.072094410988));
#27796=CARTESIAN_POINT('Ctrl Pts',(-54.7319246805966,-100.775661103233,
177.207792449865));
#27797=CARTESIAN_POINT('Ctrl Pts',(-54.7219866685365,-100.682439333156,
175.985484945604));
#27798=CARTESIAN_POINT('Ctrl Pts',(-54.7120486564763,-100.589217563079,
174.763177441344));
#27799=CARTESIAN_POINT('Ctrl Pts',(-55.561542636343,-100.404374600888,173.89887555255));
#27800=CARTESIAN_POINT('Ctrl Pts',(-56.4110366162097,-100.219531638698,
173.034573663757));
#27801=CARTESIAN_POINT('Ctrl Pts',(-57.6165189532785,-99.9967379393085,
173.034573714903));
#27802=CARTESIAN_POINT('Ctrl Pts',(-58.8220012903473,-99.7739442399195,
173.034573766048));
#27803=CARTESIAN_POINT('Ctrl Pts',(-59.6714951982915,-99.5891012853962,
173.898875727171));
#27804=CARTESIAN_POINT('Ctrl Pts',(-60.5209891062358,-99.4042583308729,
174.763177688294));
#27805=CARTESIAN_POINT('Ctrl Pts',(-60.5110509924619,-99.3110365716392,
175.985485192554));
#27806=CARTESIAN_POINT('Ctrl Pts',(-60.501112878688,-99.2178148124055,177.207792696815));
#27807=CARTESIAN_POINT('Ctrl Pts',(-59.6317427729873,-99.2162142452855,
178.072094585608));
#27808=CARTESIAN_POINT('Ctrl Pts',(-58.7623726672866,-99.2146136781656,
178.936396474401));
#27809=CARTESIAN_POINT('Ctrl Pts',(-57.5370142043838,-99.2509638482439,
178.936396423256));
#27810=CARTESIAN_POINT('Ctrl Pts',(-56.3116557414809,-99.2873140183222,
178.936396372111));
#27811=CARTESIAN_POINT('Ctrl Pts',(-55.4422857077027,-99.2857134435348,
178.072094410988));
#27812=CARTESIAN_POINT('Ctrl Pts',(-54.5729156739244,-99.2841128687474,
177.207792449865));
#27813=CARTESIAN_POINT('Ctrl Pts',(-54.5629776618643,-99.1908910986704,
175.985484945604));
#27814=CARTESIAN_POINT('Ctrl Pts',(-54.5530396498041,-99.0976693285933,
174.763177441344));
#27815=CARTESIAN_POINT('Ctrl Pts',(-55.4025336296708,-98.9128263664026,
173.89887555255));
#27816=CARTESIAN_POINT('Ctrl Pts',(-56.2520276095374,-98.727983404212,173.034573663757));
#27817=CARTESIAN_POINT('Ctrl Pts',(-57.4575099466063,-98.5051897048229,
173.034573714903));
#27818=CARTESIAN_POINT('Ctrl Pts',(-58.6629922836751,-98.2823960054338,
173.034573766048));
#27819=CARTESIAN_POINT('Ctrl Pts',(-59.5124861916193,-98.0975530509106,
173.898875727171));
#27820=CARTESIAN_POINT('Ctrl Pts',(-60.3619800995635,-97.9127100963873,
174.763177688294));
#27821=CARTESIAN_POINT('Ctrl Pts',(-60.3520419857897,-97.8194883371536,
175.985485192554));
#27822=CARTESIAN_POINT('Ctrl Pts',(-60.3421038720158,-97.7262665779199,
177.207792696815));
#27823=CARTESIAN_POINT('Ctrl Pts',(-59.4727337663151,-97.7246660108,178.072094585608));
#27824=CARTESIAN_POINT('Ctrl Pts',(-58.6033636606144,-97.72306544368,178.936396474401));
#27825=CARTESIAN_POINT('Ctrl Pts',(-57.3780051977115,-97.7594156137583,
178.936396423256));
#27826=CARTESIAN_POINT('Ctrl Pts',(-56.1526467348087,-97.7957657838366,
178.936396372111));
#27827=CARTESIAN_POINT('Ctrl Pts',(-55.2832767010304,-97.7941652090492,
178.072094410988));
#27828=CARTESIAN_POINT('Ctrl Pts',(-56.1707931031902,-113.117197303651,
178.813912075476));
#27829=CARTESIAN_POINT('Ctrl Pts',(-54.9958834532485,-113.148169293224,
177.6423391512));
#27830=CARTESIAN_POINT('Ctrl Pts',(-54.9859454592686,-113.05494752122,175.985484901707));
#27831=CARTESIAN_POINT('Ctrl Pts',(-54.9760074652888,-112.961725749215,
174.328630652215));
#27832=CARTESIAN_POINT('Ctrl Pts',(-56.1310410868884,-112.744310219938,
173.157057825983));
#27833=CARTESIAN_POINT('Ctrl Pts',(-57.286074708488,-112.52689469066,171.985484999752));
#27834=CARTESIAN_POINT('Ctrl Pts',(-58.9236553326579,-112.258036427063,
171.985485069079));
#27835=CARTESIAN_POINT('Ctrl Pts',(-60.5612359568277,-111.989178163466,
171.985485138407));
#27836=CARTESIAN_POINT('Ctrl Pts',(-61.7162694809355,-111.771762644582,
173.157058062683));
#27837=CARTESIAN_POINT('Ctrl Pts',(-62.8713030050432,-111.554347125698,
174.328630986959));
#27838=CARTESIAN_POINT('Ctrl Pts',(-62.861364873189,-111.461125368392,175.985485236451));
#27839=CARTESIAN_POINT('Ctrl Pts',(-62.8514267413349,-111.367903611086,
177.642339485944));
#27840=CARTESIAN_POINT('Ctrl Pts',(-61.6765169939012,-111.398875611052,
178.813912312176));
#27841=CARTESIAN_POINT('Ctrl Pts',(-60.5016072464676,-111.429847611019,
179.985485138407));
#27842=CARTESIAN_POINT('Ctrl Pts',(-58.8441504964637,-111.512262345305,
179.985485069079));
#27843=CARTESIAN_POINT('Ctrl Pts',(-57.1866937464598,-111.594677079592,
179.985484999752));
#27844=CARTESIAN_POINT('Ctrl Pts',(-56.011784096518,-111.625649069165,178.813912075476));
#27845=CARTESIAN_POINT('Ctrl Pts',(-54.8368744465762,-111.656621058739,
177.6423391512));
#27846=CARTESIAN_POINT('Ctrl Pts',(-54.8269364525964,-111.563399286734,
175.985484901707));
#27847=CARTESIAN_POINT('Ctrl Pts',(-54.8169984586165,-111.47017751473,174.328630652215));
#27848=CARTESIAN_POINT('Ctrl Pts',(-55.9720320802161,-111.252761985452,
173.157057825983));
#27849=CARTESIAN_POINT('Ctrl Pts',(-57.1270657018158,-111.035346456175,
171.985484999752));
#27850=CARTESIAN_POINT('Ctrl Pts',(-58.7646463259856,-110.766488192578,
171.985485069079));
#27851=CARTESIAN_POINT('Ctrl Pts',(-60.4022269501555,-110.497629928981,
171.985485138407));
#27852=CARTESIAN_POINT('Ctrl Pts',(-61.5572604742632,-110.280214410097,
173.157058062683));
#27853=CARTESIAN_POINT('Ctrl Pts',(-62.712293998371,-110.062798891212,174.328630986959));
#27854=CARTESIAN_POINT('Ctrl Pts',(-62.7023558665168,-109.969577133906,
175.985485236451));
#27855=CARTESIAN_POINT('Ctrl Pts',(-62.6924177346626,-109.8763553766,177.642339485944));
#27856=CARTESIAN_POINT('Ctrl Pts',(-61.517507987229,-109.907327376567,178.813912312176));
#27857=CARTESIAN_POINT('Ctrl Pts',(-60.3425982397954,-109.938299376534,
179.985485138407));
#27858=CARTESIAN_POINT('Ctrl Pts',(-58.6851414897915,-110.02071411082,179.985485069079));
#27859=CARTESIAN_POINT('Ctrl Pts',(-57.0276847397876,-110.103128845106,
179.985484999752));
#27860=CARTESIAN_POINT('Ctrl Pts',(-55.8527750898458,-110.13410083468,178.813912075476));
#27861=CARTESIAN_POINT('Ctrl Pts',(-54.677865439904,-110.165072824253,177.6423391512));
#27862=CARTESIAN_POINT('Ctrl Pts',(-54.6679274459242,-110.071851052249,
175.985484901707));
#27863=CARTESIAN_POINT('Ctrl Pts',(-54.6579894519443,-109.978629280244,
174.328630652215));
#27864=CARTESIAN_POINT('Ctrl Pts',(-55.8130230735439,-109.761213750967,
173.157057825983));
#27865=CARTESIAN_POINT('Ctrl Pts',(-56.9680566951435,-109.543798221689,
171.985484999752));
#27866=CARTESIAN_POINT('Ctrl Pts',(-58.6056373193134,-109.274939958092,
171.985485069079));
#27867=CARTESIAN_POINT('Ctrl Pts',(-60.2432179434833,-109.006081694495,
171.985485138407));
#27868=CARTESIAN_POINT('Ctrl Pts',(-61.398251467591,-108.788666175611,173.157058062683));
#27869=CARTESIAN_POINT('Ctrl Pts',(-62.5532849916988,-108.571250656727,
174.328630986959));
#27870=CARTESIAN_POINT('Ctrl Pts',(-62.5433468598446,-108.478028899421,
175.985485236451));
#27871=CARTESIAN_POINT('Ctrl Pts',(-62.5334087279904,-108.384807142114,
177.642339485944));
#27872=CARTESIAN_POINT('Ctrl Pts',(-61.3584989805568,-108.415779142081,
178.813912312176));
#27873=CARTESIAN_POINT('Ctrl Pts',(-60.1835892331231,-108.446751142048,
179.985485138407));
#27874=CARTESIAN_POINT('Ctrl Pts',(-58.5261324831192,-108.529165876334,
179.985485069079));
#27875=CARTESIAN_POINT('Ctrl Pts',(-56.8686757331153,-108.611580610621,
179.985484999752));
#27876=CARTESIAN_POINT('Ctrl Pts',(-55.6937660831736,-108.642552600194,
178.813912075476));
#27877=CARTESIAN_POINT('Ctrl Pts',(-54.5188564332318,-108.673524589768,
177.6423391512));
#27878=CARTESIAN_POINT('Ctrl Pts',(-54.5089184392519,-108.580302817763,
175.985484901707));
#27879=CARTESIAN_POINT('Ctrl Pts',(-54.4989804452721,-108.487081045759,
174.328630652215));
#27880=CARTESIAN_POINT('Ctrl Pts',(-55.6540140668717,-108.269665516481,
173.157057825983));
#27881=CARTESIAN_POINT('Ctrl Pts',(-56.8090476884713,-108.052249987204,
171.985484999752));
#27882=CARTESIAN_POINT('Ctrl Pts',(-58.4466283126412,-107.783391723607,
171.985485069079));
#27883=CARTESIAN_POINT('Ctrl Pts',(-60.084208936811,-107.51453346001,171.985485138407));
#27884=CARTESIAN_POINT('Ctrl Pts',(-61.2392424609188,-107.297117941125,
173.157058062683));
#27885=CARTESIAN_POINT('Ctrl Pts',(-62.3942759850265,-107.079702422241,
174.328630986959));
#27886=CARTESIAN_POINT('Ctrl Pts',(-62.3843378531723,-106.986480664935,
175.985485236451));
#27887=CARTESIAN_POINT('Ctrl Pts',(-62.3743997213182,-106.893258907629,
177.642339485944));
#27888=CARTESIAN_POINT('Ctrl Pts',(-61.1994899738845,-106.924230907596,
178.813912312176));
#27889=CARTESIAN_POINT('Ctrl Pts',(-60.0245802264509,-106.955202907562,
179.985485138407));
#27890=CARTESIAN_POINT('Ctrl Pts',(-58.367123476447,-107.037617641849,179.985485069079));
#27891=CARTESIAN_POINT('Ctrl Pts',(-56.7096667264431,-107.120032376135,
179.985484999752));
#27892=CARTESIAN_POINT('Ctrl Pts',(-55.5347570765013,-107.151004365708,
178.813912075476));
#27893=CARTESIAN_POINT('Ctrl Pts',(-54.3598474265596,-107.181976355282,
177.6423391512));
#27894=CARTESIAN_POINT('Ctrl Pts',(-54.3499094325797,-107.088754583277,
175.985484901707));
#27895=CARTESIAN_POINT('Ctrl Pts',(-54.3399714385998,-106.995532811273,
174.328630652215));
#27896=CARTESIAN_POINT('Ctrl Pts',(-55.4950050601995,-106.778117281995,
173.157057825983));
#27897=CARTESIAN_POINT('Ctrl Pts',(-56.6500386817991,-106.560701752718,
171.985484999752));
#27898=CARTESIAN_POINT('Ctrl Pts',(-58.2876193059689,-106.291843489121,
171.985485069079));
#27899=CARTESIAN_POINT('Ctrl Pts',(-59.9251999301388,-106.022985225524,
171.985485138407));
#27900=CARTESIAN_POINT('Ctrl Pts',(-61.0802334542465,-105.80556970664,173.157058062683));
#27901=CARTESIAN_POINT('Ctrl Pts',(-62.2352669783543,-105.588154187756,
174.328630986959));
#27902=CARTESIAN_POINT('Ctrl Pts',(-62.2253288465001,-105.494932430449,
175.985485236451));
#27903=CARTESIAN_POINT('Ctrl Pts',(-62.2153907146459,-105.401710673143,
177.642339485944));
#27904=CARTESIAN_POINT('Ctrl Pts',(-61.0404809672123,-105.43268267311,178.813912312176));
#27905=CARTESIAN_POINT('Ctrl Pts',(-59.8655712197787,-105.463654673077,
179.985485138407));
#27906=CARTESIAN_POINT('Ctrl Pts',(-58.2081144697748,-105.546069407363,
179.985485069079));
#27907=CARTESIAN_POINT('Ctrl Pts',(-56.5506577197709,-105.628484141649,
179.985484999752));
#27908=CARTESIAN_POINT('Ctrl Pts',(-55.3757480698291,-105.659456131223,
178.813912075476));
#27909=CARTESIAN_POINT('Ctrl Pts',(-54.2008384198873,-105.690428120796,
177.6423391512));
#27910=CARTESIAN_POINT('Ctrl Pts',(-54.1909004259075,-105.597206348792,
175.985484901707));
#27911=CARTESIAN_POINT('Ctrl Pts',(-54.1809624319276,-105.503984576787,
174.328630652215));
#27912=CARTESIAN_POINT('Ctrl Pts',(-55.3359960535272,-105.28656904751,173.157057825983));
#27913=CARTESIAN_POINT('Ctrl Pts',(-56.4910296751268,-105.069153518232,
171.985484999752));
#27914=CARTESIAN_POINT('Ctrl Pts',(-58.1286102992967,-104.800295254635,
171.985485069079));
#27915=CARTESIAN_POINT('Ctrl Pts',(-59.7661909234666,-104.531436991038,
171.985485138407));
#27916=CARTESIAN_POINT('Ctrl Pts',(-60.9212244475743,-104.314021472154,
173.157058062683));
#27917=CARTESIAN_POINT('Ctrl Pts',(-62.0762579716821,-104.09660595327,174.328630986959));
#27918=CARTESIAN_POINT('Ctrl Pts',(-62.0663198398279,-104.003384195964,
175.985485236451));
#27919=CARTESIAN_POINT('Ctrl Pts',(-62.0563817079737,-103.910162438658,
177.642339485944));
#27920=CARTESIAN_POINT('Ctrl Pts',(-60.8814719605401,-103.941134438624,
178.813912312176));
#27921=CARTESIAN_POINT('Ctrl Pts',(-59.7065622131064,-103.972106438591,
179.985485138407));
#27922=CARTESIAN_POINT('Ctrl Pts',(-58.0491054631025,-104.054521172878,
179.985485069079));
#27923=CARTESIAN_POINT('Ctrl Pts',(-56.3916487130987,-104.136935907164,
179.985484999752));
#27924=CARTESIAN_POINT('Ctrl Pts',(-55.2167390631569,-104.167907896737,
178.813912075476));
#27925=CARTESIAN_POINT('Ctrl Pts',(-54.0418294132151,-104.198879886311,
177.6423391512));
#27926=CARTESIAN_POINT('Ctrl Pts',(-54.0318914192353,-104.105658114306,
175.985484901707));
#27927=CARTESIAN_POINT('Ctrl Pts',(-54.0219534252554,-104.012436342302,
174.328630652215));
#27928=CARTESIAN_POINT('Ctrl Pts',(-55.176987046855,-103.795020813024,173.157057825983));
#27929=CARTESIAN_POINT('Ctrl Pts',(-56.3320206684546,-103.577605283747,
171.985484999752));
#27930=CARTESIAN_POINT('Ctrl Pts',(-57.9696012926245,-103.30874702015,171.985485069079));
#27931=CARTESIAN_POINT('Ctrl Pts',(-59.6071819167943,-103.039888756553,
171.985485138407));
#27932=CARTESIAN_POINT('Ctrl Pts',(-60.7622154409021,-102.822473237669,
173.157058062683));
#27933=CARTESIAN_POINT('Ctrl Pts',(-61.9172489650099,-102.605057718784,
174.328630986959));
#27934=CARTESIAN_POINT('Ctrl Pts',(-61.9073108331557,-102.511835961478,
175.985485236451));
#27935=CARTESIAN_POINT('Ctrl Pts',(-61.8973727013015,-102.418614204172,
177.642339485944));
#27936=CARTESIAN_POINT('Ctrl Pts',(-60.7224629538678,-102.449586204139,
178.813912312176));
#27937=CARTESIAN_POINT('Ctrl Pts',(-59.5475532064342,-102.480558204106,
179.985485138407));
#27938=CARTESIAN_POINT('Ctrl Pts',(-57.8900964564303,-102.562972938392,
179.985485069079));
#27939=CARTESIAN_POINT('Ctrl Pts',(-56.2326397064264,-102.645387672678,
179.985484999752));
#27940=CARTESIAN_POINT('Ctrl Pts',(-55.0577300564847,-102.676359662252,
178.813912075476));
#27941=CARTESIAN_POINT('Ctrl Pts',(-53.8828204065429,-102.707331651825,
177.6423391512));
#27942=CARTESIAN_POINT('Ctrl Pts',(-53.872882412563,-102.614109879821,175.985484901707));
#27943=CARTESIAN_POINT('Ctrl Pts',(-53.8629444185832,-102.520888107816,
174.328630652215));
#27944=CARTESIAN_POINT('Ctrl Pts',(-55.0179780401828,-102.303472578539,
173.157057825983));
#27945=CARTESIAN_POINT('Ctrl Pts',(-56.1730116617824,-102.086057049261,
171.985484999752));
#27946=CARTESIAN_POINT('Ctrl Pts',(-57.8105922859523,-101.817198785664,
171.985485069079));
#27947=CARTESIAN_POINT('Ctrl Pts',(-59.4481729101221,-101.548340522067,
171.985485138407));
#27948=CARTESIAN_POINT('Ctrl Pts',(-60.6032064342299,-101.330925003183,
173.157058062683));
#27949=CARTESIAN_POINT('Ctrl Pts',(-61.7582399583376,-101.113509484299,
174.328630986959));
#27950=CARTESIAN_POINT('Ctrl Pts',(-61.7483018264834,-101.020287726993,
175.985485236451));
#27951=CARTESIAN_POINT('Ctrl Pts',(-61.7383636946293,-100.927065969686,
177.642339485944));
#27952=CARTESIAN_POINT('Ctrl Pts',(-60.5634539471956,-100.958037969653,
178.813912312176));
#27953=CARTESIAN_POINT('Ctrl Pts',(-59.388544199762,-100.98900996962,179.985485138407));
#27954=CARTESIAN_POINT('Ctrl Pts',(-57.7310874497581,-101.071424703906,
179.985485069079));
#27955=CARTESIAN_POINT('Ctrl Pts',(-56.0736306997542,-101.153839438193,
179.985484999752));
#27956=CARTESIAN_POINT('Ctrl Pts',(-54.8987210498124,-101.184811427766,
178.813912075476));
#27957=CARTESIAN_POINT('Ctrl Pts',(-53.7238113998707,-101.21578341734,177.6423391512));
#27958=CARTESIAN_POINT('Ctrl Pts',(-53.7138734058908,-101.122561645335,
175.985484901707));
#27959=CARTESIAN_POINT('Ctrl Pts',(-53.7039354119109,-101.029339873331,
174.328630652215));
#27960=CARTESIAN_POINT('Ctrl Pts',(-54.8589690335105,-100.811924344053,
173.157057825983));
#27961=CARTESIAN_POINT('Ctrl Pts',(-56.0140026551102,-100.594508814776,
171.985484999752));
#27962=CARTESIAN_POINT('Ctrl Pts',(-57.65158327928,-100.325650551179,171.985485069079));
#27963=CARTESIAN_POINT('Ctrl Pts',(-59.2891639034499,-100.056792287582,
171.985485138407));
#27964=CARTESIAN_POINT('Ctrl Pts',(-60.4441974275576,-99.8393767686974,
173.157058062683));
#27965=CARTESIAN_POINT('Ctrl Pts',(-61.5992309516654,-99.6219612498133,
174.328630986959));
#27966=CARTESIAN_POINT('Ctrl Pts',(-61.5892928198112,-99.528739492507,175.985485236451));
#27967=CARTESIAN_POINT('Ctrl Pts',(-61.579354687957,-99.4355177352008,177.642339485944));
#27968=CARTESIAN_POINT('Ctrl Pts',(-60.4044449405234,-99.4664897351676,
178.813912312176));
#27969=CARTESIAN_POINT('Ctrl Pts',(-59.2295351930898,-99.4974617351344,
179.985485138407));
#27970=CARTESIAN_POINT('Ctrl Pts',(-57.5720784430859,-99.5798764694207,
179.985485069079));
#27971=CARTESIAN_POINT('Ctrl Pts',(-55.914621693082,-99.662291203707,179.985484999752));
#27972=CARTESIAN_POINT('Ctrl Pts',(-54.7397120431402,-99.6932631932805,
178.813912075476));
#27973=CARTESIAN_POINT('Ctrl Pts',(-53.5648023931984,-99.724235182854,177.6423391512));
#27974=CARTESIAN_POINT('Ctrl Pts',(-53.5548643992186,-99.6310134108495,
175.985484901707));
#27975=CARTESIAN_POINT('Ctrl Pts',(-53.5449264052387,-99.5377916388449,
174.328630652215));
#27976=CARTESIAN_POINT('Ctrl Pts',(-54.6999600268383,-99.3203761095675,
173.157057825983));
#27977=CARTESIAN_POINT('Ctrl Pts',(-55.8549936484379,-99.10296058029,171.985484999752));
#27978=CARTESIAN_POINT('Ctrl Pts',(-57.4925742726078,-98.834102316693,171.985485069079));
#27979=CARTESIAN_POINT('Ctrl Pts',(-59.1301548967777,-98.565244053096,171.985485138407));
#27980=CARTESIAN_POINT('Ctrl Pts',(-60.2851884208854,-98.3478285342118,
173.157058062683));
#27981=CARTESIAN_POINT('Ctrl Pts',(-61.4402219449932,-98.1304130153276,
174.328630986959));
#27982=CARTESIAN_POINT('Ctrl Pts',(-61.430283813139,-98.0371912580215,175.985485236451));
#27983=CARTESIAN_POINT('Ctrl Pts',(-61.4203456812848,-97.9439695007152,
177.642339485944));
#27984=CARTESIAN_POINT('Ctrl Pts',(-60.2454359338512,-97.974941500682,178.813912312176));
#27985=CARTESIAN_POINT('Ctrl Pts',(-59.0705261864175,-98.0059135006488,
179.985485138407));
#27986=CARTESIAN_POINT('Ctrl Pts',(-57.4130694364136,-98.0883282349351,
179.985485069079));
#27987=CARTESIAN_POINT('Ctrl Pts',(-55.7556126864097,-98.1707429692214,
179.985484999752));
#27988=CARTESIAN_POINT('Ctrl Pts',(-54.580703036468,-98.2017149587949,178.813912075476));
#27989=CARTESIAN_POINT('Ctrl Pts',(-61.4946055979174,-106.918389721436,
178.485485069079));
#27990=CARTESIAN_POINT('Ctrl Pts',(-61.3560333935607,-106.920104239314,
178.657813499464));
#27991=CARTESIAN_POINT('Ctrl Pts',(-61.1994899738845,-106.924230907596,
178.813912312176));
#27992=CARTESIAN_POINT('Ctrl Pts',(-60.0245802264509,-106.955202907562,
179.985485138407));
#27993=CARTESIAN_POINT('Ctrl Pts',(-58.367123476447,-107.037617641849,179.985485069079));
#27994=CARTESIAN_POINT('Ctrl Pts',(-56.7096667264431,-107.120032376135,
179.985484999752));
#27995=CARTESIAN_POINT('Ctrl Pts',(-55.5347570765013,-107.151004365708,
178.813912075476));
#27996=CARTESIAN_POINT('Ctrl Pts',(-54.3598474265596,-107.181976355282,
177.6423391512));
#27997=CARTESIAN_POINT('Ctrl Pts',(-54.3499094325797,-107.088754583277,
175.985484901707));
#27998=CARTESIAN_POINT('Ctrl Pts',(-54.3399714385999,-106.995532811273,
174.328630652215));
#27999=CARTESIAN_POINT('Ctrl Pts',(-55.4950050601995,-106.778117281995,
173.157057825983));
#28000=CARTESIAN_POINT('Ctrl Pts',(-56.6500386817991,-106.560701752718,
171.985484999752));
#28001=CARTESIAN_POINT('Ctrl Pts',(-58.2876193059689,-106.291843489121,
171.985485069079));
#28002=CARTESIAN_POINT('Ctrl Pts',(-59.9251999301388,-106.022985225524,
171.985485138407));
#28003=CARTESIAN_POINT('Ctrl Pts',(-61.0802334542465,-105.80556970664,173.157058062683));
#28004=CARTESIAN_POINT('Ctrl Pts',(-61.2341284751997,-105.776601572697,
173.313156769748));
#28005=CARTESIAN_POINT('Ctrl Pts',(-61.3699476791705,-105.749064143515,
173.485485069079));
#28006=CARTESIAN_POINT('Ctrl Pts',(-56.1707931031902,-113.117197303651,
178.813912075476));
#28007=CARTESIAN_POINT('Ctrl Pts',(-54.9958834532485,-113.148169293224,
177.6423391512));
#28008=CARTESIAN_POINT('Ctrl Pts',(-54.9859454592686,-113.05494752122,175.985484901707));
#28009=CARTESIAN_POINT('Ctrl Pts',(-54.9760074652888,-112.961725749215,
174.328630652215));
#28010=CARTESIAN_POINT('Ctrl Pts',(-56.1310410868884,-112.744310219938,
173.157057825983));
#28011=CARTESIAN_POINT('Ctrl Pts',(-57.286074708488,-112.52689469066,171.985484999752));
#28012=CARTESIAN_POINT('Ctrl Pts',(-58.9236553326578,-112.258036427063,
171.985485069079));
#28013=CARTESIAN_POINT('Ctrl Pts',(-60.5612359568277,-111.989178163466,
171.985485138407));
#28014=CARTESIAN_POINT('Ctrl Pts',(-61.7162694809355,-111.771762644582,
173.157058062683));
#28015=CARTESIAN_POINT('Ctrl Pts',(-62.8713030050432,-111.554347125698,
174.328630986959));
#28016=CARTESIAN_POINT('Ctrl Pts',(-62.861364873189,-111.461125368392,175.985485236451));
#28017=CARTESIAN_POINT('Ctrl Pts',(-62.8514267413349,-111.367903611086,
177.642339485944));
#28018=CARTESIAN_POINT('Ctrl Pts',(-61.6765169939012,-111.398875611052,
178.813912312176));
#28019=CARTESIAN_POINT('Ctrl Pts',(-60.5016072464676,-111.429847611019,
179.985485138407));
#28020=CARTESIAN_POINT('Ctrl Pts',(-58.8441504964637,-111.512262345305,
179.985485069079));
#28021=CARTESIAN_POINT('Ctrl Pts',(-57.1866937464598,-111.594677079592,
179.985484999752));
#28022=CARTESIAN_POINT('Ctrl Pts',(-56.011784096518,-111.625649069165,178.813912075476));
#28023=CARTESIAN_POINT('Ctrl Pts',(-54.8368744465763,-111.656621058739,
177.6423391512));
#28024=CARTESIAN_POINT('Ctrl Pts',(-54.8269364525964,-111.563399286734,
175.985484901707));
#28025=CARTESIAN_POINT('Ctrl Pts',(-54.8169984586165,-111.47017751473,174.328630652215));
#28026=CARTESIAN_POINT('Ctrl Pts',(-55.9720320802161,-111.252761985452,
173.157057825983));
#28027=CARTESIAN_POINT('Ctrl Pts',(-57.1270657018158,-111.035346456175,
171.985484999752));
#28028=CARTESIAN_POINT('Ctrl Pts',(-58.7646463259856,-110.766488192578,
171.985485069079));
#28029=CARTESIAN_POINT('Ctrl Pts',(-60.4022269501555,-110.497629928981,
171.985485138407));
#28030=CARTESIAN_POINT('Ctrl Pts',(-61.5572604742632,-110.280214410097,
173.157058062683));
#28031=CARTESIAN_POINT('Ctrl Pts',(-62.712293998371,-110.062798891212,174.328630986959));
#28032=CARTESIAN_POINT('Ctrl Pts',(-62.7023558665168,-109.969577133906,
175.985485236451));
#28033=CARTESIAN_POINT('Ctrl Pts',(-62.6924177346626,-109.8763553766,177.642339485944));
#28034=CARTESIAN_POINT('Ctrl Pts',(-61.517507987229,-109.907327376567,178.813912312176));
#28035=CARTESIAN_POINT('Ctrl Pts',(-60.3425982397954,-109.938299376534,
179.985485138407));
#28036=CARTESIAN_POINT('Ctrl Pts',(-58.6851414897915,-110.02071411082,179.985485069079));
#28037=CARTESIAN_POINT('Ctrl Pts',(-57.0276847397876,-110.103128845106,
179.985484999752));
#28038=CARTESIAN_POINT('Ctrl Pts',(-55.8527750898458,-110.13410083468,178.813912075476));
#28039=CARTESIAN_POINT('Ctrl Pts',(-54.677865439904,-110.165072824253,177.6423391512));
#28040=CARTESIAN_POINT('Ctrl Pts',(-54.6679274459242,-110.071851052249,
175.985484901707));
#28041=CARTESIAN_POINT('Ctrl Pts',(-54.6579894519443,-109.978629280244,
174.328630652215));
#28042=CARTESIAN_POINT('Ctrl Pts',(-55.8130230735439,-109.761213750967,
173.157057825983));
#28043=CARTESIAN_POINT('Ctrl Pts',(-56.9680566951435,-109.543798221689,
171.985484999752));
#28044=CARTESIAN_POINT('Ctrl Pts',(-58.6056373193134,-109.274939958092,
171.985485069079));
#28045=CARTESIAN_POINT('Ctrl Pts',(-60.2432179434833,-109.006081694495,
171.985485138407));
#28046=CARTESIAN_POINT('Ctrl Pts',(-61.398251467591,-108.788666175611,173.157058062683));
#28047=CARTESIAN_POINT('Ctrl Pts',(-62.5532849916988,-108.571250656727,
174.328630986959));
#28048=CARTESIAN_POINT('Ctrl Pts',(-62.5433468598446,-108.478028899421,
175.985485236451));
#28049=CARTESIAN_POINT('Ctrl Pts',(-62.5334087279904,-108.384807142114,
177.642339485944));
#28050=CARTESIAN_POINT('Ctrl Pts',(-61.3584989805568,-108.415779142081,
178.813912312176));
#28051=CARTESIAN_POINT('Ctrl Pts',(-60.1835892331231,-108.446751142048,
179.985485138407));
#28052=CARTESIAN_POINT('Ctrl Pts',(-58.5261324831192,-108.529165876334,
179.985485069079));
#28053=CARTESIAN_POINT('Ctrl Pts',(-56.8686757331153,-108.611580610621,
179.985484999752));
#28054=CARTESIAN_POINT('Ctrl Pts',(-55.6937660831736,-108.642552600194,
178.813912075476));
#28055=CARTESIAN_POINT('Ctrl Pts',(-54.5188564332318,-108.673524589768,
177.6423391512));
#28056=CARTESIAN_POINT('Ctrl Pts',(-54.5089184392519,-108.580302817763,
175.985484901707));
#28057=CARTESIAN_POINT('Ctrl Pts',(-54.4989804452721,-108.487081045759,
174.328630652215));
#28058=CARTESIAN_POINT('Ctrl Pts',(-55.6540140668717,-108.269665516481,
173.157057825983));
#28059=CARTESIAN_POINT('Ctrl Pts',(-56.8090476884713,-108.052249987204,
171.985484999752));
#28060=CARTESIAN_POINT('Ctrl Pts',(-58.4466283126412,-107.783391723607,
171.985485069079));
#28061=CARTESIAN_POINT('Ctrl Pts',(-60.084208936811,-107.51453346001,171.985485138407));
#28062=CARTESIAN_POINT('Ctrl Pts',(-61.2392424609188,-107.297117941125,
173.157058062683));
#28063=CARTESIAN_POINT('Ctrl Pts',(-62.3942759850265,-107.079702422241,
174.328630986959));
#28064=CARTESIAN_POINT('Ctrl Pts',(-62.3843378531723,-106.986480664935,
175.985485236451));
#28065=CARTESIAN_POINT('Ctrl Pts',(-62.3743997213182,-106.893258907629,
177.642339485944));
#28066=CARTESIAN_POINT('Ctrl Pts',(-61.1994899738845,-106.924230907596,
178.813912312176));
#28067=CARTESIAN_POINT('Ctrl Pts',(-60.0245802264509,-106.955202907562,
179.985485138407));
#28068=CARTESIAN_POINT('Ctrl Pts',(-58.367123476447,-107.037617641849,179.985485069079));
#28069=CARTESIAN_POINT('Ctrl Pts',(-56.7096667264431,-107.120032376135,
179.985484999752));
#28070=CARTESIAN_POINT('Ctrl Pts',(-55.5347570765013,-107.151004365708,
178.813912075476));
#28071=CARTESIAN_POINT('Ctrl Pts',(-54.3598474265596,-107.181976355282,
177.6423391512));
#28072=CARTESIAN_POINT('Ctrl Pts',(-54.3499094325797,-107.088754583277,
175.985484901707));
#28073=CARTESIAN_POINT('Ctrl Pts',(-54.3399714385998,-106.995532811273,
174.328630652215));
#28074=CARTESIAN_POINT('Ctrl Pts',(-55.4950050601995,-106.778117281995,
173.157057825983));
#28075=CARTESIAN_POINT('Ctrl Pts',(-56.6500386817991,-106.560701752718,
171.985484999752));
#28076=CARTESIAN_POINT('Ctrl Pts',(-58.2876193059689,-106.291843489121,
171.985485069079));
#28077=CARTESIAN_POINT('Ctrl Pts',(-59.9251999301388,-106.022985225524,
171.985485138407));
#28078=CARTESIAN_POINT('Ctrl Pts',(-61.0802334542465,-105.80556970664,173.157058062683));
#28079=CARTESIAN_POINT('Ctrl Pts',(-62.2352669783543,-105.588154187756,
174.328630986959));
#28080=CARTESIAN_POINT('Ctrl Pts',(-62.2253288465001,-105.494932430449,
175.985485236451));
#28081=CARTESIAN_POINT('Ctrl Pts',(-62.2153907146459,-105.401710673143,
177.642339485944));
#28082=CARTESIAN_POINT('Ctrl Pts',(-61.0404809672123,-105.43268267311,178.813912312176));
#28083=CARTESIAN_POINT('Ctrl Pts',(-59.8655712197787,-105.463654673077,
179.985485138407));
#28084=CARTESIAN_POINT('Ctrl Pts',(-58.2081144697748,-105.546069407363,
179.985485069079));
#28085=CARTESIAN_POINT('Ctrl Pts',(-56.5506577197709,-105.628484141649,
179.985484999752));
#28086=CARTESIAN_POINT('Ctrl Pts',(-55.3757480698291,-105.659456131223,
178.813912075476));
#28087=CARTESIAN_POINT('Ctrl Pts',(-54.2008384198873,-105.690428120796,
177.6423391512));
#28088=CARTESIAN_POINT('Ctrl Pts',(-54.1909004259075,-105.597206348792,
175.985484901707));
#28089=CARTESIAN_POINT('Ctrl Pts',(-54.1809624319276,-105.503984576787,
174.328630652215));
#28090=CARTESIAN_POINT('Ctrl Pts',(-55.3359960535272,-105.28656904751,173.157057825983));
#28091=CARTESIAN_POINT('Ctrl Pts',(-56.4910296751268,-105.069153518232,
171.985484999752));
#28092=CARTESIAN_POINT('Ctrl Pts',(-58.1286102992967,-104.800295254635,
171.985485069079));
#28093=CARTESIAN_POINT('Ctrl Pts',(-59.7661909234666,-104.531436991038,
171.985485138407));
#28094=CARTESIAN_POINT('Ctrl Pts',(-60.9212244475743,-104.314021472154,
173.157058062683));
#28095=CARTESIAN_POINT('Ctrl Pts',(-62.0762579716821,-104.09660595327,174.328630986959));
#28096=CARTESIAN_POINT('Ctrl Pts',(-62.0663198398279,-104.003384195964,
175.985485236451));
#28097=CARTESIAN_POINT('Ctrl Pts',(-62.0563817079737,-103.910162438658,
177.642339485944));
#28098=CARTESIAN_POINT('Ctrl Pts',(-60.8814719605401,-103.941134438624,
178.813912312176));
#28099=CARTESIAN_POINT('Ctrl Pts',(-59.7065622131064,-103.972106438591,
179.985485138407));
#28100=CARTESIAN_POINT('Ctrl Pts',(-58.0491054631025,-104.054521172878,
179.985485069079));
#28101=CARTESIAN_POINT('Ctrl Pts',(-56.3916487130987,-104.136935907164,
179.985484999752));
#28102=CARTESIAN_POINT('Ctrl Pts',(-55.2167390631569,-104.167907896737,
178.813912075476));
#28103=CARTESIAN_POINT('Ctrl Pts',(-54.0418294132151,-104.198879886311,
177.6423391512));
#28104=CARTESIAN_POINT('Ctrl Pts',(-54.0318914192353,-104.105658114306,
175.985484901707));
#28105=CARTESIAN_POINT('Ctrl Pts',(-54.0219534252554,-104.012436342302,
174.328630652215));
#28106=CARTESIAN_POINT('Ctrl Pts',(-55.176987046855,-103.795020813024,173.157057825983));
#28107=CARTESIAN_POINT('Ctrl Pts',(-56.3320206684546,-103.577605283747,
171.985484999752));
#28108=CARTESIAN_POINT('Ctrl Pts',(-57.9696012926245,-103.30874702015,171.985485069079));
#28109=CARTESIAN_POINT('Ctrl Pts',(-59.6071819167943,-103.039888756553,
171.985485138407));
#28110=CARTESIAN_POINT('Ctrl Pts',(-60.7622154409021,-102.822473237669,
173.157058062683));
#28111=CARTESIAN_POINT('Ctrl Pts',(-61.9172489650099,-102.605057718784,
174.328630986959));
#28112=CARTESIAN_POINT('Ctrl Pts',(-61.9073108331557,-102.511835961478,
175.985485236451));
#28113=CARTESIAN_POINT('Ctrl Pts',(-61.8973727013015,-102.418614204172,
177.642339485944));
#28114=CARTESIAN_POINT('Ctrl Pts',(-60.7224629538678,-102.449586204139,
178.813912312176));
#28115=CARTESIAN_POINT('Ctrl Pts',(-59.5475532064342,-102.480558204106,
179.985485138407));
#28116=CARTESIAN_POINT('Ctrl Pts',(-57.8900964564303,-102.562972938392,
179.985485069079));
#28117=CARTESIAN_POINT('Ctrl Pts',(-56.2326397064264,-102.645387672678,
179.985484999752));
#28118=CARTESIAN_POINT('Ctrl Pts',(-55.0577300564847,-102.676359662252,
178.813912075476));
#28119=CARTESIAN_POINT('Ctrl Pts',(-53.8828204065429,-102.707331651825,
177.6423391512));
#28120=CARTESIAN_POINT('Ctrl Pts',(-53.872882412563,-102.614109879821,175.985484901707));
#28121=CARTESIAN_POINT('Ctrl Pts',(-53.8629444185832,-102.520888107816,
174.328630652215));
#28122=CARTESIAN_POINT('Ctrl Pts',(-55.0179780401828,-102.303472578539,
173.157057825983));
#28123=CARTESIAN_POINT('Ctrl Pts',(-56.1730116617824,-102.086057049261,
171.985484999752));
#28124=CARTESIAN_POINT('Ctrl Pts',(-57.8105922859523,-101.817198785664,
171.985485069079));
#28125=CARTESIAN_POINT('Ctrl Pts',(-59.4481729101221,-101.548340522067,
171.985485138407));
#28126=CARTESIAN_POINT('Ctrl Pts',(-60.6032064342299,-101.330925003183,
173.157058062683));
#28127=CARTESIAN_POINT('Ctrl Pts',(-61.7582399583376,-101.113509484299,
174.328630986959));
#28128=CARTESIAN_POINT('Ctrl Pts',(-61.7483018264834,-101.020287726993,
175.985485236451));
#28129=CARTESIAN_POINT('Ctrl Pts',(-61.7383636946293,-100.927065969686,
177.642339485944));
#28130=CARTESIAN_POINT('Ctrl Pts',(-60.5634539471956,-100.958037969653,
178.813912312176));
#28131=CARTESIAN_POINT('Ctrl Pts',(-59.388544199762,-100.98900996962,179.985485138407));
#28132=CARTESIAN_POINT('Ctrl Pts',(-57.7310874497581,-101.071424703906,
179.985485069079));
#28133=CARTESIAN_POINT('Ctrl Pts',(-56.0736306997542,-101.153839438193,
179.985484999752));
#28134=CARTESIAN_POINT('Ctrl Pts',(-54.8987210498124,-101.184811427766,
178.813912075476));
#28135=CARTESIAN_POINT('Ctrl Pts',(-53.7238113998707,-101.21578341734,177.6423391512));
#28136=CARTESIAN_POINT('Ctrl Pts',(-53.7138734058908,-101.122561645335,
175.985484901707));
#28137=CARTESIAN_POINT('Ctrl Pts',(-53.7039354119109,-101.029339873331,
174.328630652215));
#28138=CARTESIAN_POINT('Ctrl Pts',(-54.8589690335105,-100.811924344053,
173.157057825983));
#28139=CARTESIAN_POINT('Ctrl Pts',(-56.0140026551102,-100.594508814776,
171.985484999752));
#28140=CARTESIAN_POINT('Ctrl Pts',(-57.65158327928,-100.325650551179,171.985485069079));
#28141=CARTESIAN_POINT('Ctrl Pts',(-59.2891639034499,-100.056792287582,
171.985485138407));
#28142=CARTESIAN_POINT('Ctrl Pts',(-60.4441974275576,-99.8393767686974,
173.157058062683));
#28143=CARTESIAN_POINT('Ctrl Pts',(-61.5992309516654,-99.6219612498133,
174.328630986959));
#28144=CARTESIAN_POINT('Ctrl Pts',(-61.5892928198112,-99.528739492507,175.985485236451));
#28145=CARTESIAN_POINT('Ctrl Pts',(-61.579354687957,-99.4355177352008,177.642339485944));
#28146=CARTESIAN_POINT('Ctrl Pts',(-60.4044449405234,-99.4664897351676,
178.813912312176));
#28147=CARTESIAN_POINT('Ctrl Pts',(-59.2295351930898,-99.4974617351344,
179.985485138407));
#28148=CARTESIAN_POINT('Ctrl Pts',(-57.5720784430859,-99.5798764694207,
179.985485069079));
#28149=CARTESIAN_POINT('Ctrl Pts',(-55.914621693082,-99.662291203707,179.985484999752));
#28150=CARTESIAN_POINT('Ctrl Pts',(-54.7397120431402,-99.6932631932805,
178.813912075476));
#28151=CARTESIAN_POINT('Ctrl Pts',(-53.5648023931984,-99.724235182854,177.6423391512));
#28152=CARTESIAN_POINT('Ctrl Pts',(-53.5548643992186,-99.6310134108495,
175.985484901707));
#28153=CARTESIAN_POINT('Ctrl Pts',(-53.5449264052387,-99.5377916388449,
174.328630652215));
#28154=CARTESIAN_POINT('Ctrl Pts',(-54.6999600268383,-99.3203761095675,
173.157057825983));
#28155=CARTESIAN_POINT('Ctrl Pts',(-55.8549936484379,-99.10296058029,171.985484999752));
#28156=CARTESIAN_POINT('Ctrl Pts',(-57.4925742726078,-98.834102316693,171.985485069079));
#28157=CARTESIAN_POINT('Ctrl Pts',(-59.1301548967777,-98.5652440530961,
171.985485138407));
#28158=CARTESIAN_POINT('Ctrl Pts',(-60.2851884208854,-98.3478285342118,
173.157058062683));
#28159=CARTESIAN_POINT('Ctrl Pts',(-61.4402219449932,-98.1304130153276,
174.328630986959));
#28160=CARTESIAN_POINT('Ctrl Pts',(-61.430283813139,-98.0371912580215,175.985485236451));
#28161=CARTESIAN_POINT('Ctrl Pts',(-61.4203456812848,-97.9439695007152,
177.642339485944));
#28162=CARTESIAN_POINT('Ctrl Pts',(-60.2454359338512,-97.974941500682,178.813912312176));
#28163=CARTESIAN_POINT('Ctrl Pts',(-59.0705261864175,-98.0059135006488,
179.985485138407));
#28164=CARTESIAN_POINT('Ctrl Pts',(-57.4130694364136,-98.0883282349351,
179.985485069079));
#28165=CARTESIAN_POINT('Ctrl Pts',(-55.7556126864097,-98.1707429692214,
179.985484999752));
#28166=CARTESIAN_POINT('Ctrl Pts',(-54.580703036468,-98.2017149587949,178.813912075476));
#28167=CARTESIAN_POINT('Ctrl Pts',(-56.181115489574,-113.283598570176,178.821287383467));
#28168=CARTESIAN_POINT('Ctrl Pts',(-55.0031681001975,-113.314894403068,
177.646659506339));
#28169=CARTESIAN_POINT('Ctrl Pts',(-54.9932301063974,-113.221672631044,
175.985484901271));
#28170=CARTESIAN_POINT('Ctrl Pts',(-54.9832921125973,-113.12845085902,174.324310296203));
#28171=CARTESIAN_POINT('Ctrl Pts',(-56.1413634738858,-112.910711486397,
173.149682517375));
#28172=CARTESIAN_POINT('Ctrl Pts',(-57.2994348351743,-112.692972113774,
171.975054738546));
#28173=CARTESIAN_POINT('Ctrl Pts',(-58.9413114718314,-112.423655866545,
171.975054808055));
#28174=CARTESIAN_POINT('Ctrl Pts',(-60.5831881084886,-112.154339619316,
171.975054877564));
#28175=CARTESIAN_POINT('Ctrl Pts',(-61.741259372031,-111.936600257113,173.149682754692));
#28176=CARTESIAN_POINT('Ctrl Pts',(-62.8993306355734,-111.71886089491,174.32431063182));
#28177=CARTESIAN_POINT('Ctrl Pts',(-62.8893925035395,-111.625639137623,
175.985485236888));
#28178=CARTESIAN_POINT('Ctrl Pts',(-62.8794543715055,-111.532417380336,
177.646659841956));
#28179=CARTESIAN_POINT('Ctrl Pts',(-61.701506884383,-111.563713223648,178.821287620784));
#28180=CARTESIAN_POINT('Ctrl Pts',(-60.5235593972605,-111.595009066961,
179.995915399612));
#28181=CARTESIAN_POINT('Ctrl Pts',(-58.8618066347693,-111.677881784879,
179.995915330104));
#28182=CARTESIAN_POINT('Ctrl Pts',(-57.2000538722782,-111.760754502798,
179.995915260595));
#28183=CARTESIAN_POINT('Ctrl Pts',(-56.0221064829017,-111.79205033569,178.821287383467));
#28184=CARTESIAN_POINT('Ctrl Pts',(-54.8441590935253,-111.823346168582,
177.646659506339));
#28185=CARTESIAN_POINT('Ctrl Pts',(-54.8342210997252,-111.730124396559,
175.985484901271));
#28186=CARTESIAN_POINT('Ctrl Pts',(-54.8242831059251,-111.636902624535,
174.324310296203));
#28187=CARTESIAN_POINT('Ctrl Pts',(-55.9823544672136,-111.419163251912,
173.149682517375));
#28188=CARTESIAN_POINT('Ctrl Pts',(-57.1404258285021,-111.201423879289,
171.975054738546));
#28189=CARTESIAN_POINT('Ctrl Pts',(-58.7823024651592,-110.932107632059,
171.975054808055));
#28190=CARTESIAN_POINT('Ctrl Pts',(-60.4241791018163,-110.66279138483,171.975054877564));
#28191=CARTESIAN_POINT('Ctrl Pts',(-61.5822503653587,-110.445052022627,
173.149682754692));
#28192=CARTESIAN_POINT('Ctrl Pts',(-62.7403216289012,-110.227312660424,
174.32431063182));
#28193=CARTESIAN_POINT('Ctrl Pts',(-62.7303834968672,-110.134090903137,
175.985485236888));
#28194=CARTESIAN_POINT('Ctrl Pts',(-62.7204453648333,-110.04086914585,177.646659841956));
#28195=CARTESIAN_POINT('Ctrl Pts',(-61.5424978777108,-110.072164989163,
178.821287620784));
#28196=CARTESIAN_POINT('Ctrl Pts',(-60.3645503905882,-110.103460832475,
179.995915399612));
#28197=CARTESIAN_POINT('Ctrl Pts',(-58.7027976280971,-110.186333550394,
179.995915330104));
#28198=CARTESIAN_POINT('Ctrl Pts',(-57.041044865606,-110.269206268313,179.995915260595));
#28199=CARTESIAN_POINT('Ctrl Pts',(-55.8630974762295,-110.300502101205,
178.821287383467));
#28200=CARTESIAN_POINT('Ctrl Pts',(-54.6851500868531,-110.331797934097,
177.646659506339));
#28201=CARTESIAN_POINT('Ctrl Pts',(-54.675212093053,-110.238576162073,175.985484901271));
#28202=CARTESIAN_POINT('Ctrl Pts',(-54.6652740992529,-110.145354390049,
174.324310296203));
#28203=CARTESIAN_POINT('Ctrl Pts',(-55.8233454605414,-109.927615017426,
173.149682517375));
#28204=CARTESIAN_POINT('Ctrl Pts',(-56.9814168218299,-109.709875644803,
171.975054738546));
#28205=CARTESIAN_POINT('Ctrl Pts',(-58.623293458487,-109.440559397574,171.975054808055));
#28206=CARTESIAN_POINT('Ctrl Pts',(-60.2651700951441,-109.171243150344,
171.975054877564));
#28207=CARTESIAN_POINT('Ctrl Pts',(-61.4232413586865,-108.953503788142,
173.149682754692));
#28208=CARTESIAN_POINT('Ctrl Pts',(-62.581312622229,-108.735764425939,174.32431063182));
#28209=CARTESIAN_POINT('Ctrl Pts',(-62.571374490195,-108.642542668652,175.985485236888));
#28210=CARTESIAN_POINT('Ctrl Pts',(-62.5614363581611,-108.549320911365,
177.646659841956));
#28211=CARTESIAN_POINT('Ctrl Pts',(-61.3834888710385,-108.580616754677,
178.821287620784));
#28212=CARTESIAN_POINT('Ctrl Pts',(-60.205541383916,-108.61191259799,179.995915399612));
#28213=CARTESIAN_POINT('Ctrl Pts',(-58.5437886214249,-108.694785315908,
179.995915330104));
#28214=CARTESIAN_POINT('Ctrl Pts',(-56.8820358589338,-108.777658033827,
179.995915260595));
#28215=CARTESIAN_POINT('Ctrl Pts',(-55.7040884695573,-108.808953866719,
178.821287383467));
#28216=CARTESIAN_POINT('Ctrl Pts',(-54.5261410801808,-108.840249699611,
177.646659506339));
#28217=CARTESIAN_POINT('Ctrl Pts',(-54.5162030863807,-108.747027927587,
175.985484901271));
#28218=CARTESIAN_POINT('Ctrl Pts',(-54.5062650925806,-108.653806155564,
174.324310296203));
#28219=CARTESIAN_POINT('Ctrl Pts',(-55.6643364538691,-108.436066782941,
173.149682517375));
#28220=CARTESIAN_POINT('Ctrl Pts',(-56.8224078151577,-108.218327410317,
171.975054738546));
#28221=CARTESIAN_POINT('Ctrl Pts',(-58.4642844518147,-107.949011163088,
171.975054808055));
#28222=CARTESIAN_POINT('Ctrl Pts',(-60.1061610884719,-107.679694915859,
171.975054877564));
#28223=CARTESIAN_POINT('Ctrl Pts',(-61.2642323520143,-107.461955553656,
173.149682754692));
#28224=CARTESIAN_POINT('Ctrl Pts',(-62.4223036155567,-107.244216191453,
174.32431063182));
#28225=CARTESIAN_POINT('Ctrl Pts',(-62.4123654835228,-107.150994434166,
175.985485236888));
#28226=CARTESIAN_POINT('Ctrl Pts',(-62.4024273514889,-107.057772676879,
177.646659841956));
#28227=CARTESIAN_POINT('Ctrl Pts',(-61.2244798643663,-107.089068520192,
178.821287620784));
#28228=CARTESIAN_POINT('Ctrl Pts',(-60.0465323772438,-107.120364363504,
179.995915399612));
#28229=CARTESIAN_POINT('Ctrl Pts',(-58.3847796147526,-107.203237081423,
179.995915330104));
#28230=CARTESIAN_POINT('Ctrl Pts',(-56.7230268522615,-107.286109799341,
179.995915260595));
#28231=CARTESIAN_POINT('Ctrl Pts',(-55.5450794628851,-107.317405632233,
178.821287383467));
#28232=CARTESIAN_POINT('Ctrl Pts',(-54.3671320735086,-107.348701465125,
177.646659506339));
#28233=CARTESIAN_POINT('Ctrl Pts',(-54.3571940797085,-107.255479693102,
175.985484901271));
#28234=CARTESIAN_POINT('Ctrl Pts',(-54.3472560859084,-107.162257921078,
174.324310296203));
#28235=CARTESIAN_POINT('Ctrl Pts',(-55.5053274471969,-106.944518548455,
173.149682517375));
#28236=CARTESIAN_POINT('Ctrl Pts',(-56.6633988084854,-106.726779175832,
171.975054738546));
#28237=CARTESIAN_POINT('Ctrl Pts',(-58.3052754451425,-106.457462928602,
171.975054808055));
#28238=CARTESIAN_POINT('Ctrl Pts',(-59.9471520817997,-106.188146681373,
171.975054877564));
#28239=CARTESIAN_POINT('Ctrl Pts',(-61.1052233453421,-105.97040731917,173.149682754692));
#28240=CARTESIAN_POINT('Ctrl Pts',(-62.2632946088845,-105.752667956968,
174.32431063182));
#28241=CARTESIAN_POINT('Ctrl Pts',(-62.2533564768505,-105.659446199681,
175.985485236888));
#28242=CARTESIAN_POINT('Ctrl Pts',(-62.2434183448166,-105.566224442394,
177.646659841956));
#28243=CARTESIAN_POINT('Ctrl Pts',(-61.0654708576941,-105.597520285706,
178.821287620784));
#28244=CARTESIAN_POINT('Ctrl Pts',(-59.8875233705716,-105.628816129018,
179.995915399612));
#28245=CARTESIAN_POINT('Ctrl Pts',(-58.2257706080804,-105.711688846937,
179.995915330104));
#28246=CARTESIAN_POINT('Ctrl Pts',(-56.5640178455893,-105.794561564856,
179.995915260595));
#28247=CARTESIAN_POINT('Ctrl Pts',(-55.3860704562128,-105.825857397748,
178.821287383467));
#28248=CARTESIAN_POINT('Ctrl Pts',(-54.2081230668364,-105.85715323064,177.646659506339));
#28249=CARTESIAN_POINT('Ctrl Pts',(-54.1981850730363,-105.763931458616,
175.985484901271));
#28250=CARTESIAN_POINT('Ctrl Pts',(-54.1882470792362,-105.670709686593,
174.324310296203));
#28251=CARTESIAN_POINT('Ctrl Pts',(-55.3463184405247,-105.452970313969,
173.149682517375));
#28252=CARTESIAN_POINT('Ctrl Pts',(-56.5043898018132,-105.235230941346,
171.975054738546));
#28253=CARTESIAN_POINT('Ctrl Pts',(-58.1462664384703,-104.965914694117,
171.975054808055));
#28254=CARTESIAN_POINT('Ctrl Pts',(-59.7881430751274,-104.696598446888,
171.975054877564));
#28255=CARTESIAN_POINT('Ctrl Pts',(-60.9462143386698,-104.478859084685,
173.149682754692));
#28256=CARTESIAN_POINT('Ctrl Pts',(-62.1042856022123,-104.261119722482,
174.32431063182));
#28257=CARTESIAN_POINT('Ctrl Pts',(-62.0943474701783,-104.167897965195,
175.985485236888));
#28258=CARTESIAN_POINT('Ctrl Pts',(-62.0844093381444,-104.074676207908,
177.646659841956));
#28259=CARTESIAN_POINT('Ctrl Pts',(-60.9064618510219,-104.10597205122,178.821287620784));
#28260=CARTESIAN_POINT('Ctrl Pts',(-59.7285143638993,-104.137267894533,
179.995915399612));
#28261=CARTESIAN_POINT('Ctrl Pts',(-58.0667616014082,-104.220140612451,
179.995915330104));
#28262=CARTESIAN_POINT('Ctrl Pts',(-56.4050088389171,-104.30301333037,179.995915260595));
#28263=CARTESIAN_POINT('Ctrl Pts',(-55.2270614495406,-104.334309163262,
178.821287383467));
#28264=CARTESIAN_POINT('Ctrl Pts',(-54.0491140601642,-104.365604996154,
177.646659506339));
#28265=CARTESIAN_POINT('Ctrl Pts',(-54.039176066364,-104.272383224131,175.985484901271));
#28266=CARTESIAN_POINT('Ctrl Pts',(-54.029238072564,-104.179161452107,174.324310296203));
#28267=CARTESIAN_POINT('Ctrl Pts',(-55.1873094338524,-103.961422079484,
173.149682517375));
#28268=CARTESIAN_POINT('Ctrl Pts',(-56.345380795141,-103.743682706861,171.975054738546));
#28269=CARTESIAN_POINT('Ctrl Pts',(-57.9872574317981,-103.474366459631,
171.975054808055));
#28270=CARTESIAN_POINT('Ctrl Pts',(-59.6291340684552,-103.205050212402,
171.975054877564));
#28271=CARTESIAN_POINT('Ctrl Pts',(-60.7872053319976,-102.987310850199,
173.149682754692));
#28272=CARTESIAN_POINT('Ctrl Pts',(-61.94527659554,-102.769571487996,174.32431063182));
#28273=CARTESIAN_POINT('Ctrl Pts',(-61.9353384635061,-102.676349730709,
175.985485236888));
#28274=CARTESIAN_POINT('Ctrl Pts',(-61.9254003314722,-102.583127973422,
177.646659841956));
#28275=CARTESIAN_POINT('Ctrl Pts',(-60.7474528443496,-102.614423816735,
178.821287620784));
#28276=CARTESIAN_POINT('Ctrl Pts',(-59.5695053572271,-102.645719660047,
179.995915399612));
#28277=CARTESIAN_POINT('Ctrl Pts',(-57.907752594736,-102.728592377966,179.995915330104));
#28278=CARTESIAN_POINT('Ctrl Pts',(-56.2459998322448,-102.811465095885,
179.995915260595));
#28279=CARTESIAN_POINT('Ctrl Pts',(-55.0680524428684,-102.842760928777,
178.821287383467));
#28280=CARTESIAN_POINT('Ctrl Pts',(-53.8901050534919,-102.874056761669,
177.646659506339));
#28281=CARTESIAN_POINT('Ctrl Pts',(-53.8801670596918,-102.780834989645,
175.985484901271));
#28282=CARTESIAN_POINT('Ctrl Pts',(-53.8702290658917,-102.687613217621,
174.324310296203));
#28283=CARTESIAN_POINT('Ctrl Pts',(-55.0283004271802,-102.469873844998,
173.149682517375));
#28284=CARTESIAN_POINT('Ctrl Pts',(-56.1863717884687,-102.252134472375,
171.975054738546));
#28285=CARTESIAN_POINT('Ctrl Pts',(-57.8282484251258,-101.982818225146,
171.975054808055));
#28286=CARTESIAN_POINT('Ctrl Pts',(-59.470125061783,-101.713501977916,171.975054877564));
#28287=CARTESIAN_POINT('Ctrl Pts',(-60.6281963253254,-101.495762615714,
173.149682754692));
#28288=CARTESIAN_POINT('Ctrl Pts',(-61.7862675888678,-101.278023253511,
174.32431063182));
#28289=CARTESIAN_POINT('Ctrl Pts',(-61.7763294568339,-101.184801496224,
175.985485236888));
#28290=CARTESIAN_POINT('Ctrl Pts',(-61.7663913247999,-101.091579738937,
177.646659841956));
#28291=CARTESIAN_POINT('Ctrl Pts',(-60.5884438376774,-101.122875582249,
178.821287620784));
#28292=CARTESIAN_POINT('Ctrl Pts',(-59.4104963505549,-101.154171425562,
179.995915399612));
#28293=CARTESIAN_POINT('Ctrl Pts',(-57.7487435880637,-101.23704414348,179.995915330104));
#28294=CARTESIAN_POINT('Ctrl Pts',(-56.0869908255726,-101.319916861399,
179.995915260595));
#28295=CARTESIAN_POINT('Ctrl Pts',(-54.9090434361961,-101.351212694291,
178.821287383467));
#28296=CARTESIAN_POINT('Ctrl Pts',(-53.7310960468197,-101.382508527183,
177.646659506339));
#28297=CARTESIAN_POINT('Ctrl Pts',(-53.7211580530196,-101.289286755159,
175.985484901271));
#28298=CARTESIAN_POINT('Ctrl Pts',(-53.7112200592195,-101.196064983136,
174.324310296203));
#28299=CARTESIAN_POINT('Ctrl Pts',(-54.869291420508,-100.978325610513,173.149682517375));
#28300=CARTESIAN_POINT('Ctrl Pts',(-56.0273627817965,-100.760586237889,
171.975054738546));
#28301=CARTESIAN_POINT('Ctrl Pts',(-57.6692394184536,-100.49126999066,171.975054808055));
#28302=CARTESIAN_POINT('Ctrl Pts',(-59.3111160551107,-100.221953743431,
171.975054877564));
#28303=CARTESIAN_POINT('Ctrl Pts',(-60.4691873186531,-100.004214381228,
173.149682754692));
#28304=CARTESIAN_POINT('Ctrl Pts',(-61.6272585821956,-99.7864750190253,
174.32431063182));
#28305=CARTESIAN_POINT('Ctrl Pts',(-61.6173204501616,-99.6932532617382,
175.985485236888));
#28306=CARTESIAN_POINT('Ctrl Pts',(-61.6073823181277,-99.6000315044512,
177.646659841956));
#28307=CARTESIAN_POINT('Ctrl Pts',(-60.4294348310052,-99.6313273477637,
178.821287620784));
#28308=CARTESIAN_POINT('Ctrl Pts',(-59.2514873438827,-99.6626231910761,
179.995915399612));
#28309=CARTESIAN_POINT('Ctrl Pts',(-57.5897345813915,-99.7454959089947,
179.995915330104));
#28310=CARTESIAN_POINT('Ctrl Pts',(-55.9279818189004,-99.8283686269133,
179.995915260595));
#28311=CARTESIAN_POINT('Ctrl Pts',(-54.7500344295239,-99.8596644598054,
178.821287383467));
#28312=CARTESIAN_POINT('Ctrl Pts',(-53.5720870401475,-99.8909602926975,
177.646659506339));
#28313=CARTESIAN_POINT('Ctrl Pts',(-53.5621490463474,-99.7977385206737,
175.985484901271));
#28314=CARTESIAN_POINT('Ctrl Pts',(-53.5522110525473,-99.7045167486501,
174.324310296203));
#28315=CARTESIAN_POINT('Ctrl Pts',(-54.7102824138358,-99.4867773760269,
173.149682517375));
#28316=CARTESIAN_POINT('Ctrl Pts',(-55.8683537751243,-99.2690380034038,
171.975054738546));
#28317=CARTESIAN_POINT('Ctrl Pts',(-57.5102304117814,-98.9997217561745,
171.975054808055));
#28318=CARTESIAN_POINT('Ctrl Pts',(-59.1521070484385,-98.7304055089452,
171.975054877564));
#28319=CARTESIAN_POINT('Ctrl Pts',(-60.3101783119809,-98.5126661467424,
173.149682754692));
#28320=CARTESIAN_POINT('Ctrl Pts',(-61.4682495755234,-98.2949267845397,
174.32431063182));
#28321=CARTESIAN_POINT('Ctrl Pts',(-61.4583114434894,-98.2017050272526,
175.985485236888));
#28322=CARTESIAN_POINT('Ctrl Pts',(-61.4483733114555,-98.1084832699656,
177.646659841956));
#28323=CARTESIAN_POINT('Ctrl Pts',(-60.2704258243329,-98.139779113278,178.821287620784));
#28324=CARTESIAN_POINT('Ctrl Pts',(-59.0924783372104,-98.1710749565905,
179.995915399612));
#28325=CARTESIAN_POINT('Ctrl Pts',(-57.4307255747193,-98.2539476745091,
179.995915330104));
#28326=CARTESIAN_POINT('Ctrl Pts',(-55.7689728122282,-98.3368203924277,
179.995915260595));
#28327=CARTESIAN_POINT('Ctrl Pts',(-54.5910254228517,-98.3681162253198,
178.821287383467));
#28328=CARTESIAN_POINT('Ctrl Pts',(-56.1988062143188,-113.449542435949,
178.821287383467));
#28329=CARTESIAN_POINT('Ctrl Pts',(-55.0208588249424,-113.480838268841,
177.646659506339));
#28330=CARTESIAN_POINT('Ctrl Pts',(-55.0109208311422,-113.387616496817,
175.985484901271));
#28331=CARTESIAN_POINT('Ctrl Pts',(-55.0009828373422,-113.294394724794,
174.324310296203));
#28332=CARTESIAN_POINT('Ctrl Pts',(-56.1590541986307,-113.07665535217,173.149682517375));
#28333=CARTESIAN_POINT('Ctrl Pts',(-57.3171255599192,-112.858915979547,
171.975054738546));
#28334=CARTESIAN_POINT('Ctrl Pts',(-58.9590021965763,-112.589599732318,
171.975054808055));
#28335=CARTESIAN_POINT('Ctrl Pts',(-60.6008788332334,-112.320283485089,
171.975054877564));
#28336=CARTESIAN_POINT('Ctrl Pts',(-61.7589500967758,-112.102544122886,
173.149682754692));
#28337=CARTESIAN_POINT('Ctrl Pts',(-62.9170213603182,-111.884804760683,
174.32431063182));
#28338=CARTESIAN_POINT('Ctrl Pts',(-62.9070832282843,-111.791583003396,
175.985485236888));
#28339=CARTESIAN_POINT('Ctrl Pts',(-62.8971450962504,-111.698361246109,
177.646659841956));
#28340=CARTESIAN_POINT('Ctrl Pts',(-61.7191976091278,-111.729657089422,
178.821287620784));
#28341=CARTESIAN_POINT('Ctrl Pts',(-60.5412501220053,-111.760952932734,
179.995915399612));
#28342=CARTESIAN_POINT('Ctrl Pts',(-58.8794973595142,-111.843825650653,
179.995915330104));
#28343=CARTESIAN_POINT('Ctrl Pts',(-57.217744597023,-111.926698368571,179.995915260595));
#28344=CARTESIAN_POINT('Ctrl Pts',(-56.0397972076466,-111.957994201463,
178.821287383467));
#28345=CARTESIAN_POINT('Ctrl Pts',(-54.8618498182701,-111.989290034355,
177.646659506339));
#28346=CARTESIAN_POINT('Ctrl Pts',(-54.85191182447,-111.896068262332,175.985484901271));
#28347=CARTESIAN_POINT('Ctrl Pts',(-54.8419738306699,-111.802846490308,
174.324310296203));
#28348=CARTESIAN_POINT('Ctrl Pts',(-56.0000451919584,-111.585107117685,
173.149682517375));
#28349=CARTESIAN_POINT('Ctrl Pts',(-57.158116553247,-111.367367745062,171.975054738546));
#28350=CARTESIAN_POINT('Ctrl Pts',(-58.799993189904,-111.098051497832,171.975054808055));
#28351=CARTESIAN_POINT('Ctrl Pts',(-60.4418698265612,-110.828735250603,
171.975054877564));
#28352=CARTESIAN_POINT('Ctrl Pts',(-61.5999410901036,-110.6109958884,173.149682754692));
#28353=CARTESIAN_POINT('Ctrl Pts',(-62.758012353646,-110.393256526198,174.32431063182));
#28354=CARTESIAN_POINT('Ctrl Pts',(-62.7480742216121,-110.30003476891,175.985485236888));
#28355=CARTESIAN_POINT('Ctrl Pts',(-62.7381360895782,-110.206813011623,
177.646659841956));
#28356=CARTESIAN_POINT('Ctrl Pts',(-61.5601886024556,-110.238108854936,
178.821287620784));
#28357=CARTESIAN_POINT('Ctrl Pts',(-60.3822411153331,-110.269404698248,
179.995915399612));
#28358=CARTESIAN_POINT('Ctrl Pts',(-58.7204883528419,-110.352277416167,
179.995915330104));
#28359=CARTESIAN_POINT('Ctrl Pts',(-57.0587355903508,-110.435150134086,
179.995915260595));
#28360=CARTESIAN_POINT('Ctrl Pts',(-55.8807882009743,-110.466445966978,
178.821287383467));
#28361=CARTESIAN_POINT('Ctrl Pts',(-54.7028408115979,-110.49774179987,177.646659506339));
#28362=CARTESIAN_POINT('Ctrl Pts',(-54.6929028177978,-110.404520027846,
175.985484901271));
#28363=CARTESIAN_POINT('Ctrl Pts',(-54.6829648239977,-110.311298255822,
174.324310296203));
#28364=CARTESIAN_POINT('Ctrl Pts',(-55.8410361852862,-110.093558883199,
173.149682517375));
#28365=CARTESIAN_POINT('Ctrl Pts',(-56.9991075465747,-109.875819510576,
171.975054738546));
#28366=CARTESIAN_POINT('Ctrl Pts',(-58.6409841832318,-109.606503263347,
171.975054808055));
#28367=CARTESIAN_POINT('Ctrl Pts',(-60.2828608198889,-109.337187016117,
171.975054877564));
#28368=CARTESIAN_POINT('Ctrl Pts',(-61.4409320834313,-109.119447653915,
173.149682754692));
#28369=CARTESIAN_POINT('Ctrl Pts',(-62.5990033469738,-108.901708291712,
174.32431063182));
#28370=CARTESIAN_POINT('Ctrl Pts',(-62.5890652149398,-108.808486534425,
175.985485236888));
#28371=CARTESIAN_POINT('Ctrl Pts',(-62.5791270829059,-108.715264777138,
177.646659841956));
#28372=CARTESIAN_POINT('Ctrl Pts',(-61.4011795957834,-108.74656062045,178.821287620784));
#28373=CARTESIAN_POINT('Ctrl Pts',(-60.2232321086609,-108.777856463763,
179.995915399612));
#28374=CARTESIAN_POINT('Ctrl Pts',(-58.5614793461697,-108.860729181681,
179.995915330104));
#28375=CARTESIAN_POINT('Ctrl Pts',(-56.8997265836786,-108.9436018996,179.995915260595));
#28376=CARTESIAN_POINT('Ctrl Pts',(-55.7217791943021,-108.974897732492,
178.821287383467));
#28377=CARTESIAN_POINT('Ctrl Pts',(-54.5438318049257,-109.006193565384,
177.646659506339));
#28378=CARTESIAN_POINT('Ctrl Pts',(-54.5338938111256,-108.91297179336,175.985484901271));
#28379=CARTESIAN_POINT('Ctrl Pts',(-54.5239558173255,-108.819750021337,
174.324310296203));
#28380=CARTESIAN_POINT('Ctrl Pts',(-55.682027178614,-108.602010648714,173.149682517375));
#28381=CARTESIAN_POINT('Ctrl Pts',(-56.8400985399025,-108.384271276091,
171.975054738546));
#28382=CARTESIAN_POINT('Ctrl Pts',(-58.4819751765596,-108.114955028861,
171.975054808055));
#28383=CARTESIAN_POINT('Ctrl Pts',(-60.1238518132167,-107.845638781632,
171.975054877564));
#28384=CARTESIAN_POINT('Ctrl Pts',(-61.2819230767591,-107.627899419429,
173.149682754692));
#28385=CARTESIAN_POINT('Ctrl Pts',(-62.4399943403016,-107.410160057226,
174.32431063182));
#28386=CARTESIAN_POINT('Ctrl Pts',(-62.4300562082676,-107.316938299939,
175.985485236888));
#28387=CARTESIAN_POINT('Ctrl Pts',(-62.4201180762337,-107.223716542652,
177.646659841956));
#28388=CARTESIAN_POINT('Ctrl Pts',(-61.2421705891111,-107.255012385965,
178.821287620784));
#28389=CARTESIAN_POINT('Ctrl Pts',(-60.0642231019886,-107.286308229277,
179.995915399612));
#28390=CARTESIAN_POINT('Ctrl Pts',(-58.4024703394975,-107.369180947196,
179.995915330104));
#28391=CARTESIAN_POINT('Ctrl Pts',(-56.7407175770064,-107.452053665114,
179.995915260595));
#28392=CARTESIAN_POINT('Ctrl Pts',(-55.5627701876299,-107.483349498006,
178.821287383467));
#28393=CARTESIAN_POINT('Ctrl Pts',(-54.3848227982534,-107.514645330899,
177.646659506339));
#28394=CARTESIAN_POINT('Ctrl Pts',(-54.3748848044533,-107.421423558875,
175.985484901271));
#28395=CARTESIAN_POINT('Ctrl Pts',(-54.3649468106533,-107.328201786851,
174.324310296203));
#28396=CARTESIAN_POINT('Ctrl Pts',(-55.5230181719417,-107.110462414228,
173.149682517375));
#28397=CARTESIAN_POINT('Ctrl Pts',(-56.6810895332303,-106.892723041605,
171.975054738546));
#28398=CARTESIAN_POINT('Ctrl Pts',(-58.3229661698874,-106.623406794376,
171.975054808055));
#28399=CARTESIAN_POINT('Ctrl Pts',(-59.9648428065445,-106.354090547146,
171.975054877564));
#28400=CARTESIAN_POINT('Ctrl Pts',(-61.1229140700869,-106.136351184943,
173.149682754692));
#28401=CARTESIAN_POINT('Ctrl Pts',(-62.2809853336293,-105.918611822741,
174.32431063182));
#28402=CARTESIAN_POINT('Ctrl Pts',(-62.2710472015954,-105.825390065454,
175.985485236888));
#28403=CARTESIAN_POINT('Ctrl Pts',(-62.2611090695615,-105.732168308167,
177.646659841956));
#28404=CARTESIAN_POINT('Ctrl Pts',(-61.0831615824389,-105.763464151479,
178.821287620784));
#28405=CARTESIAN_POINT('Ctrl Pts',(-59.9052140953164,-105.794759994792,
179.995915399612));
#28406=CARTESIAN_POINT('Ctrl Pts',(-58.2434613328252,-105.87763271271,179.995915330104));
#28407=CARTESIAN_POINT('Ctrl Pts',(-56.5817085703341,-105.960505430629,
179.995915260595));
#28408=CARTESIAN_POINT('Ctrl Pts',(-55.4037611809577,-105.991801263521,
178.821287383467));
#28409=CARTESIAN_POINT('Ctrl Pts',(-54.2258137915812,-106.023097096413,
177.646659506339));
#28410=CARTESIAN_POINT('Ctrl Pts',(-54.2158757977811,-105.929875324389,
175.985484901271));
#28411=CARTESIAN_POINT('Ctrl Pts',(-54.205937803981,-105.836653552366,174.324310296203));
#28412=CARTESIAN_POINT('Ctrl Pts',(-55.3640091652695,-105.618914179742,
173.149682517375));
#28413=CARTESIAN_POINT('Ctrl Pts',(-56.522080526558,-105.401174807119,171.975054738546));
#28414=CARTESIAN_POINT('Ctrl Pts',(-58.1639571632151,-105.13185855989,171.975054808055));
#28415=CARTESIAN_POINT('Ctrl Pts',(-59.8058337998722,-104.862542312661,
171.975054877564));
#28416=CARTESIAN_POINT('Ctrl Pts',(-60.9639050634147,-104.644802950458,
173.149682754692));
#28417=CARTESIAN_POINT('Ctrl Pts',(-62.1219763269571,-104.427063588255,
174.32431063182));
#28418=CARTESIAN_POINT('Ctrl Pts',(-62.1120381949232,-104.333841830968,
175.985485236888));
#28419=CARTESIAN_POINT('Ctrl Pts',(-62.1021000628892,-104.240620073681,
177.646659841956));
#28420=CARTESIAN_POINT('Ctrl Pts',(-60.9241525757667,-104.271915916993,
178.821287620784));
#28421=CARTESIAN_POINT('Ctrl Pts',(-59.7462050886442,-104.303211760306,
179.995915399612));
#28422=CARTESIAN_POINT('Ctrl Pts',(-58.084452326153,-104.386084478225,179.995915330104));
#28423=CARTESIAN_POINT('Ctrl Pts',(-56.4226995636619,-104.468957196143,
179.995915260595));
#28424=CARTESIAN_POINT('Ctrl Pts',(-55.2447521742854,-104.500253029035,
178.821287383467));
#28425=CARTESIAN_POINT('Ctrl Pts',(-54.066804784909,-104.531548861927,177.646659506339));
#28426=CARTESIAN_POINT('Ctrl Pts',(-54.0568667911089,-104.438327089904,
175.985484901271));
#28427=CARTESIAN_POINT('Ctrl Pts',(-54.0469287973088,-104.34510531788,174.324310296203));
#28428=CARTESIAN_POINT('Ctrl Pts',(-55.2050001585973,-104.127365945257,
173.149682517375));
#28429=CARTESIAN_POINT('Ctrl Pts',(-56.3630715198858,-103.909626572634,
171.975054738546));
#28430=CARTESIAN_POINT('Ctrl Pts',(-58.0049481565429,-103.640310325404,
171.975054808055));
#28431=CARTESIAN_POINT('Ctrl Pts',(-59.6468247932,-103.370994078175,171.975054877564));
#28432=CARTESIAN_POINT('Ctrl Pts',(-60.8048960567424,-103.153254715972,
173.149682754692));
#28433=CARTESIAN_POINT('Ctrl Pts',(-61.9629673202849,-102.93551535377,174.32431063182));
#28434=CARTESIAN_POINT('Ctrl Pts',(-61.9530291882509,-102.842293596483,
175.985485236888));
#28435=CARTESIAN_POINT('Ctrl Pts',(-61.943091056217,-102.749071839196,177.646659841956));
#28436=CARTESIAN_POINT('Ctrl Pts',(-60.7651435690945,-102.780367682508,
178.821287620784));
#28437=CARTESIAN_POINT('Ctrl Pts',(-59.587196081972,-102.81166352582,179.995915399612));
#28438=CARTESIAN_POINT('Ctrl Pts',(-57.9254433194808,-102.894536243739,
179.995915330104));
#28439=CARTESIAN_POINT('Ctrl Pts',(-56.2636905569897,-102.977408961658,
179.995915260595));
#28440=CARTESIAN_POINT('Ctrl Pts',(-55.0857431676132,-103.00870479455,178.821287383467));
#28441=CARTESIAN_POINT('Ctrl Pts',(-53.9077957782368,-103.040000627442,
177.646659506339));
#28442=CARTESIAN_POINT('Ctrl Pts',(-53.8978577844367,-102.946778855418,
175.985484901271));
#28443=CARTESIAN_POINT('Ctrl Pts',(-53.8879197906366,-102.853557083394,
174.324310296203));
#28444=CARTESIAN_POINT('Ctrl Pts',(-55.0459911519251,-102.635817710771,
173.149682517375));
#28445=CARTESIAN_POINT('Ctrl Pts',(-56.2040625132136,-102.418078338148,
171.975054738546));
#28446=CARTESIAN_POINT('Ctrl Pts',(-57.8459391498707,-102.148762090919,
171.975054808055));
#28447=CARTESIAN_POINT('Ctrl Pts',(-59.4878157865278,-101.879445843689,
171.975054877564));
#28448=CARTESIAN_POINT('Ctrl Pts',(-60.6458870500702,-101.661706481487,
173.149682754692));
#28449=CARTESIAN_POINT('Ctrl Pts',(-61.8039583136126,-101.443967119284,
174.32431063182));
#28450=CARTESIAN_POINT('Ctrl Pts',(-61.7940201815787,-101.350745361997,
175.985485236888));
#28451=CARTESIAN_POINT('Ctrl Pts',(-61.7840820495448,-101.25752360471,177.646659841956));
#28452=CARTESIAN_POINT('Ctrl Pts',(-60.6061345624222,-101.288819448022,
178.821287620784));
#28453=CARTESIAN_POINT('Ctrl Pts',(-59.4281870752997,-101.320115291335,
179.995915399612));
#28454=CARTESIAN_POINT('Ctrl Pts',(-57.7664343128086,-101.402988009253,
179.995915330104));
#28455=CARTESIAN_POINT('Ctrl Pts',(-56.1046815503175,-101.485860727172,
179.995915260595));
#28456=CARTESIAN_POINT('Ctrl Pts',(-54.926734160941,-101.517156560064,178.821287383467));
#28457=CARTESIAN_POINT('Ctrl Pts',(-53.7487867715645,-101.548452392956,
177.646659506339));
#28458=CARTESIAN_POINT('Ctrl Pts',(-53.7388487777644,-101.455230620932,
175.985484901271));
#28459=CARTESIAN_POINT('Ctrl Pts',(-53.7289107839643,-101.362008848909,
174.324310296203));
#28460=CARTESIAN_POINT('Ctrl Pts',(-54.8869821452528,-101.144269476286,
173.149682517375));
#28461=CARTESIAN_POINT('Ctrl Pts',(-56.0450535065414,-100.926530103662,
171.975054738546));
#28462=CARTESIAN_POINT('Ctrl Pts',(-57.6869301431984,-100.657213856433,
171.975054808055));
#28463=CARTESIAN_POINT('Ctrl Pts',(-59.3288067798556,-100.387897609204,
171.975054877564));
#28464=CARTESIAN_POINT('Ctrl Pts',(-60.486878043398,-100.170158247001,173.149682754692));
#28465=CARTESIAN_POINT('Ctrl Pts',(-61.6449493069404,-99.9524188847983,
174.32431063182));
#28466=CARTESIAN_POINT('Ctrl Pts',(-61.6350111749065,-99.8591971275113,
175.985485236888));
#28467=CARTESIAN_POINT('Ctrl Pts',(-61.6250730428726,-99.7659753702243,
177.646659841956));
#28468=CARTESIAN_POINT('Ctrl Pts',(-60.44712555575,-99.7972712135367,178.821287620784));
#28469=CARTESIAN_POINT('Ctrl Pts',(-59.2691780686275,-99.8285670568492,
179.995915399612));
#28470=CARTESIAN_POINT('Ctrl Pts',(-57.6074253061363,-99.9114397747677,
179.995915330104));
#28471=CARTESIAN_POINT('Ctrl Pts',(-55.9456725436452,-99.9943124926864,
179.995915260595));
#28472=CARTESIAN_POINT('Ctrl Pts',(-54.7677251542687,-100.025608325578,
178.821287383467));
#28473=CARTESIAN_POINT('Ctrl Pts',(-53.5897777648923,-100.05690415847,177.646659506339));
#28474=CARTESIAN_POINT('Ctrl Pts',(-53.5798397710922,-99.9636823864468,
175.985484901271));
#28475=CARTESIAN_POINT('Ctrl Pts',(-53.5699017772921,-99.8704606144232,
174.324310296203));
#28476=CARTESIAN_POINT('Ctrl Pts',(-54.7279731385806,-99.6527212418,173.149682517375));
#28477=CARTESIAN_POINT('Ctrl Pts',(-55.8860444998691,-99.4349818691769,
171.975054738546));
#28478=CARTESIAN_POINT('Ctrl Pts',(-57.5279211365262,-99.1656656219475,
171.975054808055));
#28479=CARTESIAN_POINT('Ctrl Pts',(-59.1697977731833,-98.8963493747183,
171.975054877564));
#28480=CARTESIAN_POINT('Ctrl Pts',(-60.3278690367257,-98.6786100125155,
173.149682754692));
#28481=CARTESIAN_POINT('Ctrl Pts',(-61.4859403002682,-98.4608706503128,
174.32431063182));
#28482=CARTESIAN_POINT('Ctrl Pts',(-61.4760021682342,-98.3676488930257,
175.985485236888));
#28483=CARTESIAN_POINT('Ctrl Pts',(-61.4660640362003,-98.2744271357387,
177.646659841956));
#28484=CARTESIAN_POINT('Ctrl Pts',(-60.2881165490778,-98.3057229790511,
178.821287620784));
#28485=CARTESIAN_POINT('Ctrl Pts',(-59.1101690619552,-98.3370188223636,
179.995915399612));
#28486=CARTESIAN_POINT('Ctrl Pts',(-57.4484162994641,-98.4198915402821,
179.995915330104));
#28487=CARTESIAN_POINT('Ctrl Pts',(-55.786663536973,-98.5027642582008,179.995915260595));
#28488=CARTESIAN_POINT('Ctrl Pts',(-54.6087161475965,-98.5340600910929,
178.821287383467));
#28489=CARTESIAN_POINT('Ctrl Pts',(-56.2237961054143,-113.614380048479,
178.813912075476));
#28490=CARTESIAN_POINT('Ctrl Pts',(-55.0488864554725,-113.645352038053,
177.6423391512));
#28491=CARTESIAN_POINT('Ctrl Pts',(-55.0389484614927,-113.552130266048,
175.985484901707));
#28492=CARTESIAN_POINT('Ctrl Pts',(-55.0290104675128,-113.458908494044,
174.328630652215));
#28493=CARTESIAN_POINT('Ctrl Pts',(-56.1840440891124,-113.241492964766,
173.157057825983));
#28494=CARTESIAN_POINT('Ctrl Pts',(-57.3390777107121,-113.024077435489,
171.985484999752));
#28495=CARTESIAN_POINT('Ctrl Pts',(-58.9766583348819,-112.755219171892,
171.985485069079));
#28496=CARTESIAN_POINT('Ctrl Pts',(-60.6142389590518,-112.486360908295,
171.985485138407));
#28497=CARTESIAN_POINT('Ctrl Pts',(-61.7692724831595,-112.268945389411,
173.157058062683));
#28498=CARTESIAN_POINT('Ctrl Pts',(-62.9243060072673,-112.051529870527,
174.328630986959));
#28499=CARTESIAN_POINT('Ctrl Pts',(-62.9143678754131,-111.95830811322,175.985485236451));
#28500=CARTESIAN_POINT('Ctrl Pts',(-62.9044297435589,-111.865086355914,
177.642339485944));
#28501=CARTESIAN_POINT('Ctrl Pts',(-61.7295199961253,-111.896058355881,
178.813912312176));
#28502=CARTESIAN_POINT('Ctrl Pts',(-60.5546102486917,-111.927030355848,
179.985485138407));
#28503=CARTESIAN_POINT('Ctrl Pts',(-58.8971534986878,-112.009445090134,
179.985485069079));
#28504=CARTESIAN_POINT('Ctrl Pts',(-57.2396967486839,-112.09185982442,179.985484999752));
#28505=CARTESIAN_POINT('Ctrl Pts',(-56.0647870987421,-112.122831813994,
178.813912075476));
#28506=CARTESIAN_POINT('Ctrl Pts',(-54.8898774488003,-112.153803803567,
177.6423391512));
#28507=CARTESIAN_POINT('Ctrl Pts',(-54.8799394548205,-112.060582031563,
175.985484901707));
#28508=CARTESIAN_POINT('Ctrl Pts',(-54.8700014608406,-111.967360259558,
174.328630652215));
#28509=CARTESIAN_POINT('Ctrl Pts',(-56.0250350824402,-111.749944730281,
173.157057825983));
#28510=CARTESIAN_POINT('Ctrl Pts',(-57.1800687040398,-111.532529201003,
171.985484999752));
#28511=CARTESIAN_POINT('Ctrl Pts',(-58.8176493282097,-111.263670937406,
171.985485069079));
#28512=CARTESIAN_POINT('Ctrl Pts',(-60.4552299523796,-110.994812673809,
171.985485138407));
#28513=CARTESIAN_POINT('Ctrl Pts',(-61.6102634764873,-110.777397154925,
173.157058062683));
#28514=CARTESIAN_POINT('Ctrl Pts',(-62.7652970005951,-110.559981636041,
174.328630986959));
#28515=CARTESIAN_POINT('Ctrl Pts',(-62.7553588687409,-110.466759878735,
175.985485236451));
#28516=CARTESIAN_POINT('Ctrl Pts',(-62.7454207368867,-110.373538121429,
177.642339485944));
#28517=CARTESIAN_POINT('Ctrl Pts',(-61.5705109894531,-110.404510121395,
178.813912312176));
#28518=CARTESIAN_POINT('Ctrl Pts',(-60.3956012420194,-110.435482121362,
179.985485138407));
#28519=CARTESIAN_POINT('Ctrl Pts',(-58.7381444920155,-110.517896855648,
179.985485069079));
#28520=CARTESIAN_POINT('Ctrl Pts',(-57.0806877420116,-110.600311589935,
179.985484999752));
#28521=CARTESIAN_POINT('Ctrl Pts',(-55.9057780920699,-110.631283579508,
178.813912075476));
#28522=CARTESIAN_POINT('Ctrl Pts',(-54.7308684421281,-110.662255569082,
177.6423391512));
#28523=CARTESIAN_POINT('Ctrl Pts',(-54.7209304481482,-110.569033797077,
175.985484901707));
#28524=CARTESIAN_POINT('Ctrl Pts',(-54.7109924541684,-110.475812025073,
174.328630652215));
#28525=CARTESIAN_POINT('Ctrl Pts',(-55.866026075768,-110.258396495795,173.157057825983));
#28526=CARTESIAN_POINT('Ctrl Pts',(-57.0210596973676,-110.040980966518,
171.985484999752));
#28527=CARTESIAN_POINT('Ctrl Pts',(-58.6586403215375,-109.772122702921,
171.985485069079));
#28528=CARTESIAN_POINT('Ctrl Pts',(-60.2962209457073,-109.503264439324,
171.985485138407));
#28529=CARTESIAN_POINT('Ctrl Pts',(-61.4512544698151,-109.28584892044,173.157058062683));
#28530=CARTESIAN_POINT('Ctrl Pts',(-62.6062879939228,-109.068433401555,
174.328630986959));
#28531=CARTESIAN_POINT('Ctrl Pts',(-62.5963498620687,-108.975211644249,
175.985485236451));
#28532=CARTESIAN_POINT('Ctrl Pts',(-62.5864117302145,-108.881989886943,
177.642339485944));
#28533=CARTESIAN_POINT('Ctrl Pts',(-61.4115019827808,-108.91296188691,178.813912312176));
#28534=CARTESIAN_POINT('Ctrl Pts',(-60.2365922353472,-108.943933886877,
179.985485138407));
#28535=CARTESIAN_POINT('Ctrl Pts',(-58.5791354853433,-109.026348621163,
179.985485069079));
#28536=CARTESIAN_POINT('Ctrl Pts',(-56.9216787353394,-109.108763355449,
179.985484999752));
#28537=CARTESIAN_POINT('Ctrl Pts',(-55.7467690853976,-109.139735345023,
178.813912075476));
#28538=CARTESIAN_POINT('Ctrl Pts',(-54.5718594354559,-109.170707334596,
177.6423391512));
#28539=CARTESIAN_POINT('Ctrl Pts',(-54.561921441476,-109.077485562592,175.985484901707));
#28540=CARTESIAN_POINT('Ctrl Pts',(-54.5519834474962,-108.984263790587,
174.328630652215));
#28541=CARTESIAN_POINT('Ctrl Pts',(-55.7070170690958,-108.76684826131,173.157057825983));
#28542=CARTESIAN_POINT('Ctrl Pts',(-56.8620506906954,-108.549432732032,
171.985484999752));
#28543=CARTESIAN_POINT('Ctrl Pts',(-58.4996313148652,-108.280574468435,
171.985485069079));
#28544=CARTESIAN_POINT('Ctrl Pts',(-60.1372119390351,-108.011716204838,
171.985485138407));
#28545=CARTESIAN_POINT('Ctrl Pts',(-61.2922454631428,-107.794300685954,
173.157058062683));
#28546=CARTESIAN_POINT('Ctrl Pts',(-62.4472789872506,-107.57688516707,174.328630986959));
#28547=CARTESIAN_POINT('Ctrl Pts',(-62.4373408553964,-107.483663409764,
175.985485236451));
#28548=CARTESIAN_POINT('Ctrl Pts',(-62.4274027235423,-107.390441652457,
177.642339485944));
#28549=CARTESIAN_POINT('Ctrl Pts',(-61.2524929761086,-107.421413652424,
178.813912312176));
#28550=CARTESIAN_POINT('Ctrl Pts',(-60.077583228675,-107.452385652391,179.985485138407));
#28551=CARTESIAN_POINT('Ctrl Pts',(-58.4201264786711,-107.534800386677,
179.985485069079));
#28552=CARTESIAN_POINT('Ctrl Pts',(-56.7626697286672,-107.617215120964,
179.985484999752));
#28553=CARTESIAN_POINT('Ctrl Pts',(-55.5877600787254,-107.648187110537,
178.813912075476));
#28554=CARTESIAN_POINT('Ctrl Pts',(-54.4128504287836,-107.67915910011,177.6423391512));
#28555=CARTESIAN_POINT('Ctrl Pts',(-54.4029124348038,-107.585937328106,
175.985484901707));
#28556=CARTESIAN_POINT('Ctrl Pts',(-54.3929744408239,-107.492715556102,
174.328630652215));
#28557=CARTESIAN_POINT('Ctrl Pts',(-55.5480080624235,-107.275300026824,
173.157057825983));
#28558=CARTESIAN_POINT('Ctrl Pts',(-56.7030416840231,-107.057884497547,
171.985484999752));
#28559=CARTESIAN_POINT('Ctrl Pts',(-58.340622308193,-106.78902623395,171.985485069079));
#28560=CARTESIAN_POINT('Ctrl Pts',(-59.9782029323629,-106.520167970353,
171.985485138407));
#28561=CARTESIAN_POINT('Ctrl Pts',(-61.1332364564706,-106.302752451468,
173.157058062683));
#28562=CARTESIAN_POINT('Ctrl Pts',(-62.2882699805784,-106.085336932584,
174.328630986959));
#28563=CARTESIAN_POINT('Ctrl Pts',(-62.2783318487242,-105.992115175278,
175.985485236451));
#28564=CARTESIAN_POINT('Ctrl Pts',(-62.26839371687,-105.898893417972,177.642339485944));
#28565=CARTESIAN_POINT('Ctrl Pts',(-61.0934839694364,-105.929865417939,
178.813912312176));
#28566=CARTESIAN_POINT('Ctrl Pts',(-59.9185742220028,-105.960837417905,
179.985485138407));
#28567=CARTESIAN_POINT('Ctrl Pts',(-58.2611174719989,-106.043252152192,
179.985485069079));
#28568=CARTESIAN_POINT('Ctrl Pts',(-56.603660721995,-106.125666886478,179.985484999752));
#28569=CARTESIAN_POINT('Ctrl Pts',(-55.4287510720532,-106.156638876051,
178.813912075476));
#28570=CARTESIAN_POINT('Ctrl Pts',(-54.2538414221114,-106.187610865625,
177.6423391512));
#28571=CARTESIAN_POINT('Ctrl Pts',(-54.2439034281315,-106.09438909362,175.985484901707));
#28572=CARTESIAN_POINT('Ctrl Pts',(-54.2339654341517,-106.001167321616,
174.328630652215));
#28573=CARTESIAN_POINT('Ctrl Pts',(-55.3889990557513,-105.783751792338,
173.157057825983));
#28574=CARTESIAN_POINT('Ctrl Pts',(-56.5440326773509,-105.566336263061,
171.985484999752));
#28575=CARTESIAN_POINT('Ctrl Pts',(-58.1816133015208,-105.297477999464,
171.985485069079));
#28576=CARTESIAN_POINT('Ctrl Pts',(-59.8191939256906,-105.028619735867,
171.985485138407));
#28577=CARTESIAN_POINT('Ctrl Pts',(-60.9742274497984,-104.811204216983,
173.157058062683));
#28578=CARTESIAN_POINT('Ctrl Pts',(-62.1292609739061,-104.593788698099,
174.328630986959));
#28579=CARTESIAN_POINT('Ctrl Pts',(-62.119322842052,-104.500566940792,175.985485236451));
#28580=CARTESIAN_POINT('Ctrl Pts',(-62.1093847101978,-104.407345183486,
177.642339485944));
#28581=CARTESIAN_POINT('Ctrl Pts',(-60.9344749627642,-104.438317183453,
178.813912312176));
#28582=CARTESIAN_POINT('Ctrl Pts',(-59.7595652153305,-104.46928918342,179.985485138407));
#28583=CARTESIAN_POINT('Ctrl Pts',(-58.1021084653266,-104.551703917706,
179.985485069079));
#28584=CARTESIAN_POINT('Ctrl Pts',(-56.4446517153227,-104.634118651992,
179.985484999752));
#28585=CARTESIAN_POINT('Ctrl Pts',(-55.269742065381,-104.665090641566,178.813912075476));
#28586=CARTESIAN_POINT('Ctrl Pts',(-54.0948324154392,-104.696062631139,
177.6423391512));
#28587=CARTESIAN_POINT('Ctrl Pts',(-54.0848944214593,-104.602840859135,
175.985484901707));
#28588=CARTESIAN_POINT('Ctrl Pts',(-54.0749564274795,-104.50961908713,174.328630652215));
#28589=CARTESIAN_POINT('Ctrl Pts',(-55.2299900490791,-104.292203557853,
173.157057825983));
#28590=CARTESIAN_POINT('Ctrl Pts',(-56.3850236706787,-104.074788028575,
171.985484999752));
#28591=CARTESIAN_POINT('Ctrl Pts',(-58.0226042948486,-103.805929764978,
171.985485069079));
#28592=CARTESIAN_POINT('Ctrl Pts',(-59.6601849190184,-103.537071501381,
171.985485138407));
#28593=CARTESIAN_POINT('Ctrl Pts',(-60.8152184431262,-103.319655982497,
173.157058062683));
#28594=CARTESIAN_POINT('Ctrl Pts',(-61.9702519672339,-103.102240463613,
174.328630986959));
#28595=CARTESIAN_POINT('Ctrl Pts',(-61.9603138353797,-103.009018706307,
175.985485236451));
#28596=CARTESIAN_POINT('Ctrl Pts',(-61.9503757035256,-102.915796949001,
177.642339485944));
#28597=CARTESIAN_POINT('Ctrl Pts',(-60.7754659560919,-102.946768948967,
178.813912312176));
#28598=CARTESIAN_POINT('Ctrl Pts',(-59.6005562086583,-102.977740948934,
179.985485138407));
#28599=CARTESIAN_POINT('Ctrl Pts',(-57.9430994586544,-103.06015568322,179.985485069079));
#28600=CARTESIAN_POINT('Ctrl Pts',(-56.2856427086505,-103.142570417507,
179.985484999752));
#28601=CARTESIAN_POINT('Ctrl Pts',(-55.1107330587087,-103.17354240708,178.813912075476));
#28602=CARTESIAN_POINT('Ctrl Pts',(-53.935823408767,-103.204514396654,177.6423391512));
#28603=CARTESIAN_POINT('Ctrl Pts',(-53.9258854147871,-103.111292624649,
175.985484901707));
#28604=CARTESIAN_POINT('Ctrl Pts',(-53.9159474208072,-103.018070852645,
174.328630652215));
#28605=CARTESIAN_POINT('Ctrl Pts',(-55.0709810424069,-102.800655323367,
173.157057825983));
#28606=CARTESIAN_POINT('Ctrl Pts',(-56.2260146640065,-102.58323979409,171.985484999752));
#28607=CARTESIAN_POINT('Ctrl Pts',(-57.8635952881763,-102.314381530493,
171.985485069079));
#28608=CARTESIAN_POINT('Ctrl Pts',(-59.5011759123462,-102.045523266896,
171.985485138407));
#28609=CARTESIAN_POINT('Ctrl Pts',(-60.6562094364539,-101.828107748012,
173.157058062683));
#28610=CARTESIAN_POINT('Ctrl Pts',(-61.8112429605617,-101.610692229127,
174.328630986959));
#28611=CARTESIAN_POINT('Ctrl Pts',(-61.8013048287075,-101.517470471821,
175.985485236451));
#28612=CARTESIAN_POINT('Ctrl Pts',(-61.7913666968533,-101.424248714515,
177.642339485944));
#28613=CARTESIAN_POINT('Ctrl Pts',(-60.6164569494197,-101.455220714482,
178.813912312176));
#28614=CARTESIAN_POINT('Ctrl Pts',(-59.4415472019861,-101.486192714449,
179.985485138407));
#28615=CARTESIAN_POINT('Ctrl Pts',(-57.7840904519822,-101.568607448735,
179.985485069079));
#28616=CARTESIAN_POINT('Ctrl Pts',(-56.1266337019783,-101.651022183021,
179.985484999752));
#28617=CARTESIAN_POINT('Ctrl Pts',(-54.9517240520365,-101.681994172595,
178.813912075476));
#28618=CARTESIAN_POINT('Ctrl Pts',(-53.7768144020947,-101.712966162168,
177.6423391512));
#28619=CARTESIAN_POINT('Ctrl Pts',(-53.7668764081149,-101.619744390164,
175.985484901707));
#28620=CARTESIAN_POINT('Ctrl Pts',(-53.756938414135,-101.526522618159,174.328630652215));
#28621=CARTESIAN_POINT('Ctrl Pts',(-54.9119720357346,-101.309107088882,
173.157057825983));
#28622=CARTESIAN_POINT('Ctrl Pts',(-56.0670056573342,-101.091691559604,
171.985484999752));
#28623=CARTESIAN_POINT('Ctrl Pts',(-57.7045862815041,-100.822833296007,
171.985485069079));
#28624=CARTESIAN_POINT('Ctrl Pts',(-59.342166905674,-100.55397503241,171.985485138407));
#28625=CARTESIAN_POINT('Ctrl Pts',(-60.4972004297817,-100.336559513526,
173.157058062683));
#28626=CARTESIAN_POINT('Ctrl Pts',(-61.6522339538895,-100.119143994642,
174.328630986959));
#28627=CARTESIAN_POINT('Ctrl Pts',(-61.6422958220353,-100.025922237336,
175.985485236451));
#28628=CARTESIAN_POINT('Ctrl Pts',(-61.6323576901811,-99.9327004800294,
177.642339485944));
#28629=CARTESIAN_POINT('Ctrl Pts',(-60.4574479427475,-99.9636724799962,
178.813912312176));
#28630=CARTESIAN_POINT('Ctrl Pts',(-59.2825381953138,-99.994644479963,179.985485138407));
#28631=CARTESIAN_POINT('Ctrl Pts',(-57.6250814453099,-100.077059214249,
179.985485069079));
#28632=CARTESIAN_POINT('Ctrl Pts',(-55.9676246953061,-100.159473948536,
179.985484999752));
#28633=CARTESIAN_POINT('Ctrl Pts',(-54.7927150453643,-100.190445938109,
178.813912075476));
#28634=CARTESIAN_POINT('Ctrl Pts',(-53.6178053954225,-100.221417927683,
177.6423391512));
#28635=CARTESIAN_POINT('Ctrl Pts',(-53.6078674014426,-100.128196155678,
175.985484901707));
#28636=CARTESIAN_POINT('Ctrl Pts',(-53.5979294074628,-100.034974383673,
174.328630652215));
#28637=CARTESIAN_POINT('Ctrl Pts',(-54.7529630290624,-99.817558854396,173.157057825983));
#28638=CARTESIAN_POINT('Ctrl Pts',(-55.907996650662,-99.6001433251185,171.985484999752));
#28639=CARTESIAN_POINT('Ctrl Pts',(-57.5455772748319,-99.3312850615215,
171.985485069079));
#28640=CARTESIAN_POINT('Ctrl Pts',(-59.1831578990017,-99.0624267979246,
171.985485138407));
#28641=CARTESIAN_POINT('Ctrl Pts',(-60.3381914231095,-98.8450112790404,
173.157058062683));
#28642=CARTESIAN_POINT('Ctrl Pts',(-61.4932249472172,-98.6275957601562,
174.328630986959));
#28643=CARTESIAN_POINT('Ctrl Pts',(-61.4832868153631,-98.53437400285,175.985485236451));
#28644=CARTESIAN_POINT('Ctrl Pts',(-61.4733486835089,-98.4411522455438,
177.642339485944));
#28645=CARTESIAN_POINT('Ctrl Pts',(-60.2984389360752,-98.4721242455106,
178.813912312176));
#28646=CARTESIAN_POINT('Ctrl Pts',(-59.1235291886416,-98.5030962454774,
179.985485138407));
#28647=CARTESIAN_POINT('Ctrl Pts',(-57.4660724386377,-98.5855109797636,
179.985485069079));
#28648=CARTESIAN_POINT('Ctrl Pts',(-55.8086156886338,-98.6679257140499,
179.985484999752));
#28649=CARTESIAN_POINT('Ctrl Pts',(-54.633706038692,-98.6988977036234,178.813912075476));
#28650=CARTESIAN_POINT('Ctrl Pts',(-56.2237961054143,-113.614380048479,
178.813912075476));
#28651=CARTESIAN_POINT('Ctrl Pts',(-55.0488864554725,-113.645352038053,
177.6423391512));
#28652=CARTESIAN_POINT('Ctrl Pts',(-55.0389484614927,-113.552130266048,
175.985484901707));
#28653=CARTESIAN_POINT('Ctrl Pts',(-55.0290104675128,-113.458908494044,
174.328630652215));
#28654=CARTESIAN_POINT('Ctrl Pts',(-56.1840440891124,-113.241492964766,
173.157057825983));
#28655=CARTESIAN_POINT('Ctrl Pts',(-57.3390777107121,-113.024077435489,
171.985484999752));
#28656=CARTESIAN_POINT('Ctrl Pts',(-58.9766583348819,-112.755219171892,
171.985485069079));
#28657=CARTESIAN_POINT('Ctrl Pts',(-60.6142389590518,-112.486360908295,
171.985485138407));
#28658=CARTESIAN_POINT('Ctrl Pts',(-61.7692724831595,-112.268945389411,
173.157058062683));
#28659=CARTESIAN_POINT('Ctrl Pts',(-62.9243060072673,-112.051529870527,
174.328630986959));
#28660=CARTESIAN_POINT('Ctrl Pts',(-62.9143678754131,-111.95830811322,175.985485236451));
#28661=CARTESIAN_POINT('Ctrl Pts',(-62.9044297435589,-111.865086355914,
177.642339485944));
#28662=CARTESIAN_POINT('Ctrl Pts',(-61.7295199961253,-111.896058355881,
178.813912312176));
#28663=CARTESIAN_POINT('Ctrl Pts',(-60.5546102486917,-111.927030355848,
179.985485138407));
#28664=CARTESIAN_POINT('Ctrl Pts',(-58.8971534986878,-112.009445090134,
179.985485069079));
#28665=CARTESIAN_POINT('Ctrl Pts',(-57.2396967486839,-112.09185982442,179.985484999752));
#28666=CARTESIAN_POINT('Ctrl Pts',(-56.0647870987421,-112.122831813994,
178.813912075476));
#28667=CARTESIAN_POINT('Ctrl Pts',(-54.8898774488003,-112.153803803567,
177.6423391512));
#28668=CARTESIAN_POINT('Ctrl Pts',(-54.8799394548205,-112.060582031563,
175.985484901707));
#28669=CARTESIAN_POINT('Ctrl Pts',(-54.8700014608406,-111.967360259558,
174.328630652215));
#28670=CARTESIAN_POINT('Ctrl Pts',(-56.0250350824402,-111.749944730281,
173.157057825983));
#28671=CARTESIAN_POINT('Ctrl Pts',(-57.1800687040398,-111.532529201003,
171.985484999752));
#28672=CARTESIAN_POINT('Ctrl Pts',(-58.8176493282097,-111.263670937406,
171.985485069079));
#28673=CARTESIAN_POINT('Ctrl Pts',(-60.4552299523796,-110.994812673809,
171.985485138407));
#28674=CARTESIAN_POINT('Ctrl Pts',(-61.6102634764873,-110.777397154925,
173.157058062683));
#28675=CARTESIAN_POINT('Ctrl Pts',(-62.7652970005951,-110.559981636041,
174.328630986959));
#28676=CARTESIAN_POINT('Ctrl Pts',(-62.7553588687409,-110.466759878735,
175.985485236451));
#28677=CARTESIAN_POINT('Ctrl Pts',(-62.7454207368867,-110.373538121429,
177.642339485944));
#28678=CARTESIAN_POINT('Ctrl Pts',(-61.5705109894531,-110.404510121395,
178.813912312176));
#28679=CARTESIAN_POINT('Ctrl Pts',(-60.3956012420194,-110.435482121362,
179.985485138407));
#28680=CARTESIAN_POINT('Ctrl Pts',(-58.7381444920155,-110.517896855648,
179.985485069079));
#28681=CARTESIAN_POINT('Ctrl Pts',(-57.0806877420116,-110.600311589935,
179.985484999752));
#28682=CARTESIAN_POINT('Ctrl Pts',(-55.9057780920699,-110.631283579508,
178.813912075476));
#28683=CARTESIAN_POINT('Ctrl Pts',(-54.7308684421281,-110.662255569082,
177.6423391512));
#28684=CARTESIAN_POINT('Ctrl Pts',(-54.7209304481482,-110.569033797077,
175.985484901707));
#28685=CARTESIAN_POINT('Ctrl Pts',(-54.7109924541684,-110.475812025073,
174.328630652215));
#28686=CARTESIAN_POINT('Ctrl Pts',(-55.866026075768,-110.258396495795,173.157057825983));
#28687=CARTESIAN_POINT('Ctrl Pts',(-57.0210596973676,-110.040980966518,
171.985484999752));
#28688=CARTESIAN_POINT('Ctrl Pts',(-58.6586403215375,-109.772122702921,
171.985485069079));
#28689=CARTESIAN_POINT('Ctrl Pts',(-60.2962209457073,-109.503264439324,
171.985485138407));
#28690=CARTESIAN_POINT('Ctrl Pts',(-61.4512544698151,-109.28584892044,173.157058062683));
#28691=CARTESIAN_POINT('Ctrl Pts',(-62.6062879939228,-109.068433401555,
174.328630986959));
#28692=CARTESIAN_POINT('Ctrl Pts',(-62.5963498620687,-108.975211644249,
175.985485236451));
#28693=CARTESIAN_POINT('Ctrl Pts',(-62.5864117302145,-108.881989886943,
177.642339485944));
#28694=CARTESIAN_POINT('Ctrl Pts',(-61.4115019827808,-108.91296188691,178.813912312176));
#28695=CARTESIAN_POINT('Ctrl Pts',(-60.2365922353472,-108.943933886877,
179.985485138407));
#28696=CARTESIAN_POINT('Ctrl Pts',(-58.5791354853433,-109.026348621163,
179.985485069079));
#28697=CARTESIAN_POINT('Ctrl Pts',(-56.9216787353394,-109.108763355449,
179.985484999752));
#28698=CARTESIAN_POINT('Ctrl Pts',(-55.7467690853976,-109.139735345023,
178.813912075476));
#28699=CARTESIAN_POINT('Ctrl Pts',(-54.5718594354559,-109.170707334596,
177.6423391512));
#28700=CARTESIAN_POINT('Ctrl Pts',(-54.561921441476,-109.077485562592,175.985484901707));
#28701=CARTESIAN_POINT('Ctrl Pts',(-54.5519834474962,-108.984263790587,
174.328630652215));
#28702=CARTESIAN_POINT('Ctrl Pts',(-55.7070170690958,-108.76684826131,173.157057825983));
#28703=CARTESIAN_POINT('Ctrl Pts',(-56.8620506906954,-108.549432732032,
171.985484999752));
#28704=CARTESIAN_POINT('Ctrl Pts',(-58.4996313148652,-108.280574468435,
171.985485069079));
#28705=CARTESIAN_POINT('Ctrl Pts',(-60.1372119390351,-108.011716204838,
171.985485138407));
#28706=CARTESIAN_POINT('Ctrl Pts',(-61.2922454631428,-107.794300685954,
173.157058062683));
#28707=CARTESIAN_POINT('Ctrl Pts',(-62.4472789872506,-107.57688516707,174.328630986959));
#28708=CARTESIAN_POINT('Ctrl Pts',(-62.4373408553964,-107.483663409764,
175.985485236451));
#28709=CARTESIAN_POINT('Ctrl Pts',(-62.4274027235423,-107.390441652457,
177.642339485944));
#28710=CARTESIAN_POINT('Ctrl Pts',(-61.2524929761086,-107.421413652424,
178.813912312176));
#28711=CARTESIAN_POINT('Ctrl Pts',(-60.077583228675,-107.452385652391,179.985485138407));
#28712=CARTESIAN_POINT('Ctrl Pts',(-58.4201264786711,-107.534800386677,
179.985485069079));
#28713=CARTESIAN_POINT('Ctrl Pts',(-56.7626697286672,-107.617215120964,
179.985484999752));
#28714=CARTESIAN_POINT('Ctrl Pts',(-55.5877600787254,-107.648187110537,
178.813912075476));
#28715=CARTESIAN_POINT('Ctrl Pts',(-54.4128504287836,-107.67915910011,177.6423391512));
#28716=CARTESIAN_POINT('Ctrl Pts',(-54.4029124348038,-107.585937328106,
175.985484901707));
#28717=CARTESIAN_POINT('Ctrl Pts',(-54.3929744408239,-107.492715556102,
174.328630652215));
#28718=CARTESIAN_POINT('Ctrl Pts',(-55.5480080624235,-107.275300026824,
173.157057825983));
#28719=CARTESIAN_POINT('Ctrl Pts',(-56.7030416840231,-107.057884497547,
171.985484999752));
#28720=CARTESIAN_POINT('Ctrl Pts',(-58.340622308193,-106.78902623395,171.985485069079));
#28721=CARTESIAN_POINT('Ctrl Pts',(-59.9782029323629,-106.520167970353,
171.985485138407));
#28722=CARTESIAN_POINT('Ctrl Pts',(-61.1332364564706,-106.302752451468,
173.157058062683));
#28723=CARTESIAN_POINT('Ctrl Pts',(-62.2882699805784,-106.085336932584,
174.328630986959));
#28724=CARTESIAN_POINT('Ctrl Pts',(-62.2783318487242,-105.992115175278,
175.985485236451));
#28725=CARTESIAN_POINT('Ctrl Pts',(-62.26839371687,-105.898893417972,177.642339485944));
#28726=CARTESIAN_POINT('Ctrl Pts',(-61.0934839694364,-105.929865417939,
178.813912312176));
#28727=CARTESIAN_POINT('Ctrl Pts',(-59.9185742220028,-105.960837417905,
179.985485138407));
#28728=CARTESIAN_POINT('Ctrl Pts',(-58.2611174719989,-106.043252152192,
179.985485069079));
#28729=CARTESIAN_POINT('Ctrl Pts',(-56.603660721995,-106.125666886478,179.985484999752));
#28730=CARTESIAN_POINT('Ctrl Pts',(-55.4287510720532,-106.156638876051,
178.813912075476));
#28731=CARTESIAN_POINT('Ctrl Pts',(-54.2538414221114,-106.187610865625,
177.6423391512));
#28732=CARTESIAN_POINT('Ctrl Pts',(-54.2439034281315,-106.09438909362,175.985484901707));
#28733=CARTESIAN_POINT('Ctrl Pts',(-54.2339654341517,-106.001167321616,
174.328630652215));
#28734=CARTESIAN_POINT('Ctrl Pts',(-55.3889990557513,-105.783751792338,
173.157057825983));
#28735=CARTESIAN_POINT('Ctrl Pts',(-56.5440326773509,-105.566336263061,
171.985484999752));
#28736=CARTESIAN_POINT('Ctrl Pts',(-58.1816133015208,-105.297477999464,
171.985485069079));
#28737=CARTESIAN_POINT('Ctrl Pts',(-59.8191939256906,-105.028619735867,
171.985485138407));
#28738=CARTESIAN_POINT('Ctrl Pts',(-60.9742274497984,-104.811204216983,
173.157058062683));
#28739=CARTESIAN_POINT('Ctrl Pts',(-62.1292609739061,-104.593788698099,
174.328630986959));
#28740=CARTESIAN_POINT('Ctrl Pts',(-62.119322842052,-104.500566940792,175.985485236451));
#28741=CARTESIAN_POINT('Ctrl Pts',(-62.1093847101978,-104.407345183486,
177.642339485944));
#28742=CARTESIAN_POINT('Ctrl Pts',(-60.9344749627642,-104.438317183453,
178.813912312176));
#28743=CARTESIAN_POINT('Ctrl Pts',(-59.7595652153305,-104.46928918342,179.985485138407));
#28744=CARTESIAN_POINT('Ctrl Pts',(-58.1021084653266,-104.551703917706,
179.985485069079));
#28745=CARTESIAN_POINT('Ctrl Pts',(-56.4446517153227,-104.634118651992,
179.985484999752));
#28746=CARTESIAN_POINT('Ctrl Pts',(-55.269742065381,-104.665090641566,178.813912075476));
#28747=CARTESIAN_POINT('Ctrl Pts',(-54.0948324154392,-104.696062631139,
177.6423391512));
#28748=CARTESIAN_POINT('Ctrl Pts',(-54.0848944214593,-104.602840859135,
175.985484901707));
#28749=CARTESIAN_POINT('Ctrl Pts',(-54.0749564274795,-104.50961908713,174.328630652215));
#28750=CARTESIAN_POINT('Ctrl Pts',(-55.2299900490791,-104.292203557853,
173.157057825983));
#28751=CARTESIAN_POINT('Ctrl Pts',(-56.3850236706787,-104.074788028575,
171.985484999752));
#28752=CARTESIAN_POINT('Ctrl Pts',(-58.0226042948486,-103.805929764978,
171.985485069079));
#28753=CARTESIAN_POINT('Ctrl Pts',(-59.6601849190184,-103.537071501381,
171.985485138407));
#28754=CARTESIAN_POINT('Ctrl Pts',(-60.8152184431262,-103.319655982497,
173.157058062683));
#28755=CARTESIAN_POINT('Ctrl Pts',(-61.9702519672339,-103.102240463613,
174.328630986959));
#28756=CARTESIAN_POINT('Ctrl Pts',(-61.9603138353797,-103.009018706307,
175.985485236451));
#28757=CARTESIAN_POINT('Ctrl Pts',(-61.9503757035256,-102.915796949001,
177.642339485944));
#28758=CARTESIAN_POINT('Ctrl Pts',(-60.7754659560919,-102.946768948967,
178.813912312176));
#28759=CARTESIAN_POINT('Ctrl Pts',(-59.6005562086583,-102.977740948934,
179.985485138407));
#28760=CARTESIAN_POINT('Ctrl Pts',(-57.9430994586544,-103.06015568322,179.985485069079));
#28761=CARTESIAN_POINT('Ctrl Pts',(-56.2856427086505,-103.142570417507,
179.985484999752));
#28762=CARTESIAN_POINT('Ctrl Pts',(-55.1107330587087,-103.17354240708,178.813912075476));
#28763=CARTESIAN_POINT('Ctrl Pts',(-53.935823408767,-103.204514396654,177.6423391512));
#28764=CARTESIAN_POINT('Ctrl Pts',(-53.9258854147871,-103.111292624649,
175.985484901707));
#28765=CARTESIAN_POINT('Ctrl Pts',(-53.9159474208072,-103.018070852645,
174.328630652215));
#28766=CARTESIAN_POINT('Ctrl Pts',(-55.0709810424069,-102.800655323367,
173.157057825983));
#28767=CARTESIAN_POINT('Ctrl Pts',(-56.2260146640065,-102.58323979409,171.985484999752));
#28768=CARTESIAN_POINT('Ctrl Pts',(-57.8635952881763,-102.314381530493,
171.985485069079));
#28769=CARTESIAN_POINT('Ctrl Pts',(-59.5011759123462,-102.045523266896,
171.985485138407));
#28770=CARTESIAN_POINT('Ctrl Pts',(-60.6562094364539,-101.828107748012,
173.157058062683));
#28771=CARTESIAN_POINT('Ctrl Pts',(-61.8112429605617,-101.610692229127,
174.328630986959));
#28772=CARTESIAN_POINT('Ctrl Pts',(-61.8013048287075,-101.517470471821,
175.985485236451));
#28773=CARTESIAN_POINT('Ctrl Pts',(-61.7913666968533,-101.424248714515,
177.642339485944));
#28774=CARTESIAN_POINT('Ctrl Pts',(-60.6164569494197,-101.455220714482,
178.813912312176));
#28775=CARTESIAN_POINT('Ctrl Pts',(-59.4415472019861,-101.486192714449,
179.985485138407));
#28776=CARTESIAN_POINT('Ctrl Pts',(-57.7840904519822,-101.568607448735,
179.985485069079));
#28777=CARTESIAN_POINT('Ctrl Pts',(-56.1266337019783,-101.651022183021,
179.985484999752));
#28778=CARTESIAN_POINT('Ctrl Pts',(-54.9517240520365,-101.681994172595,
178.813912075476));
#28779=CARTESIAN_POINT('Ctrl Pts',(-53.7768144020947,-101.712966162168,
177.6423391512));
#28780=CARTESIAN_POINT('Ctrl Pts',(-53.7668764081149,-101.619744390164,
175.985484901707));
#28781=CARTESIAN_POINT('Ctrl Pts',(-53.756938414135,-101.526522618159,174.328630652215));
#28782=CARTESIAN_POINT('Ctrl Pts',(-54.9119720357346,-101.309107088882,
173.157057825983));
#28783=CARTESIAN_POINT('Ctrl Pts',(-56.0670056573342,-101.091691559604,
171.985484999752));
#28784=CARTESIAN_POINT('Ctrl Pts',(-57.7045862815041,-100.822833296007,
171.985485069079));
#28785=CARTESIAN_POINT('Ctrl Pts',(-59.342166905674,-100.55397503241,171.985485138407));
#28786=CARTESIAN_POINT('Ctrl Pts',(-60.4972004297817,-100.336559513526,
173.157058062683));
#28787=CARTESIAN_POINT('Ctrl Pts',(-61.6522339538895,-100.119143994642,
174.328630986959));
#28788=CARTESIAN_POINT('Ctrl Pts',(-61.6422958220353,-100.025922237336,
175.985485236451));
#28789=CARTESIAN_POINT('Ctrl Pts',(-61.6323576901811,-99.9327004800294,
177.642339485944));
#28790=CARTESIAN_POINT('Ctrl Pts',(-60.4574479427475,-99.9636724799962,
178.813912312176));
#28791=CARTESIAN_POINT('Ctrl Pts',(-59.2825381953138,-99.994644479963,179.985485138407));
#28792=CARTESIAN_POINT('Ctrl Pts',(-57.6250814453099,-100.077059214249,
179.985485069079));
#28793=CARTESIAN_POINT('Ctrl Pts',(-55.9676246953061,-100.159473948536,
179.985484999752));
#28794=CARTESIAN_POINT('Ctrl Pts',(-54.7927150453643,-100.190445938109,
178.813912075476));
#28795=CARTESIAN_POINT('Ctrl Pts',(-53.6178053954225,-100.221417927683,
177.6423391512));
#28796=CARTESIAN_POINT('Ctrl Pts',(-53.6078674014426,-100.128196155678,
175.985484901707));
#28797=CARTESIAN_POINT('Ctrl Pts',(-53.5979294074628,-100.034974383673,
174.328630652215));
#28798=CARTESIAN_POINT('Ctrl Pts',(-54.7529630290624,-99.817558854396,173.157057825983));
#28799=CARTESIAN_POINT('Ctrl Pts',(-55.907996650662,-99.6001433251185,171.985484999752));
#28800=CARTESIAN_POINT('Ctrl Pts',(-57.5455772748319,-99.3312850615215,
171.985485069079));
#28801=CARTESIAN_POINT('Ctrl Pts',(-59.1831578990017,-99.0624267979246,
171.985485138407));
#28802=CARTESIAN_POINT('Ctrl Pts',(-60.3381914231095,-98.8450112790404,
173.157058062683));
#28803=CARTESIAN_POINT('Ctrl Pts',(-61.4932249472172,-98.6275957601562,
174.328630986959));
#28804=CARTESIAN_POINT('Ctrl Pts',(-61.4832868153631,-98.53437400285,175.985485236451));
#28805=CARTESIAN_POINT('Ctrl Pts',(-61.4733486835089,-98.4411522455438,
177.642339485944));
#28806=CARTESIAN_POINT('Ctrl Pts',(-60.2984389360752,-98.4721242455106,
178.813912312176));
#28807=CARTESIAN_POINT('Ctrl Pts',(-59.1235291886416,-98.5030962454774,
179.985485138407));
#28808=CARTESIAN_POINT('Ctrl Pts',(-57.4660724386377,-98.5855109797636,
179.985485069079));
#28809=CARTESIAN_POINT('Ctrl Pts',(-55.8086156886338,-98.6679257140499,
179.985484999752));
#28810=CARTESIAN_POINT('Ctrl Pts',(-54.633706038692,-98.6988977036234,178.813912075476));
#28811=CARTESIAN_POINT('Ctrl Pts',(-56.9964983346804,-113.864655531781,
178.072094410988));
#28812=CARTESIAN_POINT('Ctrl Pts',(-56.1271283009022,-113.863054956993,
177.207792449865));
#28813=CARTESIAN_POINT('Ctrl Pts',(-56.117190288842,-113.769833186916,175.985484945604));
#28814=CARTESIAN_POINT('Ctrl Pts',(-56.1072522767819,-113.676611416839,
174.763177441344));
#28815=CARTESIAN_POINT('Ctrl Pts',(-56.9567462566485,-113.491768454648,
173.89887555255));
#28816=CARTESIAN_POINT('Ctrl Pts',(-57.8062402365152,-113.306925492458,
173.034573663757));
#28817=CARTESIAN_POINT('Ctrl Pts',(-59.011722573584,-113.084131793069,173.034573714903));
#28818=CARTESIAN_POINT('Ctrl Pts',(-60.2172049106529,-112.86133809368,173.034573766048));
#28819=CARTESIAN_POINT('Ctrl Pts',(-61.0666988185971,-112.676495139156,
173.898875727171));
#28820=CARTESIAN_POINT('Ctrl Pts',(-61.9161927265413,-112.491652184633,
174.763177688294));
#28821=CARTESIAN_POINT('Ctrl Pts',(-61.9062546127674,-112.398430425399,
175.985485192554));
#28822=CARTESIAN_POINT('Ctrl Pts',(-61.8963164989935,-112.305208666166,
177.207792696815));
#28823=CARTESIAN_POINT('Ctrl Pts',(-61.0269463932928,-112.303608099046,
178.072094585608));
#28824=CARTESIAN_POINT('Ctrl Pts',(-60.1575762875921,-112.302007531926,
178.936396474401));
#28825=CARTESIAN_POINT('Ctrl Pts',(-58.9322178246893,-112.338357702004,
178.936396423256));
#28826=CARTESIAN_POINT('Ctrl Pts',(-57.7068593617864,-112.374707872082,
178.936396372111));
#28827=CARTESIAN_POINT('Ctrl Pts',(-56.8374893280082,-112.373107297295,
178.072094410988));
#28828=CARTESIAN_POINT('Ctrl Pts',(-55.9681192942299,-112.371506722508,
177.207792449865));
#28829=CARTESIAN_POINT('Ctrl Pts',(-55.9581812821698,-112.278284952431,
175.985484945604));
#28830=CARTESIAN_POINT('Ctrl Pts',(-55.9482432701096,-112.185063182354,
174.763177441344));
#28831=CARTESIAN_POINT('Ctrl Pts',(-56.7977372499763,-112.000220220163,
173.89887555255));
#28832=CARTESIAN_POINT('Ctrl Pts',(-57.647231229843,-111.815377257972,173.034573663757));
#28833=CARTESIAN_POINT('Ctrl Pts',(-58.8527135669118,-111.592583558583,
173.034573714903));
#28834=CARTESIAN_POINT('Ctrl Pts',(-60.0581959039807,-111.369789859194,
173.034573766048));
#28835=CARTESIAN_POINT('Ctrl Pts',(-60.9076898119249,-111.184946904671,
173.898875727171));
#28836=CARTESIAN_POINT('Ctrl Pts',(-61.7571837198691,-111.000103950148,
174.763177688294));
#28837=CARTESIAN_POINT('Ctrl Pts',(-61.7472456060952,-110.906882190914,
175.985485192554));
#28838=CARTESIAN_POINT('Ctrl Pts',(-61.7373074923213,-110.81366043168,177.207792696815));
#28839=CARTESIAN_POINT('Ctrl Pts',(-60.8679373866206,-110.81205986456,178.072094585608));
#28840=CARTESIAN_POINT('Ctrl Pts',(-59.9985672809199,-110.81045929744,178.936396474401));
#28841=CARTESIAN_POINT('Ctrl Pts',(-58.7732088180171,-110.846809467519,
178.936396423256));
#28842=CARTESIAN_POINT('Ctrl Pts',(-57.5478503551142,-110.883159637597,
178.936396372111));
#28843=CARTESIAN_POINT('Ctrl Pts',(-56.6784803213359,-110.881559062809,
178.072094410988));
#28844=CARTESIAN_POINT('Ctrl Pts',(-55.8091102875577,-110.879958488022,
177.207792449865));
#28845=CARTESIAN_POINT('Ctrl Pts',(-55.7991722754976,-110.786736717945,
175.985484945604));
#28846=CARTESIAN_POINT('Ctrl Pts',(-55.7892342634374,-110.693514947868,
174.763177441344));
#28847=CARTESIAN_POINT('Ctrl Pts',(-56.6387282433041,-110.508671985677,
173.89887555255));
#28848=CARTESIAN_POINT('Ctrl Pts',(-57.4882222231708,-110.323829023487,
173.034573663757));
#28849=CARTESIAN_POINT('Ctrl Pts',(-58.6937045602396,-110.101035324098,
173.034573714903));
#28850=CARTESIAN_POINT('Ctrl Pts',(-59.8991868973084,-109.878241624709,
173.034573766048));
#28851=CARTESIAN_POINT('Ctrl Pts',(-60.7486808052526,-109.693398670185,
173.898875727171));
#28852=CARTESIAN_POINT('Ctrl Pts',(-61.5981747131968,-109.508555715662,
174.763177688294));
#28853=CARTESIAN_POINT('Ctrl Pts',(-61.588236599423,-109.415333956428,175.985485192554));
#28854=CARTESIAN_POINT('Ctrl Pts',(-61.5782984856491,-109.322112197195,
177.207792696815));
#28855=CARTESIAN_POINT('Ctrl Pts',(-60.7089283799484,-109.320511630075,
178.072094585608));
#28856=CARTESIAN_POINT('Ctrl Pts',(-59.8395582742477,-109.318911062955,
178.936396474401));
#28857=CARTESIAN_POINT('Ctrl Pts',(-58.6141998113448,-109.355261233033,
178.936396423256));
#28858=CARTESIAN_POINT('Ctrl Pts',(-57.388841348442,-109.391611403111,178.936396372111));
#28859=CARTESIAN_POINT('Ctrl Pts',(-56.5194713146637,-109.390010828324,
178.072094410988));
#28860=CARTESIAN_POINT('Ctrl Pts',(-55.6501012808855,-109.388410253536,
177.207792449865));
#28861=CARTESIAN_POINT('Ctrl Pts',(-55.6401632688253,-109.295188483459,
175.985484945604));
#28862=CARTESIAN_POINT('Ctrl Pts',(-55.6302252567652,-109.201966713382,
174.763177441344));
#28863=CARTESIAN_POINT('Ctrl Pts',(-56.4797192366319,-109.017123751192,
173.89887555255));
#28864=CARTESIAN_POINT('Ctrl Pts',(-57.3292132164985,-108.832280789001,
173.034573663757));
#28865=CARTESIAN_POINT('Ctrl Pts',(-58.5346955535674,-108.609487089612,
173.034573714903));
#28866=CARTESIAN_POINT('Ctrl Pts',(-59.7401778906362,-108.386693390223,
173.034573766048));
#28867=CARTESIAN_POINT('Ctrl Pts',(-60.5896717985804,-108.2018504357,173.898875727171));
#28868=CARTESIAN_POINT('Ctrl Pts',(-61.4391657065246,-108.017007481176,
174.763177688294));
#28869=CARTESIAN_POINT('Ctrl Pts',(-61.4292275927507,-107.923785721943,
175.985485192554));
#28870=CARTESIAN_POINT('Ctrl Pts',(-61.4192894789769,-107.830563962709,
177.207792696815));
#28871=CARTESIAN_POINT('Ctrl Pts',(-60.5499193732762,-107.828963395589,
178.072094585608));
#28872=CARTESIAN_POINT('Ctrl Pts',(-59.6805492675755,-107.827362828469,
178.936396474401));
#28873=CARTESIAN_POINT('Ctrl Pts',(-58.4551908046726,-107.863712998547,
178.936396423256));
#28874=CARTESIAN_POINT('Ctrl Pts',(-57.2298323417698,-107.900063168626,
178.936396372111));
#28875=CARTESIAN_POINT('Ctrl Pts',(-56.3604623079915,-107.898462593838,
178.072094410988));
#28876=CARTESIAN_POINT('Ctrl Pts',(-55.4910922742133,-107.896862019051,
177.207792449865));
#28877=CARTESIAN_POINT('Ctrl Pts',(-55.4811542621531,-107.803640248974,
175.985484945604));
#28878=CARTESIAN_POINT('Ctrl Pts',(-55.471216250093,-107.710418478897,174.763177441344));
#28879=CARTESIAN_POINT('Ctrl Pts',(-56.3207102299596,-107.525575516706,
173.89887555255));
#28880=CARTESIAN_POINT('Ctrl Pts',(-57.1702042098263,-107.340732554515,
173.034573663757));
#28881=CARTESIAN_POINT('Ctrl Pts',(-58.3756865468951,-107.117938855126,
173.034573714903));
#28882=CARTESIAN_POINT('Ctrl Pts',(-59.581168883964,-106.895145155737,173.034573766048));
#28883=CARTESIAN_POINT('Ctrl Pts',(-60.4306627919082,-106.710302201214,
173.898875727171));
#28884=CARTESIAN_POINT('Ctrl Pts',(-61.2801566998524,-106.525459246691,
174.763177688294));
#28885=CARTESIAN_POINT('Ctrl Pts',(-61.2702185860785,-106.432237487457,
175.985485192554));
#28886=CARTESIAN_POINT('Ctrl Pts',(-61.2602804723046,-106.339015728223,
177.207792696815));
#28887=CARTESIAN_POINT('Ctrl Pts',(-60.3909103666039,-106.337415161103,
178.072094585608));
#28888=CARTESIAN_POINT('Ctrl Pts',(-59.5215402609032,-106.335814593983,
178.936396474401));
#28889=CARTESIAN_POINT('Ctrl Pts',(-58.2961817980004,-106.372164764062,
178.936396423256));
#28890=CARTESIAN_POINT('Ctrl Pts',(-57.0708233350975,-106.40851493414,178.936396372111));
#28891=CARTESIAN_POINT('Ctrl Pts',(-56.2014533013193,-106.406914359353,
178.072094410988));
#28892=CARTESIAN_POINT('Ctrl Pts',(-55.332083267541,-106.405313784565,177.207792449865));
#28893=CARTESIAN_POINT('Ctrl Pts',(-55.3221452554809,-106.312092014488,
175.985484945604));
#28894=CARTESIAN_POINT('Ctrl Pts',(-55.3122072434207,-106.218870244411,
174.763177441344));
#28895=CARTESIAN_POINT('Ctrl Pts',(-56.1617012232874,-106.034027282221,
173.89887555255));
#28896=CARTESIAN_POINT('Ctrl Pts',(-57.0111952031541,-105.84918432003,173.034573663757));
#28897=CARTESIAN_POINT('Ctrl Pts',(-58.2166775402229,-105.626390620641,
173.034573714903));
#28898=CARTESIAN_POINT('Ctrl Pts',(-59.4221598772917,-105.403596921252,
173.034573766048));
#28899=CARTESIAN_POINT('Ctrl Pts',(-60.2716537852359,-105.218753966728,
173.898875727171));
#28900=CARTESIAN_POINT('Ctrl Pts',(-61.1211476931802,-105.033911012205,
174.763177688294));
#28901=CARTESIAN_POINT('Ctrl Pts',(-61.1112095794063,-104.940689252971,
175.985485192554));
#28902=CARTESIAN_POINT('Ctrl Pts',(-61.1012714656324,-104.847467493738,
177.207792696815));
#28903=CARTESIAN_POINT('Ctrl Pts',(-60.2319013599317,-104.845866926618,
178.072094585608));
#28904=CARTESIAN_POINT('Ctrl Pts',(-59.362531254231,-104.844266359498,178.936396474401));
#28905=CARTESIAN_POINT('Ctrl Pts',(-58.1371727913281,-104.880616529576,
178.936396423256));
#28906=CARTESIAN_POINT('Ctrl Pts',(-56.9118143284253,-104.916966699654,
178.936396372111));
#28907=CARTESIAN_POINT('Ctrl Pts',(-56.042444294647,-104.915366124867,178.072094410988));
#28908=CARTESIAN_POINT('Ctrl Pts',(-55.1730742608688,-104.91376555008,177.207792449865));
#28909=CARTESIAN_POINT('Ctrl Pts',(-55.1631362488087,-104.820543780003,
175.985484945604));
#28910=CARTESIAN_POINT('Ctrl Pts',(-55.1531982367485,-104.727322009926,
174.763177441344));
#28911=CARTESIAN_POINT('Ctrl Pts',(-56.0026922166152,-104.542479047735,
173.89887555255));
#28912=CARTESIAN_POINT('Ctrl Pts',(-56.8521861964818,-104.357636085544,
173.034573663757));
#28913=CARTESIAN_POINT('Ctrl Pts',(-58.0576685335507,-104.134842386155,
173.034573714903));
#28914=CARTESIAN_POINT('Ctrl Pts',(-59.2631508706195,-103.912048686766,
173.034573766048));
#28915=CARTESIAN_POINT('Ctrl Pts',(-60.1126447785637,-103.727205732243,
173.898875727171));
#28916=CARTESIAN_POINT('Ctrl Pts',(-60.9621386865079,-103.54236277772,174.763177688294));
#28917=CARTESIAN_POINT('Ctrl Pts',(-60.952200572734,-103.449141018486,175.985485192554));
#28918=CARTESIAN_POINT('Ctrl Pts',(-60.9422624589602,-103.355919259252,
177.207792696815));
#28919=CARTESIAN_POINT('Ctrl Pts',(-60.0728923532595,-103.354318692132,
178.072094585608));
#28920=CARTESIAN_POINT('Ctrl Pts',(-59.2035222475588,-103.352718125012,
178.936396474401));
#28921=CARTESIAN_POINT('Ctrl Pts',(-57.9781637846559,-103.389068295091,
178.936396423256));
#28922=CARTESIAN_POINT('Ctrl Pts',(-56.7528053217531,-103.425418465169,
178.936396372111));
#28923=CARTESIAN_POINT('Ctrl Pts',(-55.8834352879748,-103.423817890381,
178.072094410988));
#28924=CARTESIAN_POINT('Ctrl Pts',(-55.0140652541966,-103.422217315594,
177.207792449865));
#28925=CARTESIAN_POINT('Ctrl Pts',(-55.0041272421364,-103.328995545517,
175.985484945604));
#28926=CARTESIAN_POINT('Ctrl Pts',(-54.9941892300763,-103.23577377544,174.763177441344));
#28927=CARTESIAN_POINT('Ctrl Pts',(-55.8436832099429,-103.050930813249,
173.89887555255));
#28928=CARTESIAN_POINT('Ctrl Pts',(-56.6931771898096,-102.866087851059,
173.034573663757));
#28929=CARTESIAN_POINT('Ctrl Pts',(-57.8986595268784,-102.64329415167,173.034573714903));
#28930=CARTESIAN_POINT('Ctrl Pts',(-59.1041418639473,-102.420500452281,
173.034573766048));
#28931=CARTESIAN_POINT('Ctrl Pts',(-59.9536357718915,-102.235657497757,
173.898875727171));
#28932=CARTESIAN_POINT('Ctrl Pts',(-60.8031296798357,-102.050814543234,
174.763177688294));
#28933=CARTESIAN_POINT('Ctrl Pts',(-60.7931915660618,-101.957592784,175.985485192554));
#28934=CARTESIAN_POINT('Ctrl Pts',(-60.783253452288,-101.864371024767,177.207792696815));
#28935=CARTESIAN_POINT('Ctrl Pts',(-59.9138833465873,-101.862770457647,
178.072094585608));
#28936=CARTESIAN_POINT('Ctrl Pts',(-59.0445132408866,-101.861169890527,
178.936396474401));
#28937=CARTESIAN_POINT('Ctrl Pts',(-57.8191547779837,-101.897520060605,
178.936396423256));
#28938=CARTESIAN_POINT('Ctrl Pts',(-56.5937963150808,-101.933870230683,
178.936396372111));
#28939=CARTESIAN_POINT('Ctrl Pts',(-55.7244262813026,-101.932269655896,
178.072094410988));
#28940=CARTESIAN_POINT('Ctrl Pts',(-54.8550562475244,-101.930669081108,
177.207792449865));
#28941=CARTESIAN_POINT('Ctrl Pts',(-54.8451182354642,-101.837447311031,
175.985484945604));
#28942=CARTESIAN_POINT('Ctrl Pts',(-54.8351802234041,-101.744225540954,
174.763177441344));
#28943=CARTESIAN_POINT('Ctrl Pts',(-55.6846742032707,-101.559382578764,
173.89887555255));
#28944=CARTESIAN_POINT('Ctrl Pts',(-56.5341681831374,-101.374539616573,
173.034573663757));
#28945=CARTESIAN_POINT('Ctrl Pts',(-57.7396505202062,-101.151745917184,
173.034573714903));
#28946=CARTESIAN_POINT('Ctrl Pts',(-58.9451328572751,-100.928952217795,
173.034573766048));
#28947=CARTESIAN_POINT('Ctrl Pts',(-59.7946267652193,-100.744109263272,
173.898875727171));
#28948=CARTESIAN_POINT('Ctrl Pts',(-60.6441206731635,-100.559266308748,
174.763177688294));
#28949=CARTESIAN_POINT('Ctrl Pts',(-60.6341825593896,-100.466044549515,
175.985485192554));
#28950=CARTESIAN_POINT('Ctrl Pts',(-60.6242444456157,-100.372822790281,
177.207792696815));
#28951=CARTESIAN_POINT('Ctrl Pts',(-59.754874339915,-100.371222223161,178.072094585608));
#28952=CARTESIAN_POINT('Ctrl Pts',(-58.8855042342143,-100.369621656041,
178.936396474401));
#28953=CARTESIAN_POINT('Ctrl Pts',(-57.6601457713115,-100.405971826119,
178.936396423256));
#28954=CARTESIAN_POINT('Ctrl Pts',(-56.4347873084086,-100.442321996198,
178.936396372111));
#28955=CARTESIAN_POINT('Ctrl Pts',(-55.5654172746304,-100.44072142141,178.072094410988));
#28956=CARTESIAN_POINT('Ctrl Pts',(-54.6960472408521,-100.439120846623,
177.207792449865));
#28957=CARTESIAN_POINT('Ctrl Pts',(-54.686109228792,-100.345899076546,175.985484945604));
#28958=CARTESIAN_POINT('Ctrl Pts',(-54.6761712167318,-100.252677306469,
174.763177441344));
#28959=CARTESIAN_POINT('Ctrl Pts',(-55.5256651965985,-100.067834344278,
173.89887555255));
#28960=CARTESIAN_POINT('Ctrl Pts',(-56.3751591764652,-99.8829913820874,
173.034573663757));
#28961=CARTESIAN_POINT('Ctrl Pts',(-57.580641513534,-99.6601976826983,173.034573714903));
#28962=CARTESIAN_POINT('Ctrl Pts',(-58.7861238506028,-99.4374039833093,
173.034573766048));
#28963=CARTESIAN_POINT('Ctrl Pts',(-59.635617758547,-99.252561028786,173.898875727171));
#28964=CARTESIAN_POINT('Ctrl Pts',(-60.4851116664912,-99.0677180742627,
174.763177688294));
#28965=CARTESIAN_POINT('Ctrl Pts',(-60.4751735527174,-98.9744963150291,
175.985485192554));
#28966=CARTESIAN_POINT('Ctrl Pts',(-60.4652354389435,-98.8812745557954,
177.207792696815));
#28967=CARTESIAN_POINT('Ctrl Pts',(-59.5958653332428,-98.8796739886754,
178.072094585608));
#28968=CARTESIAN_POINT('Ctrl Pts',(-58.7264952275421,-98.8780734215554,
178.936396474401));
#28969=CARTESIAN_POINT('Ctrl Pts',(-57.5011367646392,-98.9144235916337,
178.936396423256));
#28970=CARTESIAN_POINT('Ctrl Pts',(-56.2757783017364,-98.9507737617121,
178.936396372111));
#28971=CARTESIAN_POINT('Ctrl Pts',(-55.4064082679581,-98.9491731869247,
178.072094410988));
#28972=CARTESIAN_POINT('Ctrl Pts',(-61.3885995934693,-105.924024231779,
178.485485069079));
#28973=CARTESIAN_POINT('Ctrl Pts',(-61.2500273891125,-105.925738749657,
178.657813499464));
#28974=CARTESIAN_POINT('Ctrl Pts',(-61.0934839694364,-105.929865417939,
178.813912312176));
#28975=CARTESIAN_POINT('Ctrl Pts',(-59.9185742220028,-105.960837417905,
179.985485138407));
#28976=CARTESIAN_POINT('Ctrl Pts',(-58.2611174719989,-106.043252152192,
179.985485069079));
#28977=CARTESIAN_POINT('Ctrl Pts',(-56.603660721995,-106.125666886478,179.985484999752));
#28978=CARTESIAN_POINT('Ctrl Pts',(-55.4287510720532,-106.156638876051,
178.813912075476));
#28979=CARTESIAN_POINT('Ctrl Pts',(-54.2538414221114,-106.187610865625,
177.6423391512));
#28980=CARTESIAN_POINT('Ctrl Pts',(-54.2439034281315,-106.09438909362,175.985484901707));
#28981=CARTESIAN_POINT('Ctrl Pts',(-54.2339654341517,-106.001167321616,
174.328630652215));
#28982=CARTESIAN_POINT('Ctrl Pts',(-55.3889990557513,-105.783751792338,
173.157057825983));
#28983=CARTESIAN_POINT('Ctrl Pts',(-56.5440326773509,-105.566336263061,
171.985484999752));
#28984=CARTESIAN_POINT('Ctrl Pts',(-58.1816133015208,-105.297477999464,
171.985485069079));
#28985=CARTESIAN_POINT('Ctrl Pts',(-59.8191939256906,-105.028619735867,
171.985485138407));
#28986=CARTESIAN_POINT('Ctrl Pts',(-60.9742274497984,-104.811204216983,
173.157058062683));
#28987=CARTESIAN_POINT('Ctrl Pts',(-61.1281224707516,-104.78223608304,173.313156769748));
#28988=CARTESIAN_POINT('Ctrl Pts',(-61.2639416747223,-104.754698653858,
173.485485069079));
#28989=CARTESIAN_POINT('Ctrl Pts',(-56.8733667677527,-112.709647553905,
178.072094410988));
#28990=CARTESIAN_POINT('Ctrl Pts',(-56.0039967339745,-112.708046979118,
177.207792449865));
#28991=CARTESIAN_POINT('Ctrl Pts',(-55.9940587219143,-112.614825209041,
175.985484945604));
#28992=CARTESIAN_POINT('Ctrl Pts',(-55.9841207098542,-112.521603438964,
174.763177441344));
#28993=CARTESIAN_POINT('Ctrl Pts',(-56.8336146897208,-112.336760476773,
173.89887555255));
#28994=CARTESIAN_POINT('Ctrl Pts',(-57.6831086695875,-112.151917514582,
173.034573663757));
#28995=CARTESIAN_POINT('Ctrl Pts',(-58.8885910066563,-111.929123815193,
173.034573714903));
#28996=CARTESIAN_POINT('Ctrl Pts',(-60.0940733437252,-111.706330115804,
173.034573766048));
#28997=CARTESIAN_POINT('Ctrl Pts',(-60.9435672516694,-111.521487161281,
173.898875727171));
#28998=CARTESIAN_POINT('Ctrl Pts',(-61.7930611596136,-111.336644206758,
174.763177688294));
#28999=CARTESIAN_POINT('Ctrl Pts',(-61.7831230458397,-111.243422447524,
175.985485192554));
#29000=CARTESIAN_POINT('Ctrl Pts',(-61.7731849320658,-111.15020068829,177.207792696815));
#29001=CARTESIAN_POINT('Ctrl Pts',(-60.9038148263651,-111.14860012117,178.072094585608));
#29002=CARTESIAN_POINT('Ctrl Pts',(-60.0344447206644,-111.14699955405,178.936396474401));
#29003=CARTESIAN_POINT('Ctrl Pts',(-58.8090862577616,-111.183349724129,
178.936396423256));
#29004=CARTESIAN_POINT('Ctrl Pts',(-57.5837277948587,-111.219699894207,
178.936396372111));
#29005=CARTESIAN_POINT('Ctrl Pts',(-56.7143577610805,-111.21809931942,178.072094410988));
#29006=CARTESIAN_POINT('Ctrl Pts',(-55.8449877273022,-111.216498744632,
177.207792449865));
#29007=CARTESIAN_POINT('Ctrl Pts',(-55.8350497152421,-111.123276974555,
175.985484945604));
#29008=CARTESIAN_POINT('Ctrl Pts',(-55.8251117031819,-111.030055204478,
174.763177441344));
#29009=CARTESIAN_POINT('Ctrl Pts',(-56.6746056830486,-110.845212242287,
173.89887555255));
#29010=CARTESIAN_POINT('Ctrl Pts',(-57.5240996629153,-110.660369280097,
173.034573663757));
#29011=CARTESIAN_POINT('Ctrl Pts',(-58.7295819999841,-110.437575580708,
173.034573714903));
#29012=CARTESIAN_POINT('Ctrl Pts',(-59.9350643370529,-110.214781881319,
173.034573766048));
#29013=CARTESIAN_POINT('Ctrl Pts',(-60.7845582449971,-110.029938926795,
173.898875727171));
#29014=CARTESIAN_POINT('Ctrl Pts',(-61.6340521529414,-109.845095972272,
174.763177688294));
#29015=CARTESIAN_POINT('Ctrl Pts',(-61.6241140391675,-109.751874213038,
175.985485192554));
#29016=CARTESIAN_POINT('Ctrl Pts',(-61.6141759253936,-109.658652453805,
177.207792696815));
#29017=CARTESIAN_POINT('Ctrl Pts',(-60.7448058196929,-109.657051886685,
178.072094585608));
#29018=CARTESIAN_POINT('Ctrl Pts',(-59.8754357139922,-109.655451319565,
178.936396474401));
#29019=CARTESIAN_POINT('Ctrl Pts',(-58.6500772510893,-109.691801489643,
178.936396423256));
#29020=CARTESIAN_POINT('Ctrl Pts',(-57.4247187881865,-109.728151659721,
178.936396372111));
#29021=CARTESIAN_POINT('Ctrl Pts',(-56.5553487544082,-109.726551084934,
178.072094410988));
#29022=CARTESIAN_POINT('Ctrl Pts',(-55.68597872063,-109.724950510147,177.207792449865));
#29023=CARTESIAN_POINT('Ctrl Pts',(-55.6760407085698,-109.63172874007,175.985484945604));
#29024=CARTESIAN_POINT('Ctrl Pts',(-55.6661026965097,-109.538506969993,
174.763177441344));
#29025=CARTESIAN_POINT('Ctrl Pts',(-56.5155966763764,-109.353664007802,
173.89887555255));
#29026=CARTESIAN_POINT('Ctrl Pts',(-57.365090656243,-109.168821045611,173.034573663757));
#29027=CARTESIAN_POINT('Ctrl Pts',(-58.5705729933119,-108.946027346222,
173.034573714903));
#29028=CARTESIAN_POINT('Ctrl Pts',(-59.7760553303807,-108.723233646833,
173.034573766048));
#29029=CARTESIAN_POINT('Ctrl Pts',(-60.6255492383249,-108.53839069231,173.898875727171));
#29030=CARTESIAN_POINT('Ctrl Pts',(-61.4750431462691,-108.353547737786,
174.763177688294));
#29031=CARTESIAN_POINT('Ctrl Pts',(-61.4651050324952,-108.260325978553,
175.985485192554));
#29032=CARTESIAN_POINT('Ctrl Pts',(-61.4551669187214,-108.167104219319,
177.207792696815));
#29033=CARTESIAN_POINT('Ctrl Pts',(-60.5857968130207,-108.165503652199,
178.072094585608));
#29034=CARTESIAN_POINT('Ctrl Pts',(-59.71642670732,-108.163903085079,178.936396474401));
#29035=CARTESIAN_POINT('Ctrl Pts',(-58.4910682444171,-108.200253255158,
178.936396423256));
#29036=CARTESIAN_POINT('Ctrl Pts',(-57.2657097815143,-108.236603425236,
178.936396372111));
#29037=CARTESIAN_POINT('Ctrl Pts',(-56.396339747736,-108.235002850448,178.072094410988));
#29038=CARTESIAN_POINT('Ctrl Pts',(-55.5269697139578,-108.233402275661,
177.207792449865));
#29039=CARTESIAN_POINT('Ctrl Pts',(-55.5170317018976,-108.140180505584,
175.985484945604));
#29040=CARTESIAN_POINT('Ctrl Pts',(-55.5070936898375,-108.046958735507,
174.763177441344));
#29041=CARTESIAN_POINT('Ctrl Pts',(-56.3565876697041,-107.862115773316,
173.89887555255));
#29042=CARTESIAN_POINT('Ctrl Pts',(-57.2060816495708,-107.677272811126,
173.034573663757));
#29043=CARTESIAN_POINT('Ctrl Pts',(-58.4115639866396,-107.454479111736,
173.034573714903));
#29044=CARTESIAN_POINT('Ctrl Pts',(-59.6170463237085,-107.231685412347,
173.034573766048));
#29045=CARTESIAN_POINT('Ctrl Pts',(-60.4665402316527,-107.046842457824,
173.898875727171));
#29046=CARTESIAN_POINT('Ctrl Pts',(-61.3160341395969,-106.861999503301,
174.763177688294));
#29047=CARTESIAN_POINT('Ctrl Pts',(-61.306096025823,-106.768777744067,175.985485192554));
#29048=CARTESIAN_POINT('Ctrl Pts',(-61.2961579120492,-106.675555984834,
177.207792696815));
#29049=CARTESIAN_POINT('Ctrl Pts',(-60.4267878063484,-106.673955417714,
178.072094585608));
#29050=CARTESIAN_POINT('Ctrl Pts',(-59.5574177006478,-106.672354850594,
178.936396474401));
#29051=CARTESIAN_POINT('Ctrl Pts',(-58.3320592377449,-106.708705020672,
178.936396423256));
#29052=CARTESIAN_POINT('Ctrl Pts',(-57.106700774842,-106.74505519075,178.936396372111));
#29053=CARTESIAN_POINT('Ctrl Pts',(-56.2373307410638,-106.743454615963,
178.072094410988));
#29054=CARTESIAN_POINT('Ctrl Pts',(-55.3679607072856,-106.741854041175,
177.207792449865));
#29055=CARTESIAN_POINT('Ctrl Pts',(-55.3580226952254,-106.648632271098,
175.985484945604));
#29056=CARTESIAN_POINT('Ctrl Pts',(-55.3480846831652,-106.555410501021,
174.763177441344));
#29057=CARTESIAN_POINT('Ctrl Pts',(-56.1975786630319,-106.370567538831,
173.89887555255));
#29058=CARTESIAN_POINT('Ctrl Pts',(-57.0470726428986,-106.18572457664,173.034573663757));
#29059=CARTESIAN_POINT('Ctrl Pts',(-58.2525549799674,-105.962930877251,
173.034573714903));
#29060=CARTESIAN_POINT('Ctrl Pts',(-59.4580373170363,-105.740137177862,
173.034573766048));
#29061=CARTESIAN_POINT('Ctrl Pts',(-60.3075312249805,-105.555294223339,
173.898875727171));
#29062=CARTESIAN_POINT('Ctrl Pts',(-61.1570251329247,-105.370451268815,
174.763177688294));
#29063=CARTESIAN_POINT('Ctrl Pts',(-61.1470870191508,-105.277229509582,
175.985485192554));
#29064=CARTESIAN_POINT('Ctrl Pts',(-61.1371489053769,-105.184007750348,
177.207792696815));
#29065=CARTESIAN_POINT('Ctrl Pts',(-60.2677787996762,-105.182407183228,
178.072094585608));
#29066=CARTESIAN_POINT('Ctrl Pts',(-59.3984086939755,-105.180806616108,
178.936396474401));
#29067=CARTESIAN_POINT('Ctrl Pts',(-58.1730502310727,-105.217156786186,
178.936396423256));
#29068=CARTESIAN_POINT('Ctrl Pts',(-56.9476917681698,-105.253506956265,
178.936396372111));
#29069=CARTESIAN_POINT('Ctrl Pts',(-56.0783217343916,-105.251906381477,
178.072094410988));
#29070=CARTESIAN_POINT('Ctrl Pts',(-55.2089517006133,-105.25030580669,177.207792449865));
#29071=CARTESIAN_POINT('Ctrl Pts',(-55.1990136885532,-105.157084036613,
175.985484945604));
#29072=CARTESIAN_POINT('Ctrl Pts',(-55.189075676493,-105.063862266536,174.763177441344));
#29073=CARTESIAN_POINT('Ctrl Pts',(-56.0385696563597,-104.879019304345,
173.89887555255));
#29074=CARTESIAN_POINT('Ctrl Pts',(-56.8880636362264,-104.694176342154,
173.034573663757));
#29075=CARTESIAN_POINT('Ctrl Pts',(-58.0935459732952,-104.471382642765,
173.034573714903));
#29076=CARTESIAN_POINT('Ctrl Pts',(-59.299028310364,-104.248588943376,173.034573766048));
#29077=CARTESIAN_POINT('Ctrl Pts',(-60.1485222183082,-104.063745988853,
173.898875727171));
#29078=CARTESIAN_POINT('Ctrl Pts',(-60.9980161262524,-103.87890303433,174.763177688294));
#29079=CARTESIAN_POINT('Ctrl Pts',(-60.9880780124786,-103.785681275096,
175.985485192554));
#29080=CARTESIAN_POINT('Ctrl Pts',(-60.9781398987047,-103.692459515862,
177.207792696815));
#29081=CARTESIAN_POINT('Ctrl Pts',(-60.108769793004,-103.690858948742,178.072094585608));
#29082=CARTESIAN_POINT('Ctrl Pts',(-59.2393996873033,-103.689258381622,
178.936396474401));
#29083=CARTESIAN_POINT('Ctrl Pts',(-58.0140412244004,-103.725608551701,
178.936396423256));
#29084=CARTESIAN_POINT('Ctrl Pts',(-56.7886827614976,-103.761958721779,
178.936396372111));
#29085=CARTESIAN_POINT('Ctrl Pts',(-55.9193127277193,-103.760358146992,
178.072094410988));
#29086=CARTESIAN_POINT('Ctrl Pts',(-55.0499426939411,-103.758757572204,
177.207792449865));
#29087=CARTESIAN_POINT('Ctrl Pts',(-55.0400046818809,-103.665535802127,
175.985484945604));
#29088=CARTESIAN_POINT('Ctrl Pts',(-55.0300666698208,-103.57231403205,174.763177441344));
#29089=CARTESIAN_POINT('Ctrl Pts',(-55.8795606496874,-103.387471069859,
173.89887555255));
#29090=CARTESIAN_POINT('Ctrl Pts',(-56.7290546295541,-103.202628107669,
173.034573663757));
#29091=CARTESIAN_POINT('Ctrl Pts',(-57.934536966623,-102.97983440828,173.034573714903));
#29092=CARTESIAN_POINT('Ctrl Pts',(-59.1400193036918,-102.757040708891,
173.034573766048));
#29093=CARTESIAN_POINT('Ctrl Pts',(-59.989513211636,-102.572197754367,173.898875727171));
#29094=CARTESIAN_POINT('Ctrl Pts',(-60.8390071195802,-102.387354799844,
174.763177688294));
#29095=CARTESIAN_POINT('Ctrl Pts',(-60.8290690058063,-102.29413304061,175.985485192554));
#29096=CARTESIAN_POINT('Ctrl Pts',(-60.8191308920325,-102.200911281377,
177.207792696815));
#29097=CARTESIAN_POINT('Ctrl Pts',(-59.9497607863318,-102.199310714257,
178.072094585608));
#29098=CARTESIAN_POINT('Ctrl Pts',(-59.0803906806311,-102.197710147137,
178.936396474401));
#29099=CARTESIAN_POINT('Ctrl Pts',(-57.8550322177282,-102.234060317215,
178.936396423256));
#29100=CARTESIAN_POINT('Ctrl Pts',(-56.6296737548253,-102.270410487293,
178.936396372111));
#29101=CARTESIAN_POINT('Ctrl Pts',(-55.7603037210471,-102.268809912506,
178.072094410988));
#29102=CARTESIAN_POINT('Ctrl Pts',(-54.8909336872689,-102.267209337719,
177.207792449865));
#29103=CARTESIAN_POINT('Ctrl Pts',(-54.8809956752087,-102.173987567642,
175.985484945604));
#29104=CARTESIAN_POINT('Ctrl Pts',(-54.8710576631486,-102.080765797565,
174.763177441344));
#29105=CARTESIAN_POINT('Ctrl Pts',(-55.7205516430152,-101.895922835374,
173.89887555255));
#29106=CARTESIAN_POINT('Ctrl Pts',(-56.5700456228819,-101.711079873183,
173.034573663757));
#29107=CARTESIAN_POINT('Ctrl Pts',(-57.7755279599507,-101.488286173794,
173.034573714903));
#29108=CARTESIAN_POINT('Ctrl Pts',(-58.9810102970196,-101.265492474405,
173.034573766048));
#29109=CARTESIAN_POINT('Ctrl Pts',(-59.8305042049638,-101.080649519882,
173.898875727171));
#29110=CARTESIAN_POINT('Ctrl Pts',(-60.679998112908,-100.895806565358,174.763177688294));
#29111=CARTESIAN_POINT('Ctrl Pts',(-60.6700599991341,-100.802584806125,
175.985485192554));
#29112=CARTESIAN_POINT('Ctrl Pts',(-60.6601218853602,-100.709363046891,
177.207792696815));
#29113=CARTESIAN_POINT('Ctrl Pts',(-59.7907517796595,-100.707762479771,
178.072094585608));
#29114=CARTESIAN_POINT('Ctrl Pts',(-58.9213816739588,-100.706161912651,
178.936396474401));
#29115=CARTESIAN_POINT('Ctrl Pts',(-57.696023211056,-100.742512082729,178.936396423256));
#29116=CARTESIAN_POINT('Ctrl Pts',(-56.4706647481531,-100.778862252808,
178.936396372111));
#29117=CARTESIAN_POINT('Ctrl Pts',(-55.6012947143749,-100.77726167802,178.072094410988));
#29118=CARTESIAN_POINT('Ctrl Pts',(-54.7319246805966,-100.775661103233,
177.207792449865));
#29119=CARTESIAN_POINT('Ctrl Pts',(-54.7219866685365,-100.682439333156,
175.985484945604));
#29120=CARTESIAN_POINT('Ctrl Pts',(-54.7120486564763,-100.589217563079,
174.763177441344));
#29121=CARTESIAN_POINT('Ctrl Pts',(-55.561542636343,-100.404374600888,173.89887555255));
#29122=CARTESIAN_POINT('Ctrl Pts',(-56.4110366162097,-100.219531638698,
173.034573663757));
#29123=CARTESIAN_POINT('Ctrl Pts',(-57.6165189532785,-99.9967379393085,
173.034573714903));
#29124=CARTESIAN_POINT('Ctrl Pts',(-58.8220012903473,-99.7739442399195,
173.034573766048));
#29125=CARTESIAN_POINT('Ctrl Pts',(-59.6714951982915,-99.5891012853962,
173.898875727171));
#29126=CARTESIAN_POINT('Ctrl Pts',(-60.5209891062358,-99.4042583308729,
174.763177688294));
#29127=CARTESIAN_POINT('Ctrl Pts',(-60.5110509924619,-99.3110365716392,
175.985485192554));
#29128=CARTESIAN_POINT('Ctrl Pts',(-60.501112878688,-99.2178148124055,177.207792696815));
#29129=CARTESIAN_POINT('Ctrl Pts',(-59.6317427729873,-99.2162142452855,
178.072094585608));
#29130=CARTESIAN_POINT('Ctrl Pts',(-58.7623726672866,-99.2146136781656,
178.936396474401));
#29131=CARTESIAN_POINT('Ctrl Pts',(-57.5370142043838,-99.2509638482439,
178.936396423256));
#29132=CARTESIAN_POINT('Ctrl Pts',(-56.3116557414809,-99.2873140183222,
178.936396372111));
#29133=CARTESIAN_POINT('Ctrl Pts',(-55.4422857077027,-99.2857134435348,
178.072094410988));
#29134=CARTESIAN_POINT('Ctrl Pts',(-54.5729156739244,-99.2841128687474,
177.207792449865));
#29135=CARTESIAN_POINT('Ctrl Pts',(-54.5629776618643,-99.1908910986704,
175.985484945604));
#29136=CARTESIAN_POINT('Ctrl Pts',(-54.5530396498041,-99.0976693285933,
174.763177441344));
#29137=CARTESIAN_POINT('Ctrl Pts',(-55.4025336296708,-98.9128263664026,
173.89887555255));
#29138=CARTESIAN_POINT('Ctrl Pts',(-56.2520276095374,-98.727983404212,173.034573663757));
#29139=CARTESIAN_POINT('Ctrl Pts',(-57.4575099466063,-98.5051897048229,
173.034573714903));
#29140=CARTESIAN_POINT('Ctrl Pts',(-58.6629922836751,-98.2823960054338,
173.034573766048));
#29141=CARTESIAN_POINT('Ctrl Pts',(-59.5124861916193,-98.0975530509106,
173.898875727171));
#29142=CARTESIAN_POINT('Ctrl Pts',(-60.3619800995635,-97.9127100963873,
174.763177688294));
#29143=CARTESIAN_POINT('Ctrl Pts',(-60.3520419857897,-97.8194883371536,
175.985485192554));
#29144=CARTESIAN_POINT('Ctrl Pts',(-60.3421038720158,-97.7262665779199,
177.207792696815));
#29145=CARTESIAN_POINT('Ctrl Pts',(-59.4727337663151,-97.7246660108,178.072094585608));
#29146=CARTESIAN_POINT('Ctrl Pts',(-58.6033636606144,-97.72306544368,178.936396474401));
#29147=CARTESIAN_POINT('Ctrl Pts',(-57.3780051977115,-97.7594156137583,
178.936396423256));
#29148=CARTESIAN_POINT('Ctrl Pts',(-56.1526467348087,-97.7957657838366,
178.936396372111));
#29149=CARTESIAN_POINT('Ctrl Pts',(-55.2832767010304,-97.7941652090492,
178.072094410988));
#29150=CARTESIAN_POINT('Ctrl Pts',(-56.1707931031902,-113.117197303651,
178.813912075476));
#29151=CARTESIAN_POINT('Ctrl Pts',(-54.9958834532485,-113.148169293224,
177.6423391512));
#29152=CARTESIAN_POINT('Ctrl Pts',(-54.9859454592686,-113.05494752122,175.985484901707));
#29153=CARTESIAN_POINT('Ctrl Pts',(-54.9760074652888,-112.961725749215,
174.328630652215));
#29154=CARTESIAN_POINT('Ctrl Pts',(-56.1310410868884,-112.744310219938,
173.157057825983));
#29155=CARTESIAN_POINT('Ctrl Pts',(-57.286074708488,-112.52689469066,171.985484999752));
#29156=CARTESIAN_POINT('Ctrl Pts',(-58.9236553326579,-112.258036427063,
171.985485069079));
#29157=CARTESIAN_POINT('Ctrl Pts',(-60.5612359568277,-111.989178163466,
171.985485138407));
#29158=CARTESIAN_POINT('Ctrl Pts',(-61.7162694809355,-111.771762644582,
173.157058062683));
#29159=CARTESIAN_POINT('Ctrl Pts',(-62.8713030050432,-111.554347125698,
174.328630986959));
#29160=CARTESIAN_POINT('Ctrl Pts',(-62.861364873189,-111.461125368392,175.985485236451));
#29161=CARTESIAN_POINT('Ctrl Pts',(-62.8514267413349,-111.367903611086,
177.642339485944));
#29162=CARTESIAN_POINT('Ctrl Pts',(-61.6765169939012,-111.398875611052,
178.813912312176));
#29163=CARTESIAN_POINT('Ctrl Pts',(-60.5016072464676,-111.429847611019,
179.985485138407));
#29164=CARTESIAN_POINT('Ctrl Pts',(-58.8441504964637,-111.512262345305,
179.985485069079));
#29165=CARTESIAN_POINT('Ctrl Pts',(-57.1866937464598,-111.594677079592,
179.985484999752));
#29166=CARTESIAN_POINT('Ctrl Pts',(-56.011784096518,-111.625649069165,178.813912075476));
#29167=CARTESIAN_POINT('Ctrl Pts',(-54.8368744465762,-111.656621058739,
177.6423391512));
#29168=CARTESIAN_POINT('Ctrl Pts',(-54.8269364525964,-111.563399286734,
175.985484901707));
#29169=CARTESIAN_POINT('Ctrl Pts',(-54.8169984586165,-111.47017751473,174.328630652215));
#29170=CARTESIAN_POINT('Ctrl Pts',(-55.9720320802161,-111.252761985452,
173.157057825983));
#29171=CARTESIAN_POINT('Ctrl Pts',(-57.1270657018158,-111.035346456175,
171.985484999752));
#29172=CARTESIAN_POINT('Ctrl Pts',(-58.7646463259856,-110.766488192578,
171.985485069079));
#29173=CARTESIAN_POINT('Ctrl Pts',(-60.4022269501555,-110.497629928981,
171.985485138407));
#29174=CARTESIAN_POINT('Ctrl Pts',(-61.5572604742632,-110.280214410097,
173.157058062683));
#29175=CARTESIAN_POINT('Ctrl Pts',(-62.712293998371,-110.062798891212,174.328630986959));
#29176=CARTESIAN_POINT('Ctrl Pts',(-62.7023558665168,-109.969577133906,
175.985485236451));
#29177=CARTESIAN_POINT('Ctrl Pts',(-62.6924177346626,-109.8763553766,177.642339485944));
#29178=CARTESIAN_POINT('Ctrl Pts',(-61.517507987229,-109.907327376567,178.813912312176));
#29179=CARTESIAN_POINT('Ctrl Pts',(-60.3425982397954,-109.938299376534,
179.985485138407));
#29180=CARTESIAN_POINT('Ctrl Pts',(-58.6851414897915,-110.02071411082,179.985485069079));
#29181=CARTESIAN_POINT('Ctrl Pts',(-57.0276847397876,-110.103128845106,
179.985484999752));
#29182=CARTESIAN_POINT('Ctrl Pts',(-55.8527750898458,-110.13410083468,178.813912075476));
#29183=CARTESIAN_POINT('Ctrl Pts',(-54.677865439904,-110.165072824253,177.6423391512));
#29184=CARTESIAN_POINT('Ctrl Pts',(-54.6679274459242,-110.071851052249,
175.985484901707));
#29185=CARTESIAN_POINT('Ctrl Pts',(-54.6579894519443,-109.978629280244,
174.328630652215));
#29186=CARTESIAN_POINT('Ctrl Pts',(-55.8130230735439,-109.761213750967,
173.157057825983));
#29187=CARTESIAN_POINT('Ctrl Pts',(-56.9680566951435,-109.543798221689,
171.985484999752));
#29188=CARTESIAN_POINT('Ctrl Pts',(-58.6056373193134,-109.274939958092,
171.985485069079));
#29189=CARTESIAN_POINT('Ctrl Pts',(-60.2432179434833,-109.006081694495,
171.985485138407));
#29190=CARTESIAN_POINT('Ctrl Pts',(-61.398251467591,-108.788666175611,173.157058062683));
#29191=CARTESIAN_POINT('Ctrl Pts',(-62.5532849916988,-108.571250656727,
174.328630986959));
#29192=CARTESIAN_POINT('Ctrl Pts',(-62.5433468598446,-108.478028899421,
175.985485236451));
#29193=CARTESIAN_POINT('Ctrl Pts',(-62.5334087279904,-108.384807142114,
177.642339485944));
#29194=CARTESIAN_POINT('Ctrl Pts',(-61.3584989805568,-108.415779142081,
178.813912312176));
#29195=CARTESIAN_POINT('Ctrl Pts',(-60.1835892331231,-108.446751142048,
179.985485138407));
#29196=CARTESIAN_POINT('Ctrl Pts',(-58.5261324831192,-108.529165876334,
179.985485069079));
#29197=CARTESIAN_POINT('Ctrl Pts',(-56.8686757331153,-108.611580610621,
179.985484999752));
#29198=CARTESIAN_POINT('Ctrl Pts',(-55.6937660831736,-108.642552600194,
178.813912075476));
#29199=CARTESIAN_POINT('Ctrl Pts',(-54.5188564332318,-108.673524589768,
177.6423391512));
#29200=CARTESIAN_POINT('Ctrl Pts',(-54.5089184392519,-108.580302817763,
175.985484901707));
#29201=CARTESIAN_POINT('Ctrl Pts',(-54.4989804452721,-108.487081045759,
174.328630652215));
#29202=CARTESIAN_POINT('Ctrl Pts',(-55.6540140668717,-108.269665516481,
173.157057825983));
#29203=CARTESIAN_POINT('Ctrl Pts',(-56.8090476884713,-108.052249987204,
171.985484999752));
#29204=CARTESIAN_POINT('Ctrl Pts',(-58.4466283126412,-107.783391723607,
171.985485069079));
#29205=CARTESIAN_POINT('Ctrl Pts',(-60.084208936811,-107.51453346001,171.985485138407));
#29206=CARTESIAN_POINT('Ctrl Pts',(-61.2392424609188,-107.297117941125,
173.157058062683));
#29207=CARTESIAN_POINT('Ctrl Pts',(-62.3942759850265,-107.079702422241,
174.328630986959));
#29208=CARTESIAN_POINT('Ctrl Pts',(-62.3843378531723,-106.986480664935,
175.985485236451));
#29209=CARTESIAN_POINT('Ctrl Pts',(-62.3743997213182,-106.893258907629,
177.642339485944));
#29210=CARTESIAN_POINT('Ctrl Pts',(-61.1994899738845,-106.924230907596,
178.813912312176));
#29211=CARTESIAN_POINT('Ctrl Pts',(-60.0245802264509,-106.955202907562,
179.985485138407));
#29212=CARTESIAN_POINT('Ctrl Pts',(-58.367123476447,-107.037617641849,179.985485069079));
#29213=CARTESIAN_POINT('Ctrl Pts',(-56.7096667264431,-107.120032376135,
179.985484999752));
#29214=CARTESIAN_POINT('Ctrl Pts',(-55.5347570765013,-107.151004365708,
178.813912075476));
#29215=CARTESIAN_POINT('Ctrl Pts',(-54.3598474265596,-107.181976355282,
177.6423391512));
#29216=CARTESIAN_POINT('Ctrl Pts',(-54.3499094325797,-107.088754583277,
175.985484901707));
#29217=CARTESIAN_POINT('Ctrl Pts',(-54.3399714385998,-106.995532811273,
174.328630652215));
#29218=CARTESIAN_POINT('Ctrl Pts',(-55.4950050601995,-106.778117281995,
173.157057825983));
#29219=CARTESIAN_POINT('Ctrl Pts',(-56.6500386817991,-106.560701752718,
171.985484999752));
#29220=CARTESIAN_POINT('Ctrl Pts',(-58.2876193059689,-106.291843489121,
171.985485069079));
#29221=CARTESIAN_POINT('Ctrl Pts',(-59.9251999301388,-106.022985225524,
171.985485138407));
#29222=CARTESIAN_POINT('Ctrl Pts',(-61.0802334542465,-105.80556970664,173.157058062683));
#29223=CARTESIAN_POINT('Ctrl Pts',(-62.2352669783543,-105.588154187756,
174.328630986959));
#29224=CARTESIAN_POINT('Ctrl Pts',(-62.2253288465001,-105.494932430449,
175.985485236451));
#29225=CARTESIAN_POINT('Ctrl Pts',(-62.2153907146459,-105.401710673143,
177.642339485944));
#29226=CARTESIAN_POINT('Ctrl Pts',(-61.0404809672123,-105.43268267311,178.813912312176));
#29227=CARTESIAN_POINT('Ctrl Pts',(-59.8655712197787,-105.463654673077,
179.985485138407));
#29228=CARTESIAN_POINT('Ctrl Pts',(-58.2081144697748,-105.546069407363,
179.985485069079));
#29229=CARTESIAN_POINT('Ctrl Pts',(-56.5506577197709,-105.628484141649,
179.985484999752));
#29230=CARTESIAN_POINT('Ctrl Pts',(-55.3757480698291,-105.659456131223,
178.813912075476));
#29231=CARTESIAN_POINT('Ctrl Pts',(-54.2008384198873,-105.690428120796,
177.6423391512));
#29232=CARTESIAN_POINT('Ctrl Pts',(-54.1909004259075,-105.597206348792,
175.985484901707));
#29233=CARTESIAN_POINT('Ctrl Pts',(-54.1809624319276,-105.503984576787,
174.328630652215));
#29234=CARTESIAN_POINT('Ctrl Pts',(-55.3359960535272,-105.28656904751,173.157057825983));
#29235=CARTESIAN_POINT('Ctrl Pts',(-56.4910296751268,-105.069153518232,
171.985484999752));
#29236=CARTESIAN_POINT('Ctrl Pts',(-58.1286102992967,-104.800295254635,
171.985485069079));
#29237=CARTESIAN_POINT('Ctrl Pts',(-59.7661909234666,-104.531436991038,
171.985485138407));
#29238=CARTESIAN_POINT('Ctrl Pts',(-60.9212244475743,-104.314021472154,
173.157058062683));
#29239=CARTESIAN_POINT('Ctrl Pts',(-62.0762579716821,-104.09660595327,174.328630986959));
#29240=CARTESIAN_POINT('Ctrl Pts',(-62.0663198398279,-104.003384195964,
175.985485236451));
#29241=CARTESIAN_POINT('Ctrl Pts',(-62.0563817079737,-103.910162438658,
177.642339485944));
#29242=CARTESIAN_POINT('Ctrl Pts',(-60.8814719605401,-103.941134438624,
178.813912312176));
#29243=CARTESIAN_POINT('Ctrl Pts',(-59.7065622131064,-103.972106438591,
179.985485138407));
#29244=CARTESIAN_POINT('Ctrl Pts',(-58.0491054631025,-104.054521172878,
179.985485069079));
#29245=CARTESIAN_POINT('Ctrl Pts',(-56.3916487130987,-104.136935907164,
179.985484999752));
#29246=CARTESIAN_POINT('Ctrl Pts',(-55.2167390631569,-104.167907896737,
178.813912075476));
#29247=CARTESIAN_POINT('Ctrl Pts',(-54.0418294132151,-104.198879886311,
177.6423391512));
#29248=CARTESIAN_POINT('Ctrl Pts',(-54.0318914192353,-104.105658114306,
175.985484901707));
#29249=CARTESIAN_POINT('Ctrl Pts',(-54.0219534252554,-104.012436342302,
174.328630652215));
#29250=CARTESIAN_POINT('Ctrl Pts',(-55.176987046855,-103.795020813024,173.157057825983));
#29251=CARTESIAN_POINT('Ctrl Pts',(-56.3320206684546,-103.577605283747,
171.985484999752));
#29252=CARTESIAN_POINT('Ctrl Pts',(-57.9696012926245,-103.30874702015,171.985485069079));
#29253=CARTESIAN_POINT('Ctrl Pts',(-59.6071819167943,-103.039888756553,
171.985485138407));
#29254=CARTESIAN_POINT('Ctrl Pts',(-60.7622154409021,-102.822473237669,
173.157058062683));
#29255=CARTESIAN_POINT('Ctrl Pts',(-61.9172489650099,-102.605057718784,
174.328630986959));
#29256=CARTESIAN_POINT('Ctrl Pts',(-61.9073108331557,-102.511835961478,
175.985485236451));
#29257=CARTESIAN_POINT('Ctrl Pts',(-61.8973727013015,-102.418614204172,
177.642339485944));
#29258=CARTESIAN_POINT('Ctrl Pts',(-60.7224629538678,-102.449586204139,
178.813912312176));
#29259=CARTESIAN_POINT('Ctrl Pts',(-59.5475532064342,-102.480558204106,
179.985485138407));
#29260=CARTESIAN_POINT('Ctrl Pts',(-57.8900964564303,-102.562972938392,
179.985485069079));
#29261=CARTESIAN_POINT('Ctrl Pts',(-56.2326397064264,-102.645387672678,
179.985484999752));
#29262=CARTESIAN_POINT('Ctrl Pts',(-55.0577300564847,-102.676359662252,
178.813912075476));
#29263=CARTESIAN_POINT('Ctrl Pts',(-53.8828204065429,-102.707331651825,
177.6423391512));
#29264=CARTESIAN_POINT('Ctrl Pts',(-53.872882412563,-102.614109879821,175.985484901707));
#29265=CARTESIAN_POINT('Ctrl Pts',(-53.8629444185832,-102.520888107816,
174.328630652215));
#29266=CARTESIAN_POINT('Ctrl Pts',(-55.0179780401828,-102.303472578539,
173.157057825983));
#29267=CARTESIAN_POINT('Ctrl Pts',(-56.1730116617824,-102.086057049261,
171.985484999752));
#29268=CARTESIAN_POINT('Ctrl Pts',(-57.8105922859523,-101.817198785664,
171.985485069079));
#29269=CARTESIAN_POINT('Ctrl Pts',(-59.4481729101221,-101.548340522067,
171.985485138407));
#29270=CARTESIAN_POINT('Ctrl Pts',(-60.6032064342299,-101.330925003183,
173.157058062683));
#29271=CARTESIAN_POINT('Ctrl Pts',(-61.7582399583376,-101.113509484299,
174.328630986959));
#29272=CARTESIAN_POINT('Ctrl Pts',(-61.7483018264834,-101.020287726993,
175.985485236451));
#29273=CARTESIAN_POINT('Ctrl Pts',(-61.7383636946293,-100.927065969686,
177.642339485944));
#29274=CARTESIAN_POINT('Ctrl Pts',(-60.5634539471956,-100.958037969653,
178.813912312176));
#29275=CARTESIAN_POINT('Ctrl Pts',(-59.388544199762,-100.98900996962,179.985485138407));
#29276=CARTESIAN_POINT('Ctrl Pts',(-57.7310874497581,-101.071424703906,
179.985485069079));
#29277=CARTESIAN_POINT('Ctrl Pts',(-56.0736306997542,-101.153839438193,
179.985484999752));
#29278=CARTESIAN_POINT('Ctrl Pts',(-54.8987210498124,-101.184811427766,
178.813912075476));
#29279=CARTESIAN_POINT('Ctrl Pts',(-53.7238113998707,-101.21578341734,177.6423391512));
#29280=CARTESIAN_POINT('Ctrl Pts',(-53.7138734058908,-101.122561645335,
175.985484901707));
#29281=CARTESIAN_POINT('Ctrl Pts',(-53.7039354119109,-101.029339873331,
174.328630652215));
#29282=CARTESIAN_POINT('Ctrl Pts',(-54.8589690335105,-100.811924344053,
173.157057825983));
#29283=CARTESIAN_POINT('Ctrl Pts',(-56.0140026551102,-100.594508814776,
171.985484999752));
#29284=CARTESIAN_POINT('Ctrl Pts',(-57.65158327928,-100.325650551179,171.985485069079));
#29285=CARTESIAN_POINT('Ctrl Pts',(-59.2891639034499,-100.056792287582,
171.985485138407));
#29286=CARTESIAN_POINT('Ctrl Pts',(-60.4441974275576,-99.8393767686974,
173.157058062683));
#29287=CARTESIAN_POINT('Ctrl Pts',(-61.5992309516654,-99.6219612498133,
174.328630986959));
#29288=CARTESIAN_POINT('Ctrl Pts',(-61.5892928198112,-99.528739492507,175.985485236451));
#29289=CARTESIAN_POINT('Ctrl Pts',(-61.579354687957,-99.4355177352008,177.642339485944));
#29290=CARTESIAN_POINT('Ctrl Pts',(-60.4044449405234,-99.4664897351676,
178.813912312176));
#29291=CARTESIAN_POINT('Ctrl Pts',(-59.2295351930898,-99.4974617351344,
179.985485138407));
#29292=CARTESIAN_POINT('Ctrl Pts',(-57.5720784430859,-99.5798764694207,
179.985485069079));
#29293=CARTESIAN_POINT('Ctrl Pts',(-55.914621693082,-99.662291203707,179.985484999752));
#29294=CARTESIAN_POINT('Ctrl Pts',(-54.7397120431402,-99.6932631932805,
178.813912075476));
#29295=CARTESIAN_POINT('Ctrl Pts',(-53.5648023931984,-99.724235182854,177.6423391512));
#29296=CARTESIAN_POINT('Ctrl Pts',(-53.5548643992186,-99.6310134108495,
175.985484901707));
#29297=CARTESIAN_POINT('Ctrl Pts',(-53.5449264052387,-99.5377916388449,
174.328630652215));
#29298=CARTESIAN_POINT('Ctrl Pts',(-54.6999600268383,-99.3203761095675,
173.157057825983));
#29299=CARTESIAN_POINT('Ctrl Pts',(-55.8549936484379,-99.10296058029,171.985484999752));
#29300=CARTESIAN_POINT('Ctrl Pts',(-57.4925742726078,-98.834102316693,171.985485069079));
#29301=CARTESIAN_POINT('Ctrl Pts',(-59.1301548967777,-98.565244053096,171.985485138407));
#29302=CARTESIAN_POINT('Ctrl Pts',(-60.2851884208854,-98.3478285342118,
173.157058062683));
#29303=CARTESIAN_POINT('Ctrl Pts',(-61.4402219449932,-98.1304130153276,
174.328630986959));
#29304=CARTESIAN_POINT('Ctrl Pts',(-61.430283813139,-98.0371912580215,175.985485236451));
#29305=CARTESIAN_POINT('Ctrl Pts',(-61.4203456812848,-97.9439695007152,
177.642339485944));
#29306=CARTESIAN_POINT('Ctrl Pts',(-60.2454359338512,-97.974941500682,178.813912312176));
#29307=CARTESIAN_POINT('Ctrl Pts',(-59.0705261864175,-98.0059135006488,
179.985485138407));
#29308=CARTESIAN_POINT('Ctrl Pts',(-57.4130694364136,-98.0883282349351,
179.985485069079));
#29309=CARTESIAN_POINT('Ctrl Pts',(-55.7556126864097,-98.1707429692214,
179.985484999752));
#29310=CARTESIAN_POINT('Ctrl Pts',(-54.580703036468,-98.2017149587949,178.813912075476));
#29311=CARTESIAN_POINT('Ctrl Pts',(-61.3355965912452,-105.42684148695,178.485485069079));
#29312=CARTESIAN_POINT('Ctrl Pts',(-61.1970243868884,-105.428556004828,
178.657813499464));
#29313=CARTESIAN_POINT('Ctrl Pts',(-61.0404809672123,-105.43268267311,178.813912312176));
#29314=CARTESIAN_POINT('Ctrl Pts',(-59.8655712197787,-105.463654673077,
179.985485138407));
#29315=CARTESIAN_POINT('Ctrl Pts',(-58.2081144697748,-105.546069407363,
179.985485069079));
#29316=CARTESIAN_POINT('Ctrl Pts',(-56.5506577197709,-105.628484141649,
179.985484999752));
#29317=CARTESIAN_POINT('Ctrl Pts',(-55.3757480698291,-105.659456131223,
178.813912075476));
#29318=CARTESIAN_POINT('Ctrl Pts',(-54.2008384198873,-105.690428120796,
177.6423391512));
#29319=CARTESIAN_POINT('Ctrl Pts',(-54.1909004259075,-105.597206348792,
175.985484901707));
#29320=CARTESIAN_POINT('Ctrl Pts',(-54.1809624319276,-105.503984576787,
174.328630652215));
#29321=CARTESIAN_POINT('Ctrl Pts',(-55.3359960535272,-105.28656904751,173.157057825983));
#29322=CARTESIAN_POINT('Ctrl Pts',(-56.4910296751268,-105.069153518232,
171.985484999752));
#29323=CARTESIAN_POINT('Ctrl Pts',(-58.1286102992967,-104.800295254635,
171.985485069079));
#29324=CARTESIAN_POINT('Ctrl Pts',(-59.7661909234666,-104.531436991038,
171.985485138407));
#29325=CARTESIAN_POINT('Ctrl Pts',(-60.9212244475743,-104.314021472154,
173.157058062683));
#29326=CARTESIAN_POINT('Ctrl Pts',(-61.0751194685275,-104.285053338212,
173.313156769748));
#29327=CARTESIAN_POINT('Ctrl Pts',(-61.2109386724983,-104.25751590903,173.485485069079));
#29328=CARTESIAN_POINT('Ctrl Pts',(-56.1707931031902,-113.117197303651,
178.813912075476));
#29329=CARTESIAN_POINT('Ctrl Pts',(-54.9958834532485,-113.148169293224,
177.6423391512));
#29330=CARTESIAN_POINT('Ctrl Pts',(-54.9859454592686,-113.05494752122,175.985484901707));
#29331=CARTESIAN_POINT('Ctrl Pts',(-54.9760074652888,-112.961725749215,
174.328630652215));
#29332=CARTESIAN_POINT('Ctrl Pts',(-56.1310410868884,-112.744310219938,
173.157057825983));
#29333=CARTESIAN_POINT('Ctrl Pts',(-57.286074708488,-112.52689469066,171.985484999752));
#29334=CARTESIAN_POINT('Ctrl Pts',(-58.9236553326578,-112.258036427063,
171.985485069079));
#29335=CARTESIAN_POINT('Ctrl Pts',(-60.5612359568277,-111.989178163466,
171.985485138407));
#29336=CARTESIAN_POINT('Ctrl Pts',(-61.7162694809355,-111.771762644582,
173.157058062683));
#29337=CARTESIAN_POINT('Ctrl Pts',(-62.8713030050432,-111.554347125698,
174.328630986959));
#29338=CARTESIAN_POINT('Ctrl Pts',(-62.861364873189,-111.461125368392,175.985485236451));
#29339=CARTESIAN_POINT('Ctrl Pts',(-62.8514267413349,-111.367903611086,
177.642339485944));
#29340=CARTESIAN_POINT('Ctrl Pts',(-61.6765169939012,-111.398875611052,
178.813912312176));
#29341=CARTESIAN_POINT('Ctrl Pts',(-60.5016072464676,-111.429847611019,
179.985485138407));
#29342=CARTESIAN_POINT('Ctrl Pts',(-58.8441504964637,-111.512262345305,
179.985485069079));
#29343=CARTESIAN_POINT('Ctrl Pts',(-57.1866937464598,-111.594677079592,
179.985484999752));
#29344=CARTESIAN_POINT('Ctrl Pts',(-56.011784096518,-111.625649069165,178.813912075476));
#29345=CARTESIAN_POINT('Ctrl Pts',(-54.8368744465763,-111.656621058739,
177.6423391512));
#29346=CARTESIAN_POINT('Ctrl Pts',(-54.8269364525964,-111.563399286734,
175.985484901707));
#29347=CARTESIAN_POINT('Ctrl Pts',(-54.8169984586165,-111.47017751473,174.328630652215));
#29348=CARTESIAN_POINT('Ctrl Pts',(-55.9720320802161,-111.252761985452,
173.157057825983));
#29349=CARTESIAN_POINT('Ctrl Pts',(-57.1270657018158,-111.035346456175,
171.985484999752));
#29350=CARTESIAN_POINT('Ctrl Pts',(-58.7646463259856,-110.766488192578,
171.985485069079));
#29351=CARTESIAN_POINT('Ctrl Pts',(-60.4022269501555,-110.497629928981,
171.985485138407));
#29352=CARTESIAN_POINT('Ctrl Pts',(-61.5572604742632,-110.280214410097,
173.157058062683));
#29353=CARTESIAN_POINT('Ctrl Pts',(-62.712293998371,-110.062798891212,174.328630986959));
#29354=CARTESIAN_POINT('Ctrl Pts',(-62.7023558665168,-109.969577133906,
175.985485236451));
#29355=CARTESIAN_POINT('Ctrl Pts',(-62.6924177346626,-109.8763553766,177.642339485944));
#29356=CARTESIAN_POINT('Ctrl Pts',(-61.517507987229,-109.907327376567,178.813912312176));
#29357=CARTESIAN_POINT('Ctrl Pts',(-60.3425982397954,-109.938299376534,
179.985485138407));
#29358=CARTESIAN_POINT('Ctrl Pts',(-58.6851414897915,-110.02071411082,179.985485069079));
#29359=CARTESIAN_POINT('Ctrl Pts',(-57.0276847397876,-110.103128845106,
179.985484999752));
#29360=CARTESIAN_POINT('Ctrl Pts',(-55.8527750898458,-110.13410083468,178.813912075476));
#29361=CARTESIAN_POINT('Ctrl Pts',(-54.677865439904,-110.165072824253,177.6423391512));
#29362=CARTESIAN_POINT('Ctrl Pts',(-54.6679274459242,-110.071851052249,
175.985484901707));
#29363=CARTESIAN_POINT('Ctrl Pts',(-54.6579894519443,-109.978629280244,
174.328630652215));
#29364=CARTESIAN_POINT('Ctrl Pts',(-55.8130230735439,-109.761213750967,
173.157057825983));
#29365=CARTESIAN_POINT('Ctrl Pts',(-56.9680566951435,-109.543798221689,
171.985484999752));
#29366=CARTESIAN_POINT('Ctrl Pts',(-58.6056373193134,-109.274939958092,
171.985485069079));
#29367=CARTESIAN_POINT('Ctrl Pts',(-60.2432179434833,-109.006081694495,
171.985485138407));
#29368=CARTESIAN_POINT('Ctrl Pts',(-61.398251467591,-108.788666175611,173.157058062683));
#29369=CARTESIAN_POINT('Ctrl Pts',(-62.5532849916988,-108.571250656727,
174.328630986959));
#29370=CARTESIAN_POINT('Ctrl Pts',(-62.5433468598446,-108.478028899421,
175.985485236451));
#29371=CARTESIAN_POINT('Ctrl Pts',(-62.5334087279904,-108.384807142114,
177.642339485944));
#29372=CARTESIAN_POINT('Ctrl Pts',(-61.3584989805568,-108.415779142081,
178.813912312176));
#29373=CARTESIAN_POINT('Ctrl Pts',(-60.1835892331231,-108.446751142048,
179.985485138407));
#29374=CARTESIAN_POINT('Ctrl Pts',(-58.5261324831192,-108.529165876334,
179.985485069079));
#29375=CARTESIAN_POINT('Ctrl Pts',(-56.8686757331153,-108.611580610621,
179.985484999752));
#29376=CARTESIAN_POINT('Ctrl Pts',(-55.6937660831736,-108.642552600194,
178.813912075476));
#29377=CARTESIAN_POINT('Ctrl Pts',(-54.5188564332318,-108.673524589768,
177.6423391512));
#29378=CARTESIAN_POINT('Ctrl Pts',(-54.5089184392519,-108.580302817763,
175.985484901707));
#29379=CARTESIAN_POINT('Ctrl Pts',(-54.4989804452721,-108.487081045759,
174.328630652215));
#29380=CARTESIAN_POINT('Ctrl Pts',(-55.6540140668717,-108.269665516481,
173.157057825983));
#29381=CARTESIAN_POINT('Ctrl Pts',(-56.8090476884713,-108.052249987204,
171.985484999752));
#29382=CARTESIAN_POINT('Ctrl Pts',(-58.4466283126412,-107.783391723607,
171.985485069079));
#29383=CARTESIAN_POINT('Ctrl Pts',(-60.084208936811,-107.51453346001,171.985485138407));
#29384=CARTESIAN_POINT('Ctrl Pts',(-61.2392424609188,-107.297117941125,
173.157058062683));
#29385=CARTESIAN_POINT('Ctrl Pts',(-62.3942759850265,-107.079702422241,
174.328630986959));
#29386=CARTESIAN_POINT('Ctrl Pts',(-62.3843378531723,-106.986480664935,
175.985485236451));
#29387=CARTESIAN_POINT('Ctrl Pts',(-62.3743997213182,-106.893258907629,
177.642339485944));
#29388=CARTESIAN_POINT('Ctrl Pts',(-61.1994899738845,-106.924230907596,
178.813912312176));
#29389=CARTESIAN_POINT('Ctrl Pts',(-60.0245802264509,-106.955202907562,
179.985485138407));
#29390=CARTESIAN_POINT('Ctrl Pts',(-58.367123476447,-107.037617641849,179.985485069079));
#29391=CARTESIAN_POINT('Ctrl Pts',(-56.7096667264431,-107.120032376135,
179.985484999752));
#29392=CARTESIAN_POINT('Ctrl Pts',(-55.5347570765013,-107.151004365708,
178.813912075476));
#29393=CARTESIAN_POINT('Ctrl Pts',(-54.3598474265596,-107.181976355282,
177.6423391512));
#29394=CARTESIAN_POINT('Ctrl Pts',(-54.3499094325797,-107.088754583277,
175.985484901707));
#29395=CARTESIAN_POINT('Ctrl Pts',(-54.3399714385998,-106.995532811273,
174.328630652215));
#29396=CARTESIAN_POINT('Ctrl Pts',(-55.4950050601995,-106.778117281995,
173.157057825983));
#29397=CARTESIAN_POINT('Ctrl Pts',(-56.6500386817991,-106.560701752718,
171.985484999752));
#29398=CARTESIAN_POINT('Ctrl Pts',(-58.2876193059689,-106.291843489121,
171.985485069079));
#29399=CARTESIAN_POINT('Ctrl Pts',(-59.9251999301388,-106.022985225524,
171.985485138407));
#29400=CARTESIAN_POINT('Ctrl Pts',(-61.0802334542465,-105.80556970664,173.157058062683));
#29401=CARTESIAN_POINT('Ctrl Pts',(-62.2352669783543,-105.588154187756,
174.328630986959));
#29402=CARTESIAN_POINT('Ctrl Pts',(-62.2253288465001,-105.494932430449,
175.985485236451));
#29403=CARTESIAN_POINT('Ctrl Pts',(-62.2153907146459,-105.401710673143,
177.642339485944));
#29404=CARTESIAN_POINT('Ctrl Pts',(-61.0404809672123,-105.43268267311,178.813912312176));
#29405=CARTESIAN_POINT('Ctrl Pts',(-59.8655712197787,-105.463654673077,
179.985485138407));
#29406=CARTESIAN_POINT('Ctrl Pts',(-58.2081144697748,-105.546069407363,
179.985485069079));
#29407=CARTESIAN_POINT('Ctrl Pts',(-56.5506577197709,-105.628484141649,
179.985484999752));
#29408=CARTESIAN_POINT('Ctrl Pts',(-55.3757480698291,-105.659456131223,
178.813912075476));
#29409=CARTESIAN_POINT('Ctrl Pts',(-54.2008384198873,-105.690428120796,
177.6423391512));
#29410=CARTESIAN_POINT('Ctrl Pts',(-54.1909004259075,-105.597206348792,
175.985484901707));
#29411=CARTESIAN_POINT('Ctrl Pts',(-54.1809624319276,-105.503984576787,
174.328630652215));
#29412=CARTESIAN_POINT('Ctrl Pts',(-55.3359960535272,-105.28656904751,173.157057825983));
#29413=CARTESIAN_POINT('Ctrl Pts',(-56.4910296751268,-105.069153518232,
171.985484999752));
#29414=CARTESIAN_POINT('Ctrl Pts',(-58.1286102992967,-104.800295254635,
171.985485069079));
#29415=CARTESIAN_POINT('Ctrl Pts',(-59.7661909234666,-104.531436991038,
171.985485138407));
#29416=CARTESIAN_POINT('Ctrl Pts',(-60.9212244475743,-104.314021472154,
173.157058062683));
#29417=CARTESIAN_POINT('Ctrl Pts',(-62.0762579716821,-104.09660595327,174.328630986959));
#29418=CARTESIAN_POINT('Ctrl Pts',(-62.0663198398279,-104.003384195964,
175.985485236451));
#29419=CARTESIAN_POINT('Ctrl Pts',(-62.0563817079737,-103.910162438658,
177.642339485944));
#29420=CARTESIAN_POINT('Ctrl Pts',(-60.8814719605401,-103.941134438624,
178.813912312176));
#29421=CARTESIAN_POINT('Ctrl Pts',(-59.7065622131064,-103.972106438591,
179.985485138407));
#29422=CARTESIAN_POINT('Ctrl Pts',(-58.0491054631025,-104.054521172878,
179.985485069079));
#29423=CARTESIAN_POINT('Ctrl Pts',(-56.3916487130987,-104.136935907164,
179.985484999752));
#29424=CARTESIAN_POINT('Ctrl Pts',(-55.2167390631569,-104.167907896737,
178.813912075476));
#29425=CARTESIAN_POINT('Ctrl Pts',(-54.0418294132151,-104.198879886311,
177.6423391512));
#29426=CARTESIAN_POINT('Ctrl Pts',(-54.0318914192353,-104.105658114306,
175.985484901707));
#29427=CARTESIAN_POINT('Ctrl Pts',(-54.0219534252554,-104.012436342302,
174.328630652215));
#29428=CARTESIAN_POINT('Ctrl Pts',(-55.176987046855,-103.795020813024,173.157057825983));
#29429=CARTESIAN_POINT('Ctrl Pts',(-56.3320206684546,-103.577605283747,
171.985484999752));
#29430=CARTESIAN_POINT('Ctrl Pts',(-57.9696012926245,-103.30874702015,171.985485069079));
#29431=CARTESIAN_POINT('Ctrl Pts',(-59.6071819167943,-103.039888756553,
171.985485138407));
#29432=CARTESIAN_POINT('Ctrl Pts',(-60.7622154409021,-102.822473237669,
173.157058062683));
#29433=CARTESIAN_POINT('Ctrl Pts',(-61.9172489650099,-102.605057718784,
174.328630986959));
#29434=CARTESIAN_POINT('Ctrl Pts',(-61.9073108331557,-102.511835961478,
175.985485236451));
#29435=CARTESIAN_POINT('Ctrl Pts',(-61.8973727013015,-102.418614204172,
177.642339485944));
#29436=CARTESIAN_POINT('Ctrl Pts',(-60.7224629538678,-102.449586204139,
178.813912312176));
#29437=CARTESIAN_POINT('Ctrl Pts',(-59.5475532064342,-102.480558204106,
179.985485138407));
#29438=CARTESIAN_POINT('Ctrl Pts',(-57.8900964564303,-102.562972938392,
179.985485069079));
#29439=CARTESIAN_POINT('Ctrl Pts',(-56.2326397064264,-102.645387672678,
179.985484999752));
#29440=CARTESIAN_POINT('Ctrl Pts',(-55.0577300564847,-102.676359662252,
178.813912075476));
#29441=CARTESIAN_POINT('Ctrl Pts',(-53.8828204065429,-102.707331651825,
177.6423391512));
#29442=CARTESIAN_POINT('Ctrl Pts',(-53.872882412563,-102.614109879821,175.985484901707));
#29443=CARTESIAN_POINT('Ctrl Pts',(-53.8629444185832,-102.520888107816,
174.328630652215));
#29444=CARTESIAN_POINT('Ctrl Pts',(-55.0179780401828,-102.303472578539,
173.157057825983));
#29445=CARTESIAN_POINT('Ctrl Pts',(-56.1730116617824,-102.086057049261,
171.985484999752));
#29446=CARTESIAN_POINT('Ctrl Pts',(-57.8105922859523,-101.817198785664,
171.985485069079));
#29447=CARTESIAN_POINT('Ctrl Pts',(-59.4481729101221,-101.548340522067,
171.985485138407));
#29448=CARTESIAN_POINT('Ctrl Pts',(-60.6032064342299,-101.330925003183,
173.157058062683));
#29449=CARTESIAN_POINT('Ctrl Pts',(-61.7582399583376,-101.113509484299,
174.328630986959));
#29450=CARTESIAN_POINT('Ctrl Pts',(-61.7483018264834,-101.020287726993,
175.985485236451));
#29451=CARTESIAN_POINT('Ctrl Pts',(-61.7383636946293,-100.927065969686,
177.642339485944));
#29452=CARTESIAN_POINT('Ctrl Pts',(-60.5634539471956,-100.958037969653,
178.813912312176));
#29453=CARTESIAN_POINT('Ctrl Pts',(-59.388544199762,-100.98900996962,179.985485138407));
#29454=CARTESIAN_POINT('Ctrl Pts',(-57.7310874497581,-101.071424703906,
179.985485069079));
#29455=CARTESIAN_POINT('Ctrl Pts',(-56.0736306997542,-101.153839438193,
179.985484999752));
#29456=CARTESIAN_POINT('Ctrl Pts',(-54.8987210498124,-101.184811427766,
178.813912075476));
#29457=CARTESIAN_POINT('Ctrl Pts',(-53.7238113998707,-101.21578341734,177.6423391512));
#29458=CARTESIAN_POINT('Ctrl Pts',(-53.7138734058908,-101.122561645335,
175.985484901707));
#29459=CARTESIAN_POINT('Ctrl Pts',(-53.7039354119109,-101.029339873331,
174.328630652215));
#29460=CARTESIAN_POINT('Ctrl Pts',(-54.8589690335105,-100.811924344053,
173.157057825983));
#29461=CARTESIAN_POINT('Ctrl Pts',(-56.0140026551102,-100.594508814776,
171.985484999752));
#29462=CARTESIAN_POINT('Ctrl Pts',(-57.65158327928,-100.325650551179,171.985485069079));
#29463=CARTESIAN_POINT('Ctrl Pts',(-59.2891639034499,-100.056792287582,
171.985485138407));
#29464=CARTESIAN_POINT('Ctrl Pts',(-60.4441974275576,-99.8393767686974,
173.157058062683));
#29465=CARTESIAN_POINT('Ctrl Pts',(-61.5992309516654,-99.6219612498133,
174.328630986959));
#29466=CARTESIAN_POINT('Ctrl Pts',(-61.5892928198112,-99.528739492507,175.985485236451));
#29467=CARTESIAN_POINT('Ctrl Pts',(-61.579354687957,-99.4355177352008,177.642339485944));
#29468=CARTESIAN_POINT('Ctrl Pts',(-60.4044449405234,-99.4664897351676,
178.813912312176));
#29469=CARTESIAN_POINT('Ctrl Pts',(-59.2295351930898,-99.4974617351344,
179.985485138407));
#29470=CARTESIAN_POINT('Ctrl Pts',(-57.5720784430859,-99.5798764694207,
179.985485069079));
#29471=CARTESIAN_POINT('Ctrl Pts',(-55.914621693082,-99.662291203707,179.985484999752));
#29472=CARTESIAN_POINT('Ctrl Pts',(-54.7397120431402,-99.6932631932805,
178.813912075476));
#29473=CARTESIAN_POINT('Ctrl Pts',(-53.5648023931984,-99.724235182854,177.6423391512));
#29474=CARTESIAN_POINT('Ctrl Pts',(-53.5548643992186,-99.6310134108495,
175.985484901707));
#29475=CARTESIAN_POINT('Ctrl Pts',(-53.5449264052387,-99.5377916388449,
174.328630652215));
#29476=CARTESIAN_POINT('Ctrl Pts',(-54.6999600268383,-99.3203761095675,
173.157057825983));
#29477=CARTESIAN_POINT('Ctrl Pts',(-55.8549936484379,-99.10296058029,171.985484999752));
#29478=CARTESIAN_POINT('Ctrl Pts',(-57.4925742726078,-98.834102316693,171.985485069079));
#29479=CARTESIAN_POINT('Ctrl Pts',(-59.1301548967777,-98.5652440530961,
171.985485138407));
#29480=CARTESIAN_POINT('Ctrl Pts',(-60.2851884208854,-98.3478285342118,
173.157058062683));
#29481=CARTESIAN_POINT('Ctrl Pts',(-61.4402219449932,-98.1304130153276,
174.328630986959));
#29482=CARTESIAN_POINT('Ctrl Pts',(-61.430283813139,-98.0371912580215,175.985485236451));
#29483=CARTESIAN_POINT('Ctrl Pts',(-61.4203456812848,-97.9439695007152,
177.642339485944));
#29484=CARTESIAN_POINT('Ctrl Pts',(-60.2454359338512,-97.974941500682,178.813912312176));
#29485=CARTESIAN_POINT('Ctrl Pts',(-59.0705261864175,-98.0059135006488,
179.985485138407));
#29486=CARTESIAN_POINT('Ctrl Pts',(-57.4130694364136,-98.0883282349351,
179.985485069079));
#29487=CARTESIAN_POINT('Ctrl Pts',(-55.7556126864097,-98.1707429692214,
179.985484999752));
#29488=CARTESIAN_POINT('Ctrl Pts',(-54.580703036468,-98.2017149587949,178.813912075476));
#29489=CARTESIAN_POINT('Ctrl Pts',(-56.181115489574,-113.283598570176,178.821287383467));
#29490=CARTESIAN_POINT('Ctrl Pts',(-55.0031681001975,-113.314894403068,
177.646659506339));
#29491=CARTESIAN_POINT('Ctrl Pts',(-54.9932301063974,-113.221672631044,
175.985484901271));
#29492=CARTESIAN_POINT('Ctrl Pts',(-54.9832921125973,-113.12845085902,174.324310296203));
#29493=CARTESIAN_POINT('Ctrl Pts',(-56.1413634738858,-112.910711486397,
173.149682517375));
#29494=CARTESIAN_POINT('Ctrl Pts',(-57.2994348351743,-112.692972113774,
171.975054738546));
#29495=CARTESIAN_POINT('Ctrl Pts',(-58.9413114718314,-112.423655866545,
171.975054808055));
#29496=CARTESIAN_POINT('Ctrl Pts',(-60.5831881084886,-112.154339619316,
171.975054877564));
#29497=CARTESIAN_POINT('Ctrl Pts',(-61.741259372031,-111.936600257113,173.149682754692));
#29498=CARTESIAN_POINT('Ctrl Pts',(-62.8993306355734,-111.71886089491,174.32431063182));
#29499=CARTESIAN_POINT('Ctrl Pts',(-62.8893925035395,-111.625639137623,
175.985485236888));
#29500=CARTESIAN_POINT('Ctrl Pts',(-62.8794543715055,-111.532417380336,
177.646659841956));
#29501=CARTESIAN_POINT('Ctrl Pts',(-61.701506884383,-111.563713223648,178.821287620784));
#29502=CARTESIAN_POINT('Ctrl Pts',(-60.5235593972605,-111.595009066961,
179.995915399612));
#29503=CARTESIAN_POINT('Ctrl Pts',(-58.8618066347693,-111.677881784879,
179.995915330104));
#29504=CARTESIAN_POINT('Ctrl Pts',(-57.2000538722782,-111.760754502798,
179.995915260595));
#29505=CARTESIAN_POINT('Ctrl Pts',(-56.0221064829017,-111.79205033569,178.821287383467));
#29506=CARTESIAN_POINT('Ctrl Pts',(-54.8441590935253,-111.823346168582,
177.646659506339));
#29507=CARTESIAN_POINT('Ctrl Pts',(-54.8342210997252,-111.730124396559,
175.985484901271));
#29508=CARTESIAN_POINT('Ctrl Pts',(-54.8242831059251,-111.636902624535,
174.324310296203));
#29509=CARTESIAN_POINT('Ctrl Pts',(-55.9823544672136,-111.419163251912,
173.149682517375));
#29510=CARTESIAN_POINT('Ctrl Pts',(-57.1404258285021,-111.201423879289,
171.975054738546));
#29511=CARTESIAN_POINT('Ctrl Pts',(-58.7823024651592,-110.932107632059,
171.975054808055));
#29512=CARTESIAN_POINT('Ctrl Pts',(-60.4241791018163,-110.66279138483,171.975054877564));
#29513=CARTESIAN_POINT('Ctrl Pts',(-61.5822503653587,-110.445052022627,
173.149682754692));
#29514=CARTESIAN_POINT('Ctrl Pts',(-62.7403216289012,-110.227312660424,
174.32431063182));
#29515=CARTESIAN_POINT('Ctrl Pts',(-62.7303834968672,-110.134090903137,
175.985485236888));
#29516=CARTESIAN_POINT('Ctrl Pts',(-62.7204453648333,-110.04086914585,177.646659841956));
#29517=CARTESIAN_POINT('Ctrl Pts',(-61.5424978777108,-110.072164989163,
178.821287620784));
#29518=CARTESIAN_POINT('Ctrl Pts',(-60.3645503905882,-110.103460832475,
179.995915399612));
#29519=CARTESIAN_POINT('Ctrl Pts',(-58.7027976280971,-110.186333550394,
179.995915330104));
#29520=CARTESIAN_POINT('Ctrl Pts',(-57.041044865606,-110.269206268313,179.995915260595));
#29521=CARTESIAN_POINT('Ctrl Pts',(-55.8630974762295,-110.300502101205,
178.821287383467));
#29522=CARTESIAN_POINT('Ctrl Pts',(-54.6851500868531,-110.331797934097,
177.646659506339));
#29523=CARTESIAN_POINT('Ctrl Pts',(-54.675212093053,-110.238576162073,175.985484901271));
#29524=CARTESIAN_POINT('Ctrl Pts',(-54.6652740992529,-110.145354390049,
174.324310296203));
#29525=CARTESIAN_POINT('Ctrl Pts',(-55.8233454605414,-109.927615017426,
173.149682517375));
#29526=CARTESIAN_POINT('Ctrl Pts',(-56.9814168218299,-109.709875644803,
171.975054738546));
#29527=CARTESIAN_POINT('Ctrl Pts',(-58.623293458487,-109.440559397574,171.975054808055));
#29528=CARTESIAN_POINT('Ctrl Pts',(-60.2651700951441,-109.171243150344,
171.975054877564));
#29529=CARTESIAN_POINT('Ctrl Pts',(-61.4232413586865,-108.953503788142,
173.149682754692));
#29530=CARTESIAN_POINT('Ctrl Pts',(-62.581312622229,-108.735764425939,174.32431063182));
#29531=CARTESIAN_POINT('Ctrl Pts',(-62.571374490195,-108.642542668652,175.985485236888));
#29532=CARTESIAN_POINT('Ctrl Pts',(-62.5614363581611,-108.549320911365,
177.646659841956));
#29533=CARTESIAN_POINT('Ctrl Pts',(-61.3834888710385,-108.580616754677,
178.821287620784));
#29534=CARTESIAN_POINT('Ctrl Pts',(-60.205541383916,-108.61191259799,179.995915399612));
#29535=CARTESIAN_POINT('Ctrl Pts',(-58.5437886214249,-108.694785315908,
179.995915330104));
#29536=CARTESIAN_POINT('Ctrl Pts',(-56.8820358589338,-108.777658033827,
179.995915260595));
#29537=CARTESIAN_POINT('Ctrl Pts',(-55.7040884695573,-108.808953866719,
178.821287383467));
#29538=CARTESIAN_POINT('Ctrl Pts',(-54.5261410801808,-108.840249699611,
177.646659506339));
#29539=CARTESIAN_POINT('Ctrl Pts',(-54.5162030863807,-108.747027927587,
175.985484901271));
#29540=CARTESIAN_POINT('Ctrl Pts',(-54.5062650925806,-108.653806155564,
174.324310296203));
#29541=CARTESIAN_POINT('Ctrl Pts',(-55.6643364538691,-108.436066782941,
173.149682517375));
#29542=CARTESIAN_POINT('Ctrl Pts',(-56.8224078151577,-108.218327410317,
171.975054738546));
#29543=CARTESIAN_POINT('Ctrl Pts',(-58.4642844518147,-107.949011163088,
171.975054808055));
#29544=CARTESIAN_POINT('Ctrl Pts',(-60.1061610884719,-107.679694915859,
171.975054877564));
#29545=CARTESIAN_POINT('Ctrl Pts',(-61.2642323520143,-107.461955553656,
173.149682754692));
#29546=CARTESIAN_POINT('Ctrl Pts',(-62.4223036155567,-107.244216191453,
174.32431063182));
#29547=CARTESIAN_POINT('Ctrl Pts',(-62.4123654835228,-107.150994434166,
175.985485236888));
#29548=CARTESIAN_POINT('Ctrl Pts',(-62.4024273514889,-107.057772676879,
177.646659841956));
#29549=CARTESIAN_POINT('Ctrl Pts',(-61.2244798643663,-107.089068520192,
178.821287620784));
#29550=CARTESIAN_POINT('Ctrl Pts',(-60.0465323772438,-107.120364363504,
179.995915399612));
#29551=CARTESIAN_POINT('Ctrl Pts',(-58.3847796147526,-107.203237081423,
179.995915330104));
#29552=CARTESIAN_POINT('Ctrl Pts',(-56.7230268522615,-107.286109799341,
179.995915260595));
#29553=CARTESIAN_POINT('Ctrl Pts',(-55.5450794628851,-107.317405632233,
178.821287383467));
#29554=CARTESIAN_POINT('Ctrl Pts',(-54.3671320735086,-107.348701465125,
177.646659506339));
#29555=CARTESIAN_POINT('Ctrl Pts',(-54.3571940797085,-107.255479693102,
175.985484901271));
#29556=CARTESIAN_POINT('Ctrl Pts',(-54.3472560859084,-107.162257921078,
174.324310296203));
#29557=CARTESIAN_POINT('Ctrl Pts',(-55.5053274471969,-106.944518548455,
173.149682517375));
#29558=CARTESIAN_POINT('Ctrl Pts',(-56.6633988084854,-106.726779175832,
171.975054738546));
#29559=CARTESIAN_POINT('Ctrl Pts',(-58.3052754451425,-106.457462928602,
171.975054808055));
#29560=CARTESIAN_POINT('Ctrl Pts',(-59.9471520817997,-106.188146681373,
171.975054877564));
#29561=CARTESIAN_POINT('Ctrl Pts',(-61.1052233453421,-105.97040731917,173.149682754692));
#29562=CARTESIAN_POINT('Ctrl Pts',(-62.2632946088845,-105.752667956968,
174.32431063182));
#29563=CARTESIAN_POINT('Ctrl Pts',(-62.2533564768505,-105.659446199681,
175.985485236888));
#29564=CARTESIAN_POINT('Ctrl Pts',(-62.2434183448166,-105.566224442394,
177.646659841956));
#29565=CARTESIAN_POINT('Ctrl Pts',(-61.0654708576941,-105.597520285706,
178.821287620784));
#29566=CARTESIAN_POINT('Ctrl Pts',(-59.8875233705716,-105.628816129018,
179.995915399612));
#29567=CARTESIAN_POINT('Ctrl Pts',(-58.2257706080804,-105.711688846937,
179.995915330104));
#29568=CARTESIAN_POINT('Ctrl Pts',(-56.5640178455893,-105.794561564856,
179.995915260595));
#29569=CARTESIAN_POINT('Ctrl Pts',(-55.3860704562128,-105.825857397748,
178.821287383467));
#29570=CARTESIAN_POINT('Ctrl Pts',(-54.2081230668364,-105.85715323064,177.646659506339));
#29571=CARTESIAN_POINT('Ctrl Pts',(-54.1981850730363,-105.763931458616,
175.985484901271));
#29572=CARTESIAN_POINT('Ctrl Pts',(-54.1882470792362,-105.670709686593,
174.324310296203));
#29573=CARTESIAN_POINT('Ctrl Pts',(-55.3463184405247,-105.452970313969,
173.149682517375));
#29574=CARTESIAN_POINT('Ctrl Pts',(-56.5043898018132,-105.235230941346,
171.975054738546));
#29575=CARTESIAN_POINT('Ctrl Pts',(-58.1462664384703,-104.965914694117,
171.975054808055));
#29576=CARTESIAN_POINT('Ctrl Pts',(-59.7881430751274,-104.696598446888,
171.975054877564));
#29577=CARTESIAN_POINT('Ctrl Pts',(-60.9462143386698,-104.478859084685,
173.149682754692));
#29578=CARTESIAN_POINT('Ctrl Pts',(-62.1042856022123,-104.261119722482,
174.32431063182));
#29579=CARTESIAN_POINT('Ctrl Pts',(-62.0943474701783,-104.167897965195,
175.985485236888));
#29580=CARTESIAN_POINT('Ctrl Pts',(-62.0844093381444,-104.074676207908,
177.646659841956));
#29581=CARTESIAN_POINT('Ctrl Pts',(-60.9064618510219,-104.10597205122,178.821287620784));
#29582=CARTESIAN_POINT('Ctrl Pts',(-59.7285143638993,-104.137267894533,
179.995915399612));
#29583=CARTESIAN_POINT('Ctrl Pts',(-58.0667616014082,-104.220140612451,
179.995915330104));
#29584=CARTESIAN_POINT('Ctrl Pts',(-56.4050088389171,-104.30301333037,179.995915260595));
#29585=CARTESIAN_POINT('Ctrl Pts',(-55.2270614495406,-104.334309163262,
178.821287383467));
#29586=CARTESIAN_POINT('Ctrl Pts',(-54.0491140601642,-104.365604996154,
177.646659506339));
#29587=CARTESIAN_POINT('Ctrl Pts',(-54.039176066364,-104.272383224131,175.985484901271));
#29588=CARTESIAN_POINT('Ctrl Pts',(-54.029238072564,-104.179161452107,174.324310296203));
#29589=CARTESIAN_POINT('Ctrl Pts',(-55.1873094338524,-103.961422079484,
173.149682517375));
#29590=CARTESIAN_POINT('Ctrl Pts',(-56.345380795141,-103.743682706861,171.975054738546));
#29591=CARTESIAN_POINT('Ctrl Pts',(-57.9872574317981,-103.474366459631,
171.975054808055));
#29592=CARTESIAN_POINT('Ctrl Pts',(-59.6291340684552,-103.205050212402,
171.975054877564));
#29593=CARTESIAN_POINT('Ctrl Pts',(-60.7872053319976,-102.987310850199,
173.149682754692));
#29594=CARTESIAN_POINT('Ctrl Pts',(-61.94527659554,-102.769571487996,174.32431063182));
#29595=CARTESIAN_POINT('Ctrl Pts',(-61.9353384635061,-102.676349730709,
175.985485236888));
#29596=CARTESIAN_POINT('Ctrl Pts',(-61.9254003314722,-102.583127973422,
177.646659841956));
#29597=CARTESIAN_POINT('Ctrl Pts',(-60.7474528443496,-102.614423816735,
178.821287620784));
#29598=CARTESIAN_POINT('Ctrl Pts',(-59.5695053572271,-102.645719660047,
179.995915399612));
#29599=CARTESIAN_POINT('Ctrl Pts',(-57.907752594736,-102.728592377966,179.995915330104));
#29600=CARTESIAN_POINT('Ctrl Pts',(-56.2459998322448,-102.811465095885,
179.995915260595));
#29601=CARTESIAN_POINT('Ctrl Pts',(-55.0680524428684,-102.842760928777,
178.821287383467));
#29602=CARTESIAN_POINT('Ctrl Pts',(-53.8901050534919,-102.874056761669,
177.646659506339));
#29603=CARTESIAN_POINT('Ctrl Pts',(-53.8801670596918,-102.780834989645,
175.985484901271));
#29604=CARTESIAN_POINT('Ctrl Pts',(-53.8702290658917,-102.687613217621,
174.324310296203));
#29605=CARTESIAN_POINT('Ctrl Pts',(-55.0283004271802,-102.469873844998,
173.149682517375));
#29606=CARTESIAN_POINT('Ctrl Pts',(-56.1863717884687,-102.252134472375,
171.975054738546));
#29607=CARTESIAN_POINT('Ctrl Pts',(-57.8282484251258,-101.982818225146,
171.975054808055));
#29608=CARTESIAN_POINT('Ctrl Pts',(-59.470125061783,-101.713501977916,171.975054877564));
#29609=CARTESIAN_POINT('Ctrl Pts',(-60.6281963253254,-101.495762615714,
173.149682754692));
#29610=CARTESIAN_POINT('Ctrl Pts',(-61.7862675888678,-101.278023253511,
174.32431063182));
#29611=CARTESIAN_POINT('Ctrl Pts',(-61.7763294568339,-101.184801496224,
175.985485236888));
#29612=CARTESIAN_POINT('Ctrl Pts',(-61.7663913247999,-101.091579738937,
177.646659841956));
#29613=CARTESIAN_POINT('Ctrl Pts',(-60.5884438376774,-101.122875582249,
178.821287620784));
#29614=CARTESIAN_POINT('Ctrl Pts',(-59.4104963505549,-101.154171425562,
179.995915399612));
#29615=CARTESIAN_POINT('Ctrl Pts',(-57.7487435880637,-101.23704414348,179.995915330104));
#29616=CARTESIAN_POINT('Ctrl Pts',(-56.0869908255726,-101.319916861399,
179.995915260595));
#29617=CARTESIAN_POINT('Ctrl Pts',(-54.9090434361961,-101.351212694291,
178.821287383467));
#29618=CARTESIAN_POINT('Ctrl Pts',(-53.7310960468197,-101.382508527183,
177.646659506339));
#29619=CARTESIAN_POINT('Ctrl Pts',(-53.7211580530196,-101.289286755159,
175.985484901271));
#29620=CARTESIAN_POINT('Ctrl Pts',(-53.7112200592195,-101.196064983136,
174.324310296203));
#29621=CARTESIAN_POINT('Ctrl Pts',(-54.869291420508,-100.978325610513,173.149682517375));
#29622=CARTESIAN_POINT('Ctrl Pts',(-56.0273627817965,-100.760586237889,
171.975054738546));
#29623=CARTESIAN_POINT('Ctrl Pts',(-57.6692394184536,-100.49126999066,171.975054808055));
#29624=CARTESIAN_POINT('Ctrl Pts',(-59.3111160551107,-100.221953743431,
171.975054877564));
#29625=CARTESIAN_POINT('Ctrl Pts',(-60.4691873186531,-100.004214381228,
173.149682754692));
#29626=CARTESIAN_POINT('Ctrl Pts',(-61.6272585821956,-99.7864750190253,
174.32431063182));
#29627=CARTESIAN_POINT('Ctrl Pts',(-61.6173204501616,-99.6932532617382,
175.985485236888));
#29628=CARTESIAN_POINT('Ctrl Pts',(-61.6073823181277,-99.6000315044512,
177.646659841956));
#29629=CARTESIAN_POINT('Ctrl Pts',(-60.4294348310052,-99.6313273477637,
178.821287620784));
#29630=CARTESIAN_POINT('Ctrl Pts',(-59.2514873438827,-99.6626231910761,
179.995915399612));
#29631=CARTESIAN_POINT('Ctrl Pts',(-57.5897345813915,-99.7454959089947,
179.995915330104));
#29632=CARTESIAN_POINT('Ctrl Pts',(-55.9279818189004,-99.8283686269133,
179.995915260595));
#29633=CARTESIAN_POINT('Ctrl Pts',(-54.7500344295239,-99.8596644598054,
178.821287383467));
#29634=CARTESIAN_POINT('Ctrl Pts',(-53.5720870401475,-99.8909602926975,
177.646659506339));
#29635=CARTESIAN_POINT('Ctrl Pts',(-53.5621490463474,-99.7977385206737,
175.985484901271));
#29636=CARTESIAN_POINT('Ctrl Pts',(-53.5522110525473,-99.7045167486501,
174.324310296203));
#29637=CARTESIAN_POINT('Ctrl Pts',(-54.7102824138358,-99.4867773760269,
173.149682517375));
#29638=CARTESIAN_POINT('Ctrl Pts',(-55.8683537751243,-99.2690380034038,
171.975054738546));
#29639=CARTESIAN_POINT('Ctrl Pts',(-57.5102304117814,-98.9997217561745,
171.975054808055));
#29640=CARTESIAN_POINT('Ctrl Pts',(-59.1521070484385,-98.7304055089452,
171.975054877564));
#29641=CARTESIAN_POINT('Ctrl Pts',(-60.3101783119809,-98.5126661467424,
173.149682754692));
#29642=CARTESIAN_POINT('Ctrl Pts',(-61.4682495755234,-98.2949267845397,
174.32431063182));
#29643=CARTESIAN_POINT('Ctrl Pts',(-61.4583114434894,-98.2017050272526,
175.985485236888));
#29644=CARTESIAN_POINT('Ctrl Pts',(-61.4483733114555,-98.1084832699656,
177.646659841956));
#29645=CARTESIAN_POINT('Ctrl Pts',(-60.2704258243329,-98.139779113278,178.821287620784));
#29646=CARTESIAN_POINT('Ctrl Pts',(-59.0924783372104,-98.1710749565905,
179.995915399612));
#29647=CARTESIAN_POINT('Ctrl Pts',(-57.4307255747193,-98.2539476745091,
179.995915330104));
#29648=CARTESIAN_POINT('Ctrl Pts',(-55.7689728122282,-98.3368203924277,
179.995915260595));
#29649=CARTESIAN_POINT('Ctrl Pts',(-54.5910254228517,-98.3681162253198,
178.821287383467));
#29650=CARTESIAN_POINT('Ctrl Pts',(-56.1988062143188,-113.449542435949,
178.821287383467));
#29651=CARTESIAN_POINT('Ctrl Pts',(-55.0208588249424,-113.480838268841,
177.646659506339));
#29652=CARTESIAN_POINT('Ctrl Pts',(-55.0109208311422,-113.387616496817,
175.985484901271));
#29653=CARTESIAN_POINT('Ctrl Pts',(-55.0009828373422,-113.294394724794,
174.324310296203));
#29654=CARTESIAN_POINT('Ctrl Pts',(-56.1590541986307,-113.07665535217,173.149682517375));
#29655=CARTESIAN_POINT('Ctrl Pts',(-57.3171255599192,-112.858915979547,
171.975054738546));
#29656=CARTESIAN_POINT('Ctrl Pts',(-58.9590021965763,-112.589599732318,
171.975054808055));
#29657=CARTESIAN_POINT('Ctrl Pts',(-60.6008788332334,-112.320283485089,
171.975054877564));
#29658=CARTESIAN_POINT('Ctrl Pts',(-61.7589500967758,-112.102544122886,
173.149682754692));
#29659=CARTESIAN_POINT('Ctrl Pts',(-62.9170213603182,-111.884804760683,
174.32431063182));
#29660=CARTESIAN_POINT('Ctrl Pts',(-62.9070832282843,-111.791583003396,
175.985485236888));
#29661=CARTESIAN_POINT('Ctrl Pts',(-62.8971450962504,-111.698361246109,
177.646659841956));
#29662=CARTESIAN_POINT('Ctrl Pts',(-61.7191976091278,-111.729657089422,
178.821287620784));
#29663=CARTESIAN_POINT('Ctrl Pts',(-60.5412501220053,-111.760952932734,
179.995915399612));
#29664=CARTESIAN_POINT('Ctrl Pts',(-58.8794973595142,-111.843825650653,
179.995915330104));
#29665=CARTESIAN_POINT('Ctrl Pts',(-57.217744597023,-111.926698368571,179.995915260595));
#29666=CARTESIAN_POINT('Ctrl Pts',(-56.0397972076466,-111.957994201463,
178.821287383467));
#29667=CARTESIAN_POINT('Ctrl Pts',(-54.8618498182701,-111.989290034355,
177.646659506339));
#29668=CARTESIAN_POINT('Ctrl Pts',(-54.85191182447,-111.896068262332,175.985484901271));
#29669=CARTESIAN_POINT('Ctrl Pts',(-54.8419738306699,-111.802846490308,
174.324310296203));
#29670=CARTESIAN_POINT('Ctrl Pts',(-56.0000451919584,-111.585107117685,
173.149682517375));
#29671=CARTESIAN_POINT('Ctrl Pts',(-57.158116553247,-111.367367745062,171.975054738546));
#29672=CARTESIAN_POINT('Ctrl Pts',(-58.799993189904,-111.098051497832,171.975054808055));
#29673=CARTESIAN_POINT('Ctrl Pts',(-60.4418698265612,-110.828735250603,
171.975054877564));
#29674=CARTESIAN_POINT('Ctrl Pts',(-61.5999410901036,-110.6109958884,173.149682754692));
#29675=CARTESIAN_POINT('Ctrl Pts',(-62.758012353646,-110.393256526198,174.32431063182));
#29676=CARTESIAN_POINT('Ctrl Pts',(-62.7480742216121,-110.30003476891,175.985485236888));
#29677=CARTESIAN_POINT('Ctrl Pts',(-62.7381360895782,-110.206813011623,
177.646659841956));
#29678=CARTESIAN_POINT('Ctrl Pts',(-61.5601886024556,-110.238108854936,
178.821287620784));
#29679=CARTESIAN_POINT('Ctrl Pts',(-60.3822411153331,-110.269404698248,
179.995915399612));
#29680=CARTESIAN_POINT('Ctrl Pts',(-58.7204883528419,-110.352277416167,
179.995915330104));
#29681=CARTESIAN_POINT('Ctrl Pts',(-57.0587355903508,-110.435150134086,
179.995915260595));
#29682=CARTESIAN_POINT('Ctrl Pts',(-55.8807882009743,-110.466445966978,
178.821287383467));
#29683=CARTESIAN_POINT('Ctrl Pts',(-54.7028408115979,-110.49774179987,177.646659506339));
#29684=CARTESIAN_POINT('Ctrl Pts',(-54.6929028177978,-110.404520027846,
175.985484901271));
#29685=CARTESIAN_POINT('Ctrl Pts',(-54.6829648239977,-110.311298255822,
174.324310296203));
#29686=CARTESIAN_POINT('Ctrl Pts',(-55.8410361852862,-110.093558883199,
173.149682517375));
#29687=CARTESIAN_POINT('Ctrl Pts',(-56.9991075465747,-109.875819510576,
171.975054738546));
#29688=CARTESIAN_POINT('Ctrl Pts',(-58.6409841832318,-109.606503263347,
171.975054808055));
#29689=CARTESIAN_POINT('Ctrl Pts',(-60.2828608198889,-109.337187016117,
171.975054877564));
#29690=CARTESIAN_POINT('Ctrl Pts',(-61.4409320834313,-109.119447653915,
173.149682754692));
#29691=CARTESIAN_POINT('Ctrl Pts',(-62.5990033469738,-108.901708291712,
174.32431063182));
#29692=CARTESIAN_POINT('Ctrl Pts',(-62.5890652149398,-108.808486534425,
175.985485236888));
#29693=CARTESIAN_POINT('Ctrl Pts',(-62.5791270829059,-108.715264777138,
177.646659841956));
#29694=CARTESIAN_POINT('Ctrl Pts',(-61.4011795957834,-108.74656062045,178.821287620784));
#29695=CARTESIAN_POINT('Ctrl Pts',(-60.2232321086609,-108.777856463763,
179.995915399612));
#29696=CARTESIAN_POINT('Ctrl Pts',(-58.5614793461697,-108.860729181681,
179.995915330104));
#29697=CARTESIAN_POINT('Ctrl Pts',(-56.8997265836786,-108.9436018996,179.995915260595));
#29698=CARTESIAN_POINT('Ctrl Pts',(-55.7217791943021,-108.974897732492,
178.821287383467));
#29699=CARTESIAN_POINT('Ctrl Pts',(-54.5438318049257,-109.006193565384,
177.646659506339));
#29700=CARTESIAN_POINT('Ctrl Pts',(-54.5338938111256,-108.91297179336,175.985484901271));
#29701=CARTESIAN_POINT('Ctrl Pts',(-54.5239558173255,-108.819750021337,
174.324310296203));
#29702=CARTESIAN_POINT('Ctrl Pts',(-55.682027178614,-108.602010648714,173.149682517375));
#29703=CARTESIAN_POINT('Ctrl Pts',(-56.8400985399025,-108.384271276091,
171.975054738546));
#29704=CARTESIAN_POINT('Ctrl Pts',(-58.4819751765596,-108.114955028861,
171.975054808055));
#29705=CARTESIAN_POINT('Ctrl Pts',(-60.1238518132167,-107.845638781632,
171.975054877564));
#29706=CARTESIAN_POINT('Ctrl Pts',(-61.2819230767591,-107.627899419429,
173.149682754692));
#29707=CARTESIAN_POINT('Ctrl Pts',(-62.4399943403016,-107.410160057226,
174.32431063182));
#29708=CARTESIAN_POINT('Ctrl Pts',(-62.4300562082676,-107.316938299939,
175.985485236888));
#29709=CARTESIAN_POINT('Ctrl Pts',(-62.4201180762337,-107.223716542652,
177.646659841956));
#29710=CARTESIAN_POINT('Ctrl Pts',(-61.2421705891111,-107.255012385965,
178.821287620784));
#29711=CARTESIAN_POINT('Ctrl Pts',(-60.0642231019886,-107.286308229277,
179.995915399612));
#29712=CARTESIAN_POINT('Ctrl Pts',(-58.4024703394975,-107.369180947196,
179.995915330104));
#29713=CARTESIAN_POINT('Ctrl Pts',(-56.7407175770064,-107.452053665114,
179.995915260595));
#29714=CARTESIAN_POINT('Ctrl Pts',(-55.5627701876299,-107.483349498006,
178.821287383467));
#29715=CARTESIAN_POINT('Ctrl Pts',(-54.3848227982534,-107.514645330899,
177.646659506339));
#29716=CARTESIAN_POINT('Ctrl Pts',(-54.3748848044533,-107.421423558875,
175.985484901271));
#29717=CARTESIAN_POINT('Ctrl Pts',(-54.3649468106533,-107.328201786851,
174.324310296203));
#29718=CARTESIAN_POINT('Ctrl Pts',(-55.5230181719417,-107.110462414228,
173.149682517375));
#29719=CARTESIAN_POINT('Ctrl Pts',(-56.6810895332303,-106.892723041605,
171.975054738546));
#29720=CARTESIAN_POINT('Ctrl Pts',(-58.3229661698874,-106.623406794376,
171.975054808055));
#29721=CARTESIAN_POINT('Ctrl Pts',(-59.9648428065445,-106.354090547146,
171.975054877564));
#29722=CARTESIAN_POINT('Ctrl Pts',(-61.1229140700869,-106.136351184943,
173.149682754692));
#29723=CARTESIAN_POINT('Ctrl Pts',(-62.2809853336293,-105.918611822741,
174.32431063182));
#29724=CARTESIAN_POINT('Ctrl Pts',(-62.2710472015954,-105.825390065454,
175.985485236888));
#29725=CARTESIAN_POINT('Ctrl Pts',(-62.2611090695615,-105.732168308167,
177.646659841956));
#29726=CARTESIAN_POINT('Ctrl Pts',(-61.0831615824389,-105.763464151479,
178.821287620784));
#29727=CARTESIAN_POINT('Ctrl Pts',(-59.9052140953164,-105.794759994792,
179.995915399612));
#29728=CARTESIAN_POINT('Ctrl Pts',(-58.2434613328252,-105.87763271271,179.995915330104));
#29729=CARTESIAN_POINT('Ctrl Pts',(-56.5817085703341,-105.960505430629,
179.995915260595));
#29730=CARTESIAN_POINT('Ctrl Pts',(-55.4037611809577,-105.991801263521,
178.821287383467));
#29731=CARTESIAN_POINT('Ctrl Pts',(-54.2258137915812,-106.023097096413,
177.646659506339));
#29732=CARTESIAN_POINT('Ctrl Pts',(-54.2158757977811,-105.929875324389,
175.985484901271));
#29733=CARTESIAN_POINT('Ctrl Pts',(-54.205937803981,-105.836653552366,174.324310296203));
#29734=CARTESIAN_POINT('Ctrl Pts',(-55.3640091652695,-105.618914179742,
173.149682517375));
#29735=CARTESIAN_POINT('Ctrl Pts',(-56.522080526558,-105.401174807119,171.975054738546));
#29736=CARTESIAN_POINT('Ctrl Pts',(-58.1639571632151,-105.13185855989,171.975054808055));
#29737=CARTESIAN_POINT('Ctrl Pts',(-59.8058337998722,-104.862542312661,
171.975054877564));
#29738=CARTESIAN_POINT('Ctrl Pts',(-60.9639050634147,-104.644802950458,
173.149682754692));
#29739=CARTESIAN_POINT('Ctrl Pts',(-62.1219763269571,-104.427063588255,
174.32431063182));
#29740=CARTESIAN_POINT('Ctrl Pts',(-62.1120381949232,-104.333841830968,
175.985485236888));
#29741=CARTESIAN_POINT('Ctrl Pts',(-62.1021000628892,-104.240620073681,
177.646659841956));
#29742=CARTESIAN_POINT('Ctrl Pts',(-60.9241525757667,-104.271915916993,
178.821287620784));
#29743=CARTESIAN_POINT('Ctrl Pts',(-59.7462050886442,-104.303211760306,
179.995915399612));
#29744=CARTESIAN_POINT('Ctrl Pts',(-58.084452326153,-104.386084478225,179.995915330104));
#29745=CARTESIAN_POINT('Ctrl Pts',(-56.4226995636619,-104.468957196143,
179.995915260595));
#29746=CARTESIAN_POINT('Ctrl Pts',(-55.2447521742854,-104.500253029035,
178.821287383467));
#29747=CARTESIAN_POINT('Ctrl Pts',(-54.066804784909,-104.531548861927,177.646659506339));
#29748=CARTESIAN_POINT('Ctrl Pts',(-54.0568667911089,-104.438327089904,
175.985484901271));
#29749=CARTESIAN_POINT('Ctrl Pts',(-54.0469287973088,-104.34510531788,174.324310296203));
#29750=CARTESIAN_POINT('Ctrl Pts',(-55.2050001585973,-104.127365945257,
173.149682517375));
#29751=CARTESIAN_POINT('Ctrl Pts',(-56.3630715198858,-103.909626572634,
171.975054738546));
#29752=CARTESIAN_POINT('Ctrl Pts',(-58.0049481565429,-103.640310325404,
171.975054808055));
#29753=CARTESIAN_POINT('Ctrl Pts',(-59.6468247932,-103.370994078175,171.975054877564));
#29754=CARTESIAN_POINT('Ctrl Pts',(-60.8048960567424,-103.153254715972,
173.149682754692));
#29755=CARTESIAN_POINT('Ctrl Pts',(-61.9629673202849,-102.93551535377,174.32431063182));
#29756=CARTESIAN_POINT('Ctrl Pts',(-61.9530291882509,-102.842293596483,
175.985485236888));
#29757=CARTESIAN_POINT('Ctrl Pts',(-61.943091056217,-102.749071839196,177.646659841956));
#29758=CARTESIAN_POINT('Ctrl Pts',(-60.7651435690945,-102.780367682508,
178.821287620784));
#29759=CARTESIAN_POINT('Ctrl Pts',(-59.587196081972,-102.81166352582,179.995915399612));
#29760=CARTESIAN_POINT('Ctrl Pts',(-57.9254433194808,-102.894536243739,
179.995915330104));
#29761=CARTESIAN_POINT('Ctrl Pts',(-56.2636905569897,-102.977408961658,
179.995915260595));
#29762=CARTESIAN_POINT('Ctrl Pts',(-55.0857431676132,-103.00870479455,178.821287383467));
#29763=CARTESIAN_POINT('Ctrl Pts',(-53.9077957782368,-103.040000627442,
177.646659506339));
#29764=CARTESIAN_POINT('Ctrl Pts',(-53.8978577844367,-102.946778855418,
175.985484901271));
#29765=CARTESIAN_POINT('Ctrl Pts',(-53.8879197906366,-102.853557083394,
174.324310296203));
#29766=CARTESIAN_POINT('Ctrl Pts',(-55.0459911519251,-102.635817710771,
173.149682517375));
#29767=CARTESIAN_POINT('Ctrl Pts',(-56.2040625132136,-102.418078338148,
171.975054738546));
#29768=CARTESIAN_POINT('Ctrl Pts',(-57.8459391498707,-102.148762090919,
171.975054808055));
#29769=CARTESIAN_POINT('Ctrl Pts',(-59.4878157865278,-101.879445843689,
171.975054877564));
#29770=CARTESIAN_POINT('Ctrl Pts',(-60.6458870500702,-101.661706481487,
173.149682754692));
#29771=CARTESIAN_POINT('Ctrl Pts',(-61.8039583136126,-101.443967119284,
174.32431063182));
#29772=CARTESIAN_POINT('Ctrl Pts',(-61.7940201815787,-101.350745361997,
175.985485236888));
#29773=CARTESIAN_POINT('Ctrl Pts',(-61.7840820495448,-101.25752360471,177.646659841956));
#29774=CARTESIAN_POINT('Ctrl Pts',(-60.6061345624222,-101.288819448022,
178.821287620784));
#29775=CARTESIAN_POINT('Ctrl Pts',(-59.4281870752997,-101.320115291335,
179.995915399612));
#29776=CARTESIAN_POINT('Ctrl Pts',(-57.7664343128086,-101.402988009253,
179.995915330104));
#29777=CARTESIAN_POINT('Ctrl Pts',(-56.1046815503175,-101.485860727172,
179.995915260595));
#29778=CARTESIAN_POINT('Ctrl Pts',(-54.926734160941,-101.517156560064,178.821287383467));
#29779=CARTESIAN_POINT('Ctrl Pts',(-53.7487867715645,-101.548452392956,
177.646659506339));
#29780=CARTESIAN_POINT('Ctrl Pts',(-53.7388487777644,-101.455230620932,
175.985484901271));
#29781=CARTESIAN_POINT('Ctrl Pts',(-53.7289107839643,-101.362008848909,
174.324310296203));
#29782=CARTESIAN_POINT('Ctrl Pts',(-54.8869821452528,-101.144269476286,
173.149682517375));
#29783=CARTESIAN_POINT('Ctrl Pts',(-56.0450535065414,-100.926530103662,
171.975054738546));
#29784=CARTESIAN_POINT('Ctrl Pts',(-57.6869301431984,-100.657213856433,
171.975054808055));
#29785=CARTESIAN_POINT('Ctrl Pts',(-59.3288067798556,-100.387897609204,
171.975054877564));
#29786=CARTESIAN_POINT('Ctrl Pts',(-60.486878043398,-100.170158247001,173.149682754692));
#29787=CARTESIAN_POINT('Ctrl Pts',(-61.6449493069404,-99.9524188847983,
174.32431063182));
#29788=CARTESIAN_POINT('Ctrl Pts',(-61.6350111749065,-99.8591971275113,
175.985485236888));
#29789=CARTESIAN_POINT('Ctrl Pts',(-61.6250730428726,-99.7659753702243,
177.646659841956));
#29790=CARTESIAN_POINT('Ctrl Pts',(-60.44712555575,-99.7972712135367,178.821287620784));
#29791=CARTESIAN_POINT('Ctrl Pts',(-59.2691780686275,-99.8285670568492,
179.995915399612));
#29792=CARTESIAN_POINT('Ctrl Pts',(-57.6074253061363,-99.9114397747677,
179.995915330104));
#29793=CARTESIAN_POINT('Ctrl Pts',(-55.9456725436452,-99.9943124926864,
179.995915260595));
#29794=CARTESIAN_POINT('Ctrl Pts',(-54.7677251542687,-100.025608325578,
178.821287383467));
#29795=CARTESIAN_POINT('Ctrl Pts',(-53.5897777648923,-100.05690415847,177.646659506339));
#29796=CARTESIAN_POINT('Ctrl Pts',(-53.5798397710922,-99.9636823864468,
175.985484901271));
#29797=CARTESIAN_POINT('Ctrl Pts',(-53.5699017772921,-99.8704606144232,
174.324310296203));
#29798=CARTESIAN_POINT('Ctrl Pts',(-54.7279731385806,-99.6527212418,173.149682517375));
#29799=CARTESIAN_POINT('Ctrl Pts',(-55.8860444998691,-99.4349818691769,
171.975054738546));
#29800=CARTESIAN_POINT('Ctrl Pts',(-57.5279211365262,-99.1656656219475,
171.975054808055));
#29801=CARTESIAN_POINT('Ctrl Pts',(-59.1697977731833,-98.8963493747183,
171.975054877564));
#29802=CARTESIAN_POINT('Ctrl Pts',(-60.3278690367257,-98.6786100125155,
173.149682754692));
#29803=CARTESIAN_POINT('Ctrl Pts',(-61.4859403002682,-98.4608706503128,
174.32431063182));
#29804=CARTESIAN_POINT('Ctrl Pts',(-61.4760021682342,-98.3676488930257,
175.985485236888));
#29805=CARTESIAN_POINT('Ctrl Pts',(-61.4660640362003,-98.2744271357387,
177.646659841956));
#29806=CARTESIAN_POINT('Ctrl Pts',(-60.2881165490778,-98.3057229790511,
178.821287620784));
#29807=CARTESIAN_POINT('Ctrl Pts',(-59.1101690619552,-98.3370188223636,
179.995915399612));
#29808=CARTESIAN_POINT('Ctrl Pts',(-57.4484162994641,-98.4198915402821,
179.995915330104));
#29809=CARTESIAN_POINT('Ctrl Pts',(-55.786663536973,-98.5027642582008,179.995915260595));
#29810=CARTESIAN_POINT('Ctrl Pts',(-54.6087161475965,-98.5340600910929,
178.821287383467));
#29811=CARTESIAN_POINT('Ctrl Pts',(-56.2237961054143,-113.614380048479,
178.813912075476));
#29812=CARTESIAN_POINT('Ctrl Pts',(-55.0488864554725,-113.645352038053,
177.6423391512));
#29813=CARTESIAN_POINT('Ctrl Pts',(-55.0389484614927,-113.552130266048,
175.985484901707));
#29814=CARTESIAN_POINT('Ctrl Pts',(-55.0290104675128,-113.458908494044,
174.328630652215));
#29815=CARTESIAN_POINT('Ctrl Pts',(-56.1840440891124,-113.241492964766,
173.157057825983));
#29816=CARTESIAN_POINT('Ctrl Pts',(-57.3390777107121,-113.024077435489,
171.985484999752));
#29817=CARTESIAN_POINT('Ctrl Pts',(-58.9766583348819,-112.755219171892,
171.985485069079));
#29818=CARTESIAN_POINT('Ctrl Pts',(-60.6142389590518,-112.486360908295,
171.985485138407));
#29819=CARTESIAN_POINT('Ctrl Pts',(-61.7692724831595,-112.268945389411,
173.157058062683));
#29820=CARTESIAN_POINT('Ctrl Pts',(-62.9243060072673,-112.051529870527,
174.328630986959));
#29821=CARTESIAN_POINT('Ctrl Pts',(-62.9143678754131,-111.95830811322,175.985485236451));
#29822=CARTESIAN_POINT('Ctrl Pts',(-62.9044297435589,-111.865086355914,
177.642339485944));
#29823=CARTESIAN_POINT('Ctrl Pts',(-61.7295199961253,-111.896058355881,
178.813912312176));
#29824=CARTESIAN_POINT('Ctrl Pts',(-60.5546102486917,-111.927030355848,
179.985485138407));
#29825=CARTESIAN_POINT('Ctrl Pts',(-58.8971534986878,-112.009445090134,
179.985485069079));
#29826=CARTESIAN_POINT('Ctrl Pts',(-57.2396967486839,-112.09185982442,179.985484999752));
#29827=CARTESIAN_POINT('Ctrl Pts',(-56.0647870987421,-112.122831813994,
178.813912075476));
#29828=CARTESIAN_POINT('Ctrl Pts',(-54.8898774488003,-112.153803803567,
177.6423391512));
#29829=CARTESIAN_POINT('Ctrl Pts',(-54.8799394548205,-112.060582031563,
175.985484901707));
#29830=CARTESIAN_POINT('Ctrl Pts',(-54.8700014608406,-111.967360259558,
174.328630652215));
#29831=CARTESIAN_POINT('Ctrl Pts',(-56.0250350824402,-111.749944730281,
173.157057825983));
#29832=CARTESIAN_POINT('Ctrl Pts',(-57.1800687040398,-111.532529201003,
171.985484999752));
#29833=CARTESIAN_POINT('Ctrl Pts',(-58.8176493282097,-111.263670937406,
171.985485069079));
#29834=CARTESIAN_POINT('Ctrl Pts',(-60.4552299523796,-110.994812673809,
171.985485138407));
#29835=CARTESIAN_POINT('Ctrl Pts',(-61.6102634764873,-110.777397154925,
173.157058062683));
#29836=CARTESIAN_POINT('Ctrl Pts',(-62.7652970005951,-110.559981636041,
174.328630986959));
#29837=CARTESIAN_POINT('Ctrl Pts',(-62.7553588687409,-110.466759878735,
175.985485236451));
#29838=CARTESIAN_POINT('Ctrl Pts',(-62.7454207368867,-110.373538121429,
177.642339485944));
#29839=CARTESIAN_POINT('Ctrl Pts',(-61.5705109894531,-110.404510121395,
178.813912312176));
#29840=CARTESIAN_POINT('Ctrl Pts',(-60.3956012420194,-110.435482121362,
179.985485138407));
#29841=CARTESIAN_POINT('Ctrl Pts',(-58.7381444920155,-110.517896855648,
179.985485069079));
#29842=CARTESIAN_POINT('Ctrl Pts',(-57.0806877420116,-110.600311589935,
179.985484999752));
#29843=CARTESIAN_POINT('Ctrl Pts',(-55.9057780920699,-110.631283579508,
178.813912075476));
#29844=CARTESIAN_POINT('Ctrl Pts',(-54.7308684421281,-110.662255569082,
177.6423391512));
#29845=CARTESIAN_POINT('Ctrl Pts',(-54.7209304481482,-110.569033797077,
175.985484901707));
#29846=CARTESIAN_POINT('Ctrl Pts',(-54.7109924541684,-110.475812025073,
174.328630652215));
#29847=CARTESIAN_POINT('Ctrl Pts',(-55.866026075768,-110.258396495795,173.157057825983));
#29848=CARTESIAN_POINT('Ctrl Pts',(-57.0210596973676,-110.040980966518,
171.985484999752));
#29849=CARTESIAN_POINT('Ctrl Pts',(-58.6586403215375,-109.772122702921,
171.985485069079));
#29850=CARTESIAN_POINT('Ctrl Pts',(-60.2962209457073,-109.503264439324,
171.985485138407));
#29851=CARTESIAN_POINT('Ctrl Pts',(-61.4512544698151,-109.28584892044,173.157058062683));
#29852=CARTESIAN_POINT('Ctrl Pts',(-62.6062879939228,-109.068433401555,
174.328630986959));
#29853=CARTESIAN_POINT('Ctrl Pts',(-62.5963498620687,-108.975211644249,
175.985485236451));
#29854=CARTESIAN_POINT('Ctrl Pts',(-62.5864117302145,-108.881989886943,
177.642339485944));
#29855=CARTESIAN_POINT('Ctrl Pts',(-61.4115019827808,-108.91296188691,178.813912312176));
#29856=CARTESIAN_POINT('Ctrl Pts',(-60.2365922353472,-108.943933886877,
179.985485138407));
#29857=CARTESIAN_POINT('Ctrl Pts',(-58.5791354853433,-109.026348621163,
179.985485069079));
#29858=CARTESIAN_POINT('Ctrl Pts',(-56.9216787353394,-109.108763355449,
179.985484999752));
#29859=CARTESIAN_POINT('Ctrl Pts',(-55.7467690853976,-109.139735345023,
178.813912075476));
#29860=CARTESIAN_POINT('Ctrl Pts',(-54.5718594354559,-109.170707334596,
177.6423391512));
#29861=CARTESIAN_POINT('Ctrl Pts',(-54.561921441476,-109.077485562592,175.985484901707));
#29862=CARTESIAN_POINT('Ctrl Pts',(-54.5519834474962,-108.984263790587,
174.328630652215));
#29863=CARTESIAN_POINT('Ctrl Pts',(-55.7070170690958,-108.76684826131,173.157057825983));
#29864=CARTESIAN_POINT('Ctrl Pts',(-56.8620506906954,-108.549432732032,
171.985484999752));
#29865=CARTESIAN_POINT('Ctrl Pts',(-58.4996313148652,-108.280574468435,
171.985485069079));
#29866=CARTESIAN_POINT('Ctrl Pts',(-60.1372119390351,-108.011716204838,
171.985485138407));
#29867=CARTESIAN_POINT('Ctrl Pts',(-61.2922454631428,-107.794300685954,
173.157058062683));
#29868=CARTESIAN_POINT('Ctrl Pts',(-62.4472789872506,-107.57688516707,174.328630986959));
#29869=CARTESIAN_POINT('Ctrl Pts',(-62.4373408553964,-107.483663409764,
175.985485236451));
#29870=CARTESIAN_POINT('Ctrl Pts',(-62.4274027235423,-107.390441652457,
177.642339485944));
#29871=CARTESIAN_POINT('Ctrl Pts',(-61.2524929761086,-107.421413652424,
178.813912312176));
#29872=CARTESIAN_POINT('Ctrl Pts',(-60.077583228675,-107.452385652391,179.985485138407));
#29873=CARTESIAN_POINT('Ctrl Pts',(-58.4201264786711,-107.534800386677,
179.985485069079));
#29874=CARTESIAN_POINT('Ctrl Pts',(-56.7626697286672,-107.617215120964,
179.985484999752));
#29875=CARTESIAN_POINT('Ctrl Pts',(-55.5877600787254,-107.648187110537,
178.813912075476));
#29876=CARTESIAN_POINT('Ctrl Pts',(-54.4128504287836,-107.67915910011,177.6423391512));
#29877=CARTESIAN_POINT('Ctrl Pts',(-54.4029124348038,-107.585937328106,
175.985484901707));
#29878=CARTESIAN_POINT('Ctrl Pts',(-54.3929744408239,-107.492715556102,
174.328630652215));
#29879=CARTESIAN_POINT('Ctrl Pts',(-55.5480080624235,-107.275300026824,
173.157057825983));
#29880=CARTESIAN_POINT('Ctrl Pts',(-56.7030416840231,-107.057884497547,
171.985484999752));
#29881=CARTESIAN_POINT('Ctrl Pts',(-58.340622308193,-106.78902623395,171.985485069079));
#29882=CARTESIAN_POINT('Ctrl Pts',(-59.9782029323629,-106.520167970353,
171.985485138407));
#29883=CARTESIAN_POINT('Ctrl Pts',(-61.1332364564706,-106.302752451468,
173.157058062683));
#29884=CARTESIAN_POINT('Ctrl Pts',(-62.2882699805784,-106.085336932584,
174.328630986959));
#29885=CARTESIAN_POINT('Ctrl Pts',(-62.2783318487242,-105.992115175278,
175.985485236451));
#29886=CARTESIAN_POINT('Ctrl Pts',(-62.26839371687,-105.898893417972,177.642339485944));
#29887=CARTESIAN_POINT('Ctrl Pts',(-61.0934839694364,-105.929865417939,
178.813912312176));
#29888=CARTESIAN_POINT('Ctrl Pts',(-59.9185742220028,-105.960837417905,
179.985485138407));
#29889=CARTESIAN_POINT('Ctrl Pts',(-58.2611174719989,-106.043252152192,
179.985485069079));
#29890=CARTESIAN_POINT('Ctrl Pts',(-56.603660721995,-106.125666886478,179.985484999752));
#29891=CARTESIAN_POINT('Ctrl Pts',(-55.4287510720532,-106.156638876051,
178.813912075476));
#29892=CARTESIAN_POINT('Ctrl Pts',(-54.2538414221114,-106.187610865625,
177.6423391512));
#29893=CARTESIAN_POINT('Ctrl Pts',(-54.2439034281315,-106.09438909362,175.985484901707));
#29894=CARTESIAN_POINT('Ctrl Pts',(-54.2339654341517,-106.001167321616,
174.328630652215));
#29895=CARTESIAN_POINT('Ctrl Pts',(-55.3889990557513,-105.783751792338,
173.157057825983));
#29896=CARTESIAN_POINT('Ctrl Pts',(-56.5440326773509,-105.566336263061,
171.985484999752));
#29897=CARTESIAN_POINT('Ctrl Pts',(-58.1816133015208,-105.297477999464,
171.985485069079));
#29898=CARTESIAN_POINT('Ctrl Pts',(-59.8191939256906,-105.028619735867,
171.985485138407));
#29899=CARTESIAN_POINT('Ctrl Pts',(-60.9742274497984,-104.811204216983,
173.157058062683));
#29900=CARTESIAN_POINT('Ctrl Pts',(-62.1292609739061,-104.593788698099,
174.328630986959));
#29901=CARTESIAN_POINT('Ctrl Pts',(-62.119322842052,-104.500566940792,175.985485236451));
#29902=CARTESIAN_POINT('Ctrl Pts',(-62.1093847101978,-104.407345183486,
177.642339485944));
#29903=CARTESIAN_POINT('Ctrl Pts',(-60.9344749627642,-104.438317183453,
178.813912312176));
#29904=CARTESIAN_POINT('Ctrl Pts',(-59.7595652153305,-104.46928918342,179.985485138407));
#29905=CARTESIAN_POINT('Ctrl Pts',(-58.1021084653266,-104.551703917706,
179.985485069079));
#29906=CARTESIAN_POINT('Ctrl Pts',(-56.4446517153227,-104.634118651992,
179.985484999752));
#29907=CARTESIAN_POINT('Ctrl Pts',(-55.269742065381,-104.665090641566,178.813912075476));
#29908=CARTESIAN_POINT('Ctrl Pts',(-54.0948324154392,-104.696062631139,
177.6423391512));
#29909=CARTESIAN_POINT('Ctrl Pts',(-54.0848944214593,-104.602840859135,
175.985484901707));
#29910=CARTESIAN_POINT('Ctrl Pts',(-54.0749564274795,-104.50961908713,174.328630652215));
#29911=CARTESIAN_POINT('Ctrl Pts',(-55.2299900490791,-104.292203557853,
173.157057825983));
#29912=CARTESIAN_POINT('Ctrl Pts',(-56.3850236706787,-104.074788028575,
171.985484999752));
#29913=CARTESIAN_POINT('Ctrl Pts',(-58.0226042948486,-103.805929764978,
171.985485069079));
#29914=CARTESIAN_POINT('Ctrl Pts',(-59.6601849190184,-103.537071501381,
171.985485138407));
#29915=CARTESIAN_POINT('Ctrl Pts',(-60.8152184431262,-103.319655982497,
173.157058062683));
#29916=CARTESIAN_POINT('Ctrl Pts',(-61.9702519672339,-103.102240463613,
174.328630986959));
#29917=CARTESIAN_POINT('Ctrl Pts',(-61.9603138353797,-103.009018706307,
175.985485236451));
#29918=CARTESIAN_POINT('Ctrl Pts',(-61.9503757035256,-102.915796949001,
177.642339485944));
#29919=CARTESIAN_POINT('Ctrl Pts',(-60.7754659560919,-102.946768948967,
178.813912312176));
#29920=CARTESIAN_POINT('Ctrl Pts',(-59.6005562086583,-102.977740948934,
179.985485138407));
#29921=CARTESIAN_POINT('Ctrl Pts',(-57.9430994586544,-103.06015568322,179.985485069079));
#29922=CARTESIAN_POINT('Ctrl Pts',(-56.2856427086505,-103.142570417507,
179.985484999752));
#29923=CARTESIAN_POINT('Ctrl Pts',(-55.1107330587087,-103.17354240708,178.813912075476));
#29924=CARTESIAN_POINT('Ctrl Pts',(-53.935823408767,-103.204514396654,177.6423391512));
#29925=CARTESIAN_POINT('Ctrl Pts',(-53.9258854147871,-103.111292624649,
175.985484901707));
#29926=CARTESIAN_POINT('Ctrl Pts',(-53.9159474208072,-103.018070852645,
174.328630652215));
#29927=CARTESIAN_POINT('Ctrl Pts',(-55.0709810424069,-102.800655323367,
173.157057825983));
#29928=CARTESIAN_POINT('Ctrl Pts',(-56.2260146640065,-102.58323979409,171.985484999752));
#29929=CARTESIAN_POINT('Ctrl Pts',(-57.8635952881763,-102.314381530493,
171.985485069079));
#29930=CARTESIAN_POINT('Ctrl Pts',(-59.5011759123462,-102.045523266896,
171.985485138407));
#29931=CARTESIAN_POINT('Ctrl Pts',(-60.6562094364539,-101.828107748012,
173.157058062683));
#29932=CARTESIAN_POINT('Ctrl Pts',(-61.8112429605617,-101.610692229127,
174.328630986959));
#29933=CARTESIAN_POINT('Ctrl Pts',(-61.8013048287075,-101.517470471821,
175.985485236451));
#29934=CARTESIAN_POINT('Ctrl Pts',(-61.7913666968533,-101.424248714515,
177.642339485944));
#29935=CARTESIAN_POINT('Ctrl Pts',(-60.6164569494197,-101.455220714482,
178.813912312176));
#29936=CARTESIAN_POINT('Ctrl Pts',(-59.4415472019861,-101.486192714449,
179.985485138407));
#29937=CARTESIAN_POINT('Ctrl Pts',(-57.7840904519822,-101.568607448735,
179.985485069079));
#29938=CARTESIAN_POINT('Ctrl Pts',(-56.1266337019783,-101.651022183021,
179.985484999752));
#29939=CARTESIAN_POINT('Ctrl Pts',(-54.9517240520365,-101.681994172595,
178.813912075476));
#29940=CARTESIAN_POINT('Ctrl Pts',(-53.7768144020947,-101.712966162168,
177.6423391512));
#29941=CARTESIAN_POINT('Ctrl Pts',(-53.7668764081149,-101.619744390164,
175.985484901707));
#29942=CARTESIAN_POINT('Ctrl Pts',(-53.756938414135,-101.526522618159,174.328630652215));
#29943=CARTESIAN_POINT('Ctrl Pts',(-54.9119720357346,-101.309107088882,
173.157057825983));
#29944=CARTESIAN_POINT('Ctrl Pts',(-56.0670056573342,-101.091691559604,
171.985484999752));
#29945=CARTESIAN_POINT('Ctrl Pts',(-57.7045862815041,-100.822833296007,
171.985485069079));
#29946=CARTESIAN_POINT('Ctrl Pts',(-59.342166905674,-100.55397503241,171.985485138407));
#29947=CARTESIAN_POINT('Ctrl Pts',(-60.4972004297817,-100.336559513526,
173.157058062683));
#29948=CARTESIAN_POINT('Ctrl Pts',(-61.6522339538895,-100.119143994642,
174.328630986959));
#29949=CARTESIAN_POINT('Ctrl Pts',(-61.6422958220353,-100.025922237336,
175.985485236451));
#29950=CARTESIAN_POINT('Ctrl Pts',(-61.6323576901811,-99.9327004800294,
177.642339485944));
#29951=CARTESIAN_POINT('Ctrl Pts',(-60.4574479427475,-99.9636724799962,
178.813912312176));
#29952=CARTESIAN_POINT('Ctrl Pts',(-59.2825381953138,-99.994644479963,179.985485138407));
#29953=CARTESIAN_POINT('Ctrl Pts',(-57.6250814453099,-100.077059214249,
179.985485069079));
#29954=CARTESIAN_POINT('Ctrl Pts',(-55.9676246953061,-100.159473948536,
179.985484999752));
#29955=CARTESIAN_POINT('Ctrl Pts',(-54.7927150453643,-100.190445938109,
178.813912075476));
#29956=CARTESIAN_POINT('Ctrl Pts',(-53.6178053954225,-100.221417927683,
177.6423391512));
#29957=CARTESIAN_POINT('Ctrl Pts',(-53.6078674014426,-100.128196155678,
175.985484901707));
#29958=CARTESIAN_POINT('Ctrl Pts',(-53.5979294074628,-100.034974383673,
174.328630652215));
#29959=CARTESIAN_POINT('Ctrl Pts',(-54.7529630290624,-99.817558854396,173.157057825983));
#29960=CARTESIAN_POINT('Ctrl Pts',(-55.907996650662,-99.6001433251185,171.985484999752));
#29961=CARTESIAN_POINT('Ctrl Pts',(-57.5455772748319,-99.3312850615215,
171.985485069079));
#29962=CARTESIAN_POINT('Ctrl Pts',(-59.1831578990017,-99.0624267979246,
171.985485138407));
#29963=CARTESIAN_POINT('Ctrl Pts',(-60.3381914231095,-98.8450112790404,
173.157058062683));
#29964=CARTESIAN_POINT('Ctrl Pts',(-61.4932249472172,-98.6275957601562,
174.328630986959));
#29965=CARTESIAN_POINT('Ctrl Pts',(-61.4832868153631,-98.53437400285,175.985485236451));
#29966=CARTESIAN_POINT('Ctrl Pts',(-61.4733486835089,-98.4411522455438,
177.642339485944));
#29967=CARTESIAN_POINT('Ctrl Pts',(-60.2984389360752,-98.4721242455106,
178.813912312176));
#29968=CARTESIAN_POINT('Ctrl Pts',(-59.1235291886416,-98.5030962454774,
179.985485138407));
#29969=CARTESIAN_POINT('Ctrl Pts',(-57.4660724386377,-98.5855109797636,
179.985485069079));
#29970=CARTESIAN_POINT('Ctrl Pts',(-55.8086156886338,-98.6679257140499,
179.985484999752));
#29971=CARTESIAN_POINT('Ctrl Pts',(-54.633706038692,-98.6988977036234,178.813912075476));
#29972=CARTESIAN_POINT('Ctrl Pts',(-56.2237961054143,-113.614380048479,
178.813912075476));
#29973=CARTESIAN_POINT('Ctrl Pts',(-55.0488864554725,-113.645352038053,
177.6423391512));
#29974=CARTESIAN_POINT('Ctrl Pts',(-55.0389484614927,-113.552130266048,
175.985484901707));
#29975=CARTESIAN_POINT('Ctrl Pts',(-55.0290104675128,-113.458908494044,
174.328630652215));
#29976=CARTESIAN_POINT('Ctrl Pts',(-56.1840440891124,-113.241492964766,
173.157057825983));
#29977=CARTESIAN_POINT('Ctrl Pts',(-57.3390777107121,-113.024077435489,
171.985484999752));
#29978=CARTESIAN_POINT('Ctrl Pts',(-58.9766583348819,-112.755219171892,
171.985485069079));
#29979=CARTESIAN_POINT('Ctrl Pts',(-60.6142389590518,-112.486360908295,
171.985485138407));
#29980=CARTESIAN_POINT('Ctrl Pts',(-61.7692724831595,-112.268945389411,
173.157058062683));
#29981=CARTESIAN_POINT('Ctrl Pts',(-62.9243060072673,-112.051529870527,
174.328630986959));
#29982=CARTESIAN_POINT('Ctrl Pts',(-62.9143678754131,-111.95830811322,175.985485236451));
#29983=CARTESIAN_POINT('Ctrl Pts',(-62.9044297435589,-111.865086355914,
177.642339485944));
#29984=CARTESIAN_POINT('Ctrl Pts',(-61.7295199961253,-111.896058355881,
178.813912312176));
#29985=CARTESIAN_POINT('Ctrl Pts',(-60.5546102486917,-111.927030355848,
179.985485138407));
#29986=CARTESIAN_POINT('Ctrl Pts',(-58.8971534986878,-112.009445090134,
179.985485069079));
#29987=CARTESIAN_POINT('Ctrl Pts',(-57.2396967486839,-112.09185982442,179.985484999752));
#29988=CARTESIAN_POINT('Ctrl Pts',(-56.0647870987421,-112.122831813994,
178.813912075476));
#29989=CARTESIAN_POINT('Ctrl Pts',(-54.8898774488003,-112.153803803567,
177.6423391512));
#29990=CARTESIAN_POINT('Ctrl Pts',(-54.8799394548205,-112.060582031563,
175.985484901707));
#29991=CARTESIAN_POINT('Ctrl Pts',(-54.8700014608406,-111.967360259558,
174.328630652215));
#29992=CARTESIAN_POINT('Ctrl Pts',(-56.0250350824402,-111.749944730281,
173.157057825983));
#29993=CARTESIAN_POINT('Ctrl Pts',(-57.1800687040398,-111.532529201003,
171.985484999752));
#29994=CARTESIAN_POINT('Ctrl Pts',(-58.8176493282097,-111.263670937406,
171.985485069079));
#29995=CARTESIAN_POINT('Ctrl Pts',(-60.4552299523796,-110.994812673809,
171.985485138407));
#29996=CARTESIAN_POINT('Ctrl Pts',(-61.6102634764873,-110.777397154925,
173.157058062683));
#29997=CARTESIAN_POINT('Ctrl Pts',(-62.7652970005951,-110.559981636041,
174.328630986959));
#29998=CARTESIAN_POINT('Ctrl Pts',(-62.7553588687409,-110.466759878735,
175.985485236451));
#29999=CARTESIAN_POINT('Ctrl Pts',(-62.7454207368867,-110.373538121429,
177.642339485944));
#30000=CARTESIAN_POINT('Ctrl Pts',(-61.5705109894531,-110.404510121395,
178.813912312176));
#30001=CARTESIAN_POINT('Ctrl Pts',(-60.3956012420194,-110.435482121362,
179.985485138407));
#30002=CARTESIAN_POINT('Ctrl Pts',(-58.7381444920155,-110.517896855648,
179.985485069079));
#30003=CARTESIAN_POINT('Ctrl Pts',(-57.0806877420116,-110.600311589935,
179.985484999752));
#30004=CARTESIAN_POINT('Ctrl Pts',(-55.9057780920699,-110.631283579508,
178.813912075476));
#30005=CARTESIAN_POINT('Ctrl Pts',(-54.7308684421281,-110.662255569082,
177.6423391512));
#30006=CARTESIAN_POINT('Ctrl Pts',(-54.7209304481482,-110.569033797077,
175.985484901707));
#30007=CARTESIAN_POINT('Ctrl Pts',(-54.7109924541684,-110.475812025073,
174.328630652215));
#30008=CARTESIAN_POINT('Ctrl Pts',(-55.866026075768,-110.258396495795,173.157057825983));
#30009=CARTESIAN_POINT('Ctrl Pts',(-57.0210596973676,-110.040980966518,
171.985484999752));
#30010=CARTESIAN_POINT('Ctrl Pts',(-58.6586403215375,-109.772122702921,
171.985485069079));
#30011=CARTESIAN_POINT('Ctrl Pts',(-60.2962209457073,-109.503264439324,
171.985485138407));
#30012=CARTESIAN_POINT('Ctrl Pts',(-61.4512544698151,-109.28584892044,173.157058062683));
#30013=CARTESIAN_POINT('Ctrl Pts',(-62.6062879939228,-109.068433401555,
174.328630986959));
#30014=CARTESIAN_POINT('Ctrl Pts',(-62.5963498620687,-108.975211644249,
175.985485236451));
#30015=CARTESIAN_POINT('Ctrl Pts',(-62.5864117302145,-108.881989886943,
177.642339485944));
#30016=CARTESIAN_POINT('Ctrl Pts',(-61.4115019827808,-108.91296188691,178.813912312176));
#30017=CARTESIAN_POINT('Ctrl Pts',(-60.2365922353472,-108.943933886877,
179.985485138407));
#30018=CARTESIAN_POINT('Ctrl Pts',(-58.5791354853433,-109.026348621163,
179.985485069079));
#30019=CARTESIAN_POINT('Ctrl Pts',(-56.9216787353394,-109.108763355449,
179.985484999752));
#30020=CARTESIAN_POINT('Ctrl Pts',(-55.7467690853976,-109.139735345023,
178.813912075476));
#30021=CARTESIAN_POINT('Ctrl Pts',(-54.5718594354559,-109.170707334596,
177.6423391512));
#30022=CARTESIAN_POINT('Ctrl Pts',(-54.561921441476,-109.077485562592,175.985484901707));
#30023=CARTESIAN_POINT('Ctrl Pts',(-54.5519834474962,-108.984263790587,
174.328630652215));
#30024=CARTESIAN_POINT('Ctrl Pts',(-55.7070170690958,-108.76684826131,173.157057825983));
#30025=CARTESIAN_POINT('Ctrl Pts',(-56.8620506906954,-108.549432732032,
171.985484999752));
#30026=CARTESIAN_POINT('Ctrl Pts',(-58.4996313148652,-108.280574468435,
171.985485069079));
#30027=CARTESIAN_POINT('Ctrl Pts',(-60.1372119390351,-108.011716204838,
171.985485138407));
#30028=CARTESIAN_POINT('Ctrl Pts',(-61.2922454631428,-107.794300685954,
173.157058062683));
#30029=CARTESIAN_POINT('Ctrl Pts',(-62.4472789872506,-107.57688516707,174.328630986959));
#30030=CARTESIAN_POINT('Ctrl Pts',(-62.4373408553964,-107.483663409764,
175.985485236451));
#30031=CARTESIAN_POINT('Ctrl Pts',(-62.4274027235423,-107.390441652457,
177.642339485944));
#30032=CARTESIAN_POINT('Ctrl Pts',(-61.2524929761086,-107.421413652424,
178.813912312176));
#30033=CARTESIAN_POINT('Ctrl Pts',(-60.077583228675,-107.452385652391,179.985485138407));
#30034=CARTESIAN_POINT('Ctrl Pts',(-58.4201264786711,-107.534800386677,
179.985485069079));
#30035=CARTESIAN_POINT('Ctrl Pts',(-56.7626697286672,-107.617215120964,
179.985484999752));
#30036=CARTESIAN_POINT('Ctrl Pts',(-55.5877600787254,-107.648187110537,
178.813912075476));
#30037=CARTESIAN_POINT('Ctrl Pts',(-54.4128504287836,-107.67915910011,177.6423391512));
#30038=CARTESIAN_POINT('Ctrl Pts',(-54.4029124348038,-107.585937328106,
175.985484901707));
#30039=CARTESIAN_POINT('Ctrl Pts',(-54.3929744408239,-107.492715556102,
174.328630652215));
#30040=CARTESIAN_POINT('Ctrl Pts',(-55.5480080624235,-107.275300026824,
173.157057825983));
#30041=CARTESIAN_POINT('Ctrl Pts',(-56.7030416840231,-107.057884497547,
171.985484999752));
#30042=CARTESIAN_POINT('Ctrl Pts',(-58.340622308193,-106.78902623395,171.985485069079));
#30043=CARTESIAN_POINT('Ctrl Pts',(-59.9782029323629,-106.520167970353,
171.985485138407));
#30044=CARTESIAN_POINT('Ctrl Pts',(-61.1332364564706,-106.302752451468,
173.157058062683));
#30045=CARTESIAN_POINT('Ctrl Pts',(-62.2882699805784,-106.085336932584,
174.328630986959));
#30046=CARTESIAN_POINT('Ctrl Pts',(-62.2783318487242,-105.992115175278,
175.985485236451));
#30047=CARTESIAN_POINT('Ctrl Pts',(-62.26839371687,-105.898893417972,177.642339485944));
#30048=CARTESIAN_POINT('Ctrl Pts',(-61.0934839694364,-105.929865417939,
178.813912312176));
#30049=CARTESIAN_POINT('Ctrl Pts',(-59.9185742220028,-105.960837417905,
179.985485138407));
#30050=CARTESIAN_POINT('Ctrl Pts',(-58.2611174719989,-106.043252152192,
179.985485069079));
#30051=CARTESIAN_POINT('Ctrl Pts',(-56.603660721995,-106.125666886478,179.985484999752));
#30052=CARTESIAN_POINT('Ctrl Pts',(-55.4287510720532,-106.156638876051,
178.813912075476));
#30053=CARTESIAN_POINT('Ctrl Pts',(-54.2538414221114,-106.187610865625,
177.6423391512));
#30054=CARTESIAN_POINT('Ctrl Pts',(-54.2439034281315,-106.09438909362,175.985484901707));
#30055=CARTESIAN_POINT('Ctrl Pts',(-54.2339654341517,-106.001167321616,
174.328630652215));
#30056=CARTESIAN_POINT('Ctrl Pts',(-55.3889990557513,-105.783751792338,
173.157057825983));
#30057=CARTESIAN_POINT('Ctrl Pts',(-56.5440326773509,-105.566336263061,
171.985484999752));
#30058=CARTESIAN_POINT('Ctrl Pts',(-58.1816133015208,-105.297477999464,
171.985485069079));
#30059=CARTESIAN_POINT('Ctrl Pts',(-59.8191939256906,-105.028619735867,
171.985485138407));
#30060=CARTESIAN_POINT('Ctrl Pts',(-60.9742274497984,-104.811204216983,
173.157058062683));
#30061=CARTESIAN_POINT('Ctrl Pts',(-62.1292609739061,-104.593788698099,
174.328630986959));
#30062=CARTESIAN_POINT('Ctrl Pts',(-62.119322842052,-104.500566940792,175.985485236451));
#30063=CARTESIAN_POINT('Ctrl Pts',(-62.1093847101978,-104.407345183486,
177.642339485944));
#30064=CARTESIAN_POINT('Ctrl Pts',(-60.9344749627642,-104.438317183453,
178.813912312176));
#30065=CARTESIAN_POINT('Ctrl Pts',(-59.7595652153305,-104.46928918342,179.985485138407));
#30066=CARTESIAN_POINT('Ctrl Pts',(-58.1021084653266,-104.551703917706,
179.985485069079));
#30067=CARTESIAN_POINT('Ctrl Pts',(-56.4446517153227,-104.634118651992,
179.985484999752));
#30068=CARTESIAN_POINT('Ctrl Pts',(-55.269742065381,-104.665090641566,178.813912075476));
#30069=CARTESIAN_POINT('Ctrl Pts',(-54.0948324154392,-104.696062631139,
177.6423391512));
#30070=CARTESIAN_POINT('Ctrl Pts',(-54.0848944214593,-104.602840859135,
175.985484901707));
#30071=CARTESIAN_POINT('Ctrl Pts',(-54.0749564274795,-104.50961908713,174.328630652215));
#30072=CARTESIAN_POINT('Ctrl Pts',(-55.2299900490791,-104.292203557853,
173.157057825983));
#30073=CARTESIAN_POINT('Ctrl Pts',(-56.3850236706787,-104.074788028575,
171.985484999752));
#30074=CARTESIAN_POINT('Ctrl Pts',(-58.0226042948486,-103.805929764978,
171.985485069079));
#30075=CARTESIAN_POINT('Ctrl Pts',(-59.6601849190184,-103.537071501381,
171.985485138407));
#30076=CARTESIAN_POINT('Ctrl Pts',(-60.8152184431262,-103.319655982497,
173.157058062683));
#30077=CARTESIAN_POINT('Ctrl Pts',(-61.9702519672339,-103.102240463613,
174.328630986959));
#30078=CARTESIAN_POINT('Ctrl Pts',(-61.9603138353797,-103.009018706307,
175.985485236451));
#30079=CARTESIAN_POINT('Ctrl Pts',(-61.9503757035256,-102.915796949001,
177.642339485944));
#30080=CARTESIAN_POINT('Ctrl Pts',(-60.7754659560919,-102.946768948967,
178.813912312176));
#30081=CARTESIAN_POINT('Ctrl Pts',(-59.6005562086583,-102.977740948934,
179.985485138407));
#30082=CARTESIAN_POINT('Ctrl Pts',(-57.9430994586544,-103.06015568322,179.985485069079));
#30083=CARTESIAN_POINT('Ctrl Pts',(-56.2856427086505,-103.142570417507,
179.985484999752));
#30084=CARTESIAN_POINT('Ctrl Pts',(-55.1107330587087,-103.17354240708,178.813912075476));
#30085=CARTESIAN_POINT('Ctrl Pts',(-53.935823408767,-103.204514396654,177.6423391512));
#30086=CARTESIAN_POINT('Ctrl Pts',(-53.9258854147871,-103.111292624649,
175.985484901707));
#30087=CARTESIAN_POINT('Ctrl Pts',(-53.9159474208072,-103.018070852645,
174.328630652215));
#30088=CARTESIAN_POINT('Ctrl Pts',(-55.0709810424069,-102.800655323367,
173.157057825983));
#30089=CARTESIAN_POINT('Ctrl Pts',(-56.2260146640065,-102.58323979409,171.985484999752));
#30090=CARTESIAN_POINT('Ctrl Pts',(-57.8635952881763,-102.314381530493,
171.985485069079));
#30091=CARTESIAN_POINT('Ctrl Pts',(-59.5011759123462,-102.045523266896,
171.985485138407));
#30092=CARTESIAN_POINT('Ctrl Pts',(-60.6562094364539,-101.828107748012,
173.157058062683));
#30093=CARTESIAN_POINT('Ctrl Pts',(-61.8112429605617,-101.610692229127,
174.328630986959));
#30094=CARTESIAN_POINT('Ctrl Pts',(-61.8013048287075,-101.517470471821,
175.985485236451));
#30095=CARTESIAN_POINT('Ctrl Pts',(-61.7913666968533,-101.424248714515,
177.642339485944));
#30096=CARTESIAN_POINT('Ctrl Pts',(-60.6164569494197,-101.455220714482,
178.813912312176));
#30097=CARTESIAN_POINT('Ctrl Pts',(-59.4415472019861,-101.486192714449,
179.985485138407));
#30098=CARTESIAN_POINT('Ctrl Pts',(-57.7840904519822,-101.568607448735,
179.985485069079));
#30099=CARTESIAN_POINT('Ctrl Pts',(-56.1266337019783,-101.651022183021,
179.985484999752));
#30100=CARTESIAN_POINT('Ctrl Pts',(-54.9517240520365,-101.681994172595,
178.813912075476));
#30101=CARTESIAN_POINT('Ctrl Pts',(-53.7768144020947,-101.712966162168,
177.6423391512));
#30102=CARTESIAN_POINT('Ctrl Pts',(-53.7668764081149,-101.619744390164,
175.985484901707));
#30103=CARTESIAN_POINT('Ctrl Pts',(-53.756938414135,-101.526522618159,174.328630652215));
#30104=CARTESIAN_POINT('Ctrl Pts',(-54.9119720357346,-101.309107088882,
173.157057825983));
#30105=CARTESIAN_POINT('Ctrl Pts',(-56.0670056573342,-101.091691559604,
171.985484999752));
#30106=CARTESIAN_POINT('Ctrl Pts',(-57.7045862815041,-100.822833296007,
171.985485069079));
#30107=CARTESIAN_POINT('Ctrl Pts',(-59.342166905674,-100.55397503241,171.985485138407));
#30108=CARTESIAN_POINT('Ctrl Pts',(-60.4972004297817,-100.336559513526,
173.157058062683));
#30109=CARTESIAN_POINT('Ctrl Pts',(-61.6522339538895,-100.119143994642,
174.328630986959));
#30110=CARTESIAN_POINT('Ctrl Pts',(-61.6422958220353,-100.025922237336,
175.985485236451));
#30111=CARTESIAN_POINT('Ctrl Pts',(-61.6323576901811,-99.9327004800294,
177.642339485944));
#30112=CARTESIAN_POINT('Ctrl Pts',(-60.4574479427475,-99.9636724799962,
178.813912312176));
#30113=CARTESIAN_POINT('Ctrl Pts',(-59.2825381953138,-99.994644479963,179.985485138407));
#30114=CARTESIAN_POINT('Ctrl Pts',(-57.6250814453099,-100.077059214249,
179.985485069079));
#30115=CARTESIAN_POINT('Ctrl Pts',(-55.9676246953061,-100.159473948536,
179.985484999752));
#30116=CARTESIAN_POINT('Ctrl Pts',(-54.7927150453643,-100.190445938109,
178.813912075476));
#30117=CARTESIAN_POINT('Ctrl Pts',(-53.6178053954225,-100.221417927683,
177.6423391512));
#30118=CARTESIAN_POINT('Ctrl Pts',(-53.6078674014426,-100.128196155678,
175.985484901707));
#30119=CARTESIAN_POINT('Ctrl Pts',(-53.5979294074628,-100.034974383673,
174.328630652215));
#30120=CARTESIAN_POINT('Ctrl Pts',(-54.7529630290624,-99.817558854396,173.157057825983));
#30121=CARTESIAN_POINT('Ctrl Pts',(-55.907996650662,-99.6001433251185,171.985484999752));
#30122=CARTESIAN_POINT('Ctrl Pts',(-57.5455772748319,-99.3312850615215,
171.985485069079));
#30123=CARTESIAN_POINT('Ctrl Pts',(-59.1831578990017,-99.0624267979246,
171.985485138407));
#30124=CARTESIAN_POINT('Ctrl Pts',(-60.3381914231095,-98.8450112790404,
173.157058062683));
#30125=CARTESIAN_POINT('Ctrl Pts',(-61.4932249472172,-98.6275957601562,
174.328630986959));
#30126=CARTESIAN_POINT('Ctrl Pts',(-61.4832868153631,-98.53437400285,175.985485236451));
#30127=CARTESIAN_POINT('Ctrl Pts',(-61.4733486835089,-98.4411522455438,
177.642339485944));
#30128=CARTESIAN_POINT('Ctrl Pts',(-60.2984389360752,-98.4721242455106,
178.813912312176));
#30129=CARTESIAN_POINT('Ctrl Pts',(-59.1235291886416,-98.5030962454774,
179.985485138407));
#30130=CARTESIAN_POINT('Ctrl Pts',(-57.4660724386377,-98.5855109797636,
179.985485069079));
#30131=CARTESIAN_POINT('Ctrl Pts',(-55.8086156886338,-98.6679257140499,
179.985484999752));
#30132=CARTESIAN_POINT('Ctrl Pts',(-54.633706038692,-98.6988977036234,178.813912075476));
#30133=CARTESIAN_POINT('Ctrl Pts',(-56.9964983346804,-113.864655531781,
178.072094410988));
#30134=CARTESIAN_POINT('Ctrl Pts',(-56.1271283009022,-113.863054956993,
177.207792449865));
#30135=CARTESIAN_POINT('Ctrl Pts',(-56.117190288842,-113.769833186916,175.985484945604));
#30136=CARTESIAN_POINT('Ctrl Pts',(-56.1072522767819,-113.676611416839,
174.763177441344));
#30137=CARTESIAN_POINT('Ctrl Pts',(-56.9567462566485,-113.491768454648,
173.89887555255));
#30138=CARTESIAN_POINT('Ctrl Pts',(-57.8062402365152,-113.306925492458,
173.034573663757));
#30139=CARTESIAN_POINT('Ctrl Pts',(-59.011722573584,-113.084131793069,173.034573714903));
#30140=CARTESIAN_POINT('Ctrl Pts',(-60.2172049106529,-112.86133809368,173.034573766048));
#30141=CARTESIAN_POINT('Ctrl Pts',(-61.0666988185971,-112.676495139156,
173.898875727171));
#30142=CARTESIAN_POINT('Ctrl Pts',(-61.9161927265413,-112.491652184633,
174.763177688294));
#30143=CARTESIAN_POINT('Ctrl Pts',(-61.9062546127674,-112.398430425399,
175.985485192554));
#30144=CARTESIAN_POINT('Ctrl Pts',(-61.8963164989935,-112.305208666166,
177.207792696815));
#30145=CARTESIAN_POINT('Ctrl Pts',(-61.0269463932928,-112.303608099046,
178.072094585608));
#30146=CARTESIAN_POINT('Ctrl Pts',(-60.1575762875921,-112.302007531926,
178.936396474401));
#30147=CARTESIAN_POINT('Ctrl Pts',(-58.9322178246893,-112.338357702004,
178.936396423256));
#30148=CARTESIAN_POINT('Ctrl Pts',(-57.7068593617864,-112.374707872082,
178.936396372111));
#30149=CARTESIAN_POINT('Ctrl Pts',(-56.8374893280082,-112.373107297295,
178.072094410988));
#30150=CARTESIAN_POINT('Ctrl Pts',(-55.9681192942299,-112.371506722508,
177.207792449865));
#30151=CARTESIAN_POINT('Ctrl Pts',(-55.9581812821698,-112.278284952431,
175.985484945604));
#30152=CARTESIAN_POINT('Ctrl Pts',(-55.9482432701096,-112.185063182354,
174.763177441344));
#30153=CARTESIAN_POINT('Ctrl Pts',(-56.7977372499763,-112.000220220163,
173.89887555255));
#30154=CARTESIAN_POINT('Ctrl Pts',(-57.647231229843,-111.815377257972,173.034573663757));
#30155=CARTESIAN_POINT('Ctrl Pts',(-58.8527135669118,-111.592583558583,
173.034573714903));
#30156=CARTESIAN_POINT('Ctrl Pts',(-60.0581959039807,-111.369789859194,
173.034573766048));
#30157=CARTESIAN_POINT('Ctrl Pts',(-60.9076898119249,-111.184946904671,
173.898875727171));
#30158=CARTESIAN_POINT('Ctrl Pts',(-61.7571837198691,-111.000103950148,
174.763177688294));
#30159=CARTESIAN_POINT('Ctrl Pts',(-61.7472456060952,-110.906882190914,
175.985485192554));
#30160=CARTESIAN_POINT('Ctrl Pts',(-61.7373074923213,-110.81366043168,177.207792696815));
#30161=CARTESIAN_POINT('Ctrl Pts',(-60.8679373866206,-110.81205986456,178.072094585608));
#30162=CARTESIAN_POINT('Ctrl Pts',(-59.9985672809199,-110.81045929744,178.936396474401));
#30163=CARTESIAN_POINT('Ctrl Pts',(-58.7732088180171,-110.846809467519,
178.936396423256));
#30164=CARTESIAN_POINT('Ctrl Pts',(-57.5478503551142,-110.883159637597,
178.936396372111));
#30165=CARTESIAN_POINT('Ctrl Pts',(-56.6784803213359,-110.881559062809,
178.072094410988));
#30166=CARTESIAN_POINT('Ctrl Pts',(-55.8091102875577,-110.879958488022,
177.207792449865));
#30167=CARTESIAN_POINT('Ctrl Pts',(-55.7991722754976,-110.786736717945,
175.985484945604));
#30168=CARTESIAN_POINT('Ctrl Pts',(-55.7892342634374,-110.693514947868,
174.763177441344));
#30169=CARTESIAN_POINT('Ctrl Pts',(-56.6387282433041,-110.508671985677,
173.89887555255));
#30170=CARTESIAN_POINT('Ctrl Pts',(-57.4882222231708,-110.323829023487,
173.034573663757));
#30171=CARTESIAN_POINT('Ctrl Pts',(-58.6937045602396,-110.101035324098,
173.034573714903));
#30172=CARTESIAN_POINT('Ctrl Pts',(-59.8991868973084,-109.878241624709,
173.034573766048));
#30173=CARTESIAN_POINT('Ctrl Pts',(-60.7486808052526,-109.693398670185,
173.898875727171));
#30174=CARTESIAN_POINT('Ctrl Pts',(-61.5981747131968,-109.508555715662,
174.763177688294));
#30175=CARTESIAN_POINT('Ctrl Pts',(-61.588236599423,-109.415333956428,175.985485192554));
#30176=CARTESIAN_POINT('Ctrl Pts',(-61.5782984856491,-109.322112197195,
177.207792696815));
#30177=CARTESIAN_POINT('Ctrl Pts',(-60.7089283799484,-109.320511630075,
178.072094585608));
#30178=CARTESIAN_POINT('Ctrl Pts',(-59.8395582742477,-109.318911062955,
178.936396474401));
#30179=CARTESIAN_POINT('Ctrl Pts',(-58.6141998113448,-109.355261233033,
178.936396423256));
#30180=CARTESIAN_POINT('Ctrl Pts',(-57.388841348442,-109.391611403111,178.936396372111));
#30181=CARTESIAN_POINT('Ctrl Pts',(-56.5194713146637,-109.390010828324,
178.072094410988));
#30182=CARTESIAN_POINT('Ctrl Pts',(-55.6501012808855,-109.388410253536,
177.207792449865));
#30183=CARTESIAN_POINT('Ctrl Pts',(-55.6401632688253,-109.295188483459,
175.985484945604));
#30184=CARTESIAN_POINT('Ctrl Pts',(-55.6302252567652,-109.201966713382,
174.763177441344));
#30185=CARTESIAN_POINT('Ctrl Pts',(-56.4797192366319,-109.017123751192,
173.89887555255));
#30186=CARTESIAN_POINT('Ctrl Pts',(-57.3292132164985,-108.832280789001,
173.034573663757));
#30187=CARTESIAN_POINT('Ctrl Pts',(-58.5346955535674,-108.609487089612,
173.034573714903));
#30188=CARTESIAN_POINT('Ctrl Pts',(-59.7401778906362,-108.386693390223,
173.034573766048));
#30189=CARTESIAN_POINT('Ctrl Pts',(-60.5896717985804,-108.2018504357,173.898875727171));
#30190=CARTESIAN_POINT('Ctrl Pts',(-61.4391657065246,-108.017007481176,
174.763177688294));
#30191=CARTESIAN_POINT('Ctrl Pts',(-61.4292275927507,-107.923785721943,
175.985485192554));
#30192=CARTESIAN_POINT('Ctrl Pts',(-61.4192894789769,-107.830563962709,
177.207792696815));
#30193=CARTESIAN_POINT('Ctrl Pts',(-60.5499193732762,-107.828963395589,
178.072094585608));
#30194=CARTESIAN_POINT('Ctrl Pts',(-59.6805492675755,-107.827362828469,
178.936396474401));
#30195=CARTESIAN_POINT('Ctrl Pts',(-58.4551908046726,-107.863712998547,
178.936396423256));
#30196=CARTESIAN_POINT('Ctrl Pts',(-57.2298323417698,-107.900063168626,
178.936396372111));
#30197=CARTESIAN_POINT('Ctrl Pts',(-56.3604623079915,-107.898462593838,
178.072094410988));
#30198=CARTESIAN_POINT('Ctrl Pts',(-55.4910922742133,-107.896862019051,
177.207792449865));
#30199=CARTESIAN_POINT('Ctrl Pts',(-55.4811542621531,-107.803640248974,
175.985484945604));
#30200=CARTESIAN_POINT('Ctrl Pts',(-55.471216250093,-107.710418478897,174.763177441344));
#30201=CARTESIAN_POINT('Ctrl Pts',(-56.3207102299596,-107.525575516706,
173.89887555255));
#30202=CARTESIAN_POINT('Ctrl Pts',(-57.1702042098263,-107.340732554515,
173.034573663757));
#30203=CARTESIAN_POINT('Ctrl Pts',(-58.3756865468951,-107.117938855126,
173.034573714903));
#30204=CARTESIAN_POINT('Ctrl Pts',(-59.581168883964,-106.895145155737,173.034573766048));
#30205=CARTESIAN_POINT('Ctrl Pts',(-60.4306627919082,-106.710302201214,
173.898875727171));
#30206=CARTESIAN_POINT('Ctrl Pts',(-61.2801566998524,-106.525459246691,
174.763177688294));
#30207=CARTESIAN_POINT('Ctrl Pts',(-61.2702185860785,-106.432237487457,
175.985485192554));
#30208=CARTESIAN_POINT('Ctrl Pts',(-61.2602804723046,-106.339015728223,
177.207792696815));
#30209=CARTESIAN_POINT('Ctrl Pts',(-60.3909103666039,-106.337415161103,
178.072094585608));
#30210=CARTESIAN_POINT('Ctrl Pts',(-59.5215402609032,-106.335814593983,
178.936396474401));
#30211=CARTESIAN_POINT('Ctrl Pts',(-58.2961817980004,-106.372164764062,
178.936396423256));
#30212=CARTESIAN_POINT('Ctrl Pts',(-57.0708233350975,-106.40851493414,178.936396372111));
#30213=CARTESIAN_POINT('Ctrl Pts',(-56.2014533013193,-106.406914359353,
178.072094410988));
#30214=CARTESIAN_POINT('Ctrl Pts',(-55.332083267541,-106.405313784565,177.207792449865));
#30215=CARTESIAN_POINT('Ctrl Pts',(-55.3221452554809,-106.312092014488,
175.985484945604));
#30216=CARTESIAN_POINT('Ctrl Pts',(-55.3122072434207,-106.218870244411,
174.763177441344));
#30217=CARTESIAN_POINT('Ctrl Pts',(-56.1617012232874,-106.034027282221,
173.89887555255));
#30218=CARTESIAN_POINT('Ctrl Pts',(-57.0111952031541,-105.84918432003,173.034573663757));
#30219=CARTESIAN_POINT('Ctrl Pts',(-58.2166775402229,-105.626390620641,
173.034573714903));
#30220=CARTESIAN_POINT('Ctrl Pts',(-59.4221598772917,-105.403596921252,
173.034573766048));
#30221=CARTESIAN_POINT('Ctrl Pts',(-60.2716537852359,-105.218753966728,
173.898875727171));
#30222=CARTESIAN_POINT('Ctrl Pts',(-61.1211476931802,-105.033911012205,
174.763177688294));
#30223=CARTESIAN_POINT('Ctrl Pts',(-61.1112095794063,-104.940689252971,
175.985485192554));
#30224=CARTESIAN_POINT('Ctrl Pts',(-61.1012714656324,-104.847467493738,
177.207792696815));
#30225=CARTESIAN_POINT('Ctrl Pts',(-60.2319013599317,-104.845866926618,
178.072094585608));
#30226=CARTESIAN_POINT('Ctrl Pts',(-59.362531254231,-104.844266359498,178.936396474401));
#30227=CARTESIAN_POINT('Ctrl Pts',(-58.1371727913281,-104.880616529576,
178.936396423256));
#30228=CARTESIAN_POINT('Ctrl Pts',(-56.9118143284253,-104.916966699654,
178.936396372111));
#30229=CARTESIAN_POINT('Ctrl Pts',(-56.042444294647,-104.915366124867,178.072094410988));
#30230=CARTESIAN_POINT('Ctrl Pts',(-55.1730742608688,-104.91376555008,177.207792449865));
#30231=CARTESIAN_POINT('Ctrl Pts',(-55.1631362488087,-104.820543780003,
175.985484945604));
#30232=CARTESIAN_POINT('Ctrl Pts',(-55.1531982367485,-104.727322009926,
174.763177441344));
#30233=CARTESIAN_POINT('Ctrl Pts',(-56.0026922166152,-104.542479047735,
173.89887555255));
#30234=CARTESIAN_POINT('Ctrl Pts',(-56.8521861964818,-104.357636085544,
173.034573663757));
#30235=CARTESIAN_POINT('Ctrl Pts',(-58.0576685335507,-104.134842386155,
173.034573714903));
#30236=CARTESIAN_POINT('Ctrl Pts',(-59.2631508706195,-103.912048686766,
173.034573766048));
#30237=CARTESIAN_POINT('Ctrl Pts',(-60.1126447785637,-103.727205732243,
173.898875727171));
#30238=CARTESIAN_POINT('Ctrl Pts',(-60.9621386865079,-103.54236277772,174.763177688294));
#30239=CARTESIAN_POINT('Ctrl Pts',(-60.952200572734,-103.449141018486,175.985485192554));
#30240=CARTESIAN_POINT('Ctrl Pts',(-60.9422624589602,-103.355919259252,
177.207792696815));
#30241=CARTESIAN_POINT('Ctrl Pts',(-60.0728923532595,-103.354318692132,
178.072094585608));
#30242=CARTESIAN_POINT('Ctrl Pts',(-59.2035222475588,-103.352718125012,
178.936396474401));
#30243=CARTESIAN_POINT('Ctrl Pts',(-57.9781637846559,-103.389068295091,
178.936396423256));
#30244=CARTESIAN_POINT('Ctrl Pts',(-56.7528053217531,-103.425418465169,
178.936396372111));
#30245=CARTESIAN_POINT('Ctrl Pts',(-55.8834352879748,-103.423817890381,
178.072094410988));
#30246=CARTESIAN_POINT('Ctrl Pts',(-55.0140652541966,-103.422217315594,
177.207792449865));
#30247=CARTESIAN_POINT('Ctrl Pts',(-55.0041272421364,-103.328995545517,
175.985484945604));
#30248=CARTESIAN_POINT('Ctrl Pts',(-54.9941892300763,-103.23577377544,174.763177441344));
#30249=CARTESIAN_POINT('Ctrl Pts',(-55.8436832099429,-103.050930813249,
173.89887555255));
#30250=CARTESIAN_POINT('Ctrl Pts',(-56.6931771898096,-102.866087851059,
173.034573663757));
#30251=CARTESIAN_POINT('Ctrl Pts',(-57.8986595268784,-102.64329415167,173.034573714903));
#30252=CARTESIAN_POINT('Ctrl Pts',(-59.1041418639473,-102.420500452281,
173.034573766048));
#30253=CARTESIAN_POINT('Ctrl Pts',(-59.9536357718915,-102.235657497757,
173.898875727171));
#30254=CARTESIAN_POINT('Ctrl Pts',(-60.8031296798357,-102.050814543234,
174.763177688294));
#30255=CARTESIAN_POINT('Ctrl Pts',(-60.7931915660618,-101.957592784,175.985485192554));
#30256=CARTESIAN_POINT('Ctrl Pts',(-60.783253452288,-101.864371024767,177.207792696815));
#30257=CARTESIAN_POINT('Ctrl Pts',(-59.9138833465873,-101.862770457647,
178.072094585608));
#30258=CARTESIAN_POINT('Ctrl Pts',(-59.0445132408866,-101.861169890527,
178.936396474401));
#30259=CARTESIAN_POINT('Ctrl Pts',(-57.8191547779837,-101.897520060605,
178.936396423256));
#30260=CARTESIAN_POINT('Ctrl Pts',(-56.5937963150808,-101.933870230683,
178.936396372111));
#30261=CARTESIAN_POINT('Ctrl Pts',(-55.7244262813026,-101.932269655896,
178.072094410988));
#30262=CARTESIAN_POINT('Ctrl Pts',(-54.8550562475244,-101.930669081108,
177.207792449865));
#30263=CARTESIAN_POINT('Ctrl Pts',(-54.8451182354642,-101.837447311031,
175.985484945604));
#30264=CARTESIAN_POINT('Ctrl Pts',(-54.8351802234041,-101.744225540954,
174.763177441344));
#30265=CARTESIAN_POINT('Ctrl Pts',(-55.6846742032707,-101.559382578764,
173.89887555255));
#30266=CARTESIAN_POINT('Ctrl Pts',(-56.5341681831374,-101.374539616573,
173.034573663757));
#30267=CARTESIAN_POINT('Ctrl Pts',(-57.7396505202062,-101.151745917184,
173.034573714903));
#30268=CARTESIAN_POINT('Ctrl Pts',(-58.9451328572751,-100.928952217795,
173.034573766048));
#30269=CARTESIAN_POINT('Ctrl Pts',(-59.7946267652193,-100.744109263272,
173.898875727171));
#30270=CARTESIAN_POINT('Ctrl Pts',(-60.6441206731635,-100.559266308748,
174.763177688294));
#30271=CARTESIAN_POINT('Ctrl Pts',(-60.6341825593896,-100.466044549515,
175.985485192554));
#30272=CARTESIAN_POINT('Ctrl Pts',(-60.6242444456157,-100.372822790281,
177.207792696815));
#30273=CARTESIAN_POINT('Ctrl Pts',(-59.754874339915,-100.371222223161,178.072094585608));
#30274=CARTESIAN_POINT('Ctrl Pts',(-58.8855042342143,-100.369621656041,
178.936396474401));
#30275=CARTESIAN_POINT('Ctrl Pts',(-57.6601457713115,-100.405971826119,
178.936396423256));
#30276=CARTESIAN_POINT('Ctrl Pts',(-56.4347873084086,-100.442321996198,
178.936396372111));
#30277=CARTESIAN_POINT('Ctrl Pts',(-55.5654172746304,-100.44072142141,178.072094410988));
#30278=CARTESIAN_POINT('Ctrl Pts',(-54.6960472408521,-100.439120846623,
177.207792449865));
#30279=CARTESIAN_POINT('Ctrl Pts',(-54.686109228792,-100.345899076546,175.985484945604));
#30280=CARTESIAN_POINT('Ctrl Pts',(-54.6761712167318,-100.252677306469,
174.763177441344));
#30281=CARTESIAN_POINT('Ctrl Pts',(-55.5256651965985,-100.067834344278,
173.89887555255));
#30282=CARTESIAN_POINT('Ctrl Pts',(-56.3751591764652,-99.8829913820874,
173.034573663757));
#30283=CARTESIAN_POINT('Ctrl Pts',(-57.580641513534,-99.6601976826983,173.034573714903));
#30284=CARTESIAN_POINT('Ctrl Pts',(-58.7861238506028,-99.4374039833093,
173.034573766048));
#30285=CARTESIAN_POINT('Ctrl Pts',(-59.635617758547,-99.252561028786,173.898875727171));
#30286=CARTESIAN_POINT('Ctrl Pts',(-60.4851116664912,-99.0677180742627,
174.763177688294));
#30287=CARTESIAN_POINT('Ctrl Pts',(-60.4751735527174,-98.9744963150291,
175.985485192554));
#30288=CARTESIAN_POINT('Ctrl Pts',(-60.4652354389435,-98.8812745557954,
177.207792696815));
#30289=CARTESIAN_POINT('Ctrl Pts',(-59.5958653332428,-98.8796739886754,
178.072094585608));
#30290=CARTESIAN_POINT('Ctrl Pts',(-58.7264952275421,-98.8780734215554,
178.936396474401));
#30291=CARTESIAN_POINT('Ctrl Pts',(-57.5011367646392,-98.9144235916337,
178.936396423256));
#30292=CARTESIAN_POINT('Ctrl Pts',(-56.2757783017364,-98.9507737617121,
178.936396372111));
#30293=CARTESIAN_POINT('Ctrl Pts',(-55.4064082679581,-98.9491731869247,
178.072094410988));
#30294=CARTESIAN_POINT('Ctrl Pts',(-61.229590586797,-104.432475997293,178.485485069079));
#30295=CARTESIAN_POINT('Ctrl Pts',(-61.0910183824403,-104.434190515171,
178.657813499464));
#30296=CARTESIAN_POINT('Ctrl Pts',(-60.9344749627642,-104.438317183453,
178.813912312176));
#30297=CARTESIAN_POINT('Ctrl Pts',(-59.7595652153305,-104.46928918342,179.985485138407));
#30298=CARTESIAN_POINT('Ctrl Pts',(-58.1021084653266,-104.551703917706,
179.985485069079));
#30299=CARTESIAN_POINT('Ctrl Pts',(-56.4446517153227,-104.634118651992,
179.985484999752));
#30300=CARTESIAN_POINT('Ctrl Pts',(-55.269742065381,-104.665090641566,178.813912075476));
#30301=CARTESIAN_POINT('Ctrl Pts',(-54.0948324154392,-104.696062631139,
177.6423391512));
#30302=CARTESIAN_POINT('Ctrl Pts',(-54.0848944214593,-104.602840859135,
175.985484901707));
#30303=CARTESIAN_POINT('Ctrl Pts',(-54.0749564274795,-104.50961908713,174.328630652215));
#30304=CARTESIAN_POINT('Ctrl Pts',(-55.2299900490791,-104.292203557853,
173.157057825983));
#30305=CARTESIAN_POINT('Ctrl Pts',(-56.3850236706787,-104.074788028575,
171.985484999752));
#30306=CARTESIAN_POINT('Ctrl Pts',(-58.0226042948486,-103.805929764978,
171.985485069079));
#30307=CARTESIAN_POINT('Ctrl Pts',(-59.6601849190184,-103.537071501381,
171.985485138407));
#30308=CARTESIAN_POINT('Ctrl Pts',(-60.8152184431262,-103.319655982497,
173.157058062683));
#30309=CARTESIAN_POINT('Ctrl Pts',(-60.9691134640793,-103.290687848555,
173.313156769748));
#30310=CARTESIAN_POINT('Ctrl Pts',(-61.1049326680501,-103.263150419372,
173.485485069079));
#30311=CARTESIAN_POINT('Ctrl Pts',(-56.8733667677527,-112.709647553905,
178.072094410988));
#30312=CARTESIAN_POINT('Ctrl Pts',(-56.0039967339745,-112.708046979118,
177.207792449865));
#30313=CARTESIAN_POINT('Ctrl Pts',(-55.9940587219143,-112.614825209041,
175.985484945604));
#30314=CARTESIAN_POINT('Ctrl Pts',(-55.9841207098542,-112.521603438964,
174.763177441344));
#30315=CARTESIAN_POINT('Ctrl Pts',(-56.8336146897208,-112.336760476773,
173.89887555255));
#30316=CARTESIAN_POINT('Ctrl Pts',(-57.6831086695875,-112.151917514582,
173.034573663757));
#30317=CARTESIAN_POINT('Ctrl Pts',(-58.8885910066563,-111.929123815193,
173.034573714903));
#30318=CARTESIAN_POINT('Ctrl Pts',(-60.0940733437252,-111.706330115804,
173.034573766048));
#30319=CARTESIAN_POINT('Ctrl Pts',(-60.9435672516694,-111.521487161281,
173.898875727171));
#30320=CARTESIAN_POINT('Ctrl Pts',(-61.7930611596136,-111.336644206758,
174.763177688294));
#30321=CARTESIAN_POINT('Ctrl Pts',(-61.7831230458397,-111.243422447524,
175.985485192554));
#30322=CARTESIAN_POINT('Ctrl Pts',(-61.7731849320658,-111.15020068829,177.207792696815));
#30323=CARTESIAN_POINT('Ctrl Pts',(-60.9038148263651,-111.14860012117,178.072094585608));
#30324=CARTESIAN_POINT('Ctrl Pts',(-60.0344447206644,-111.14699955405,178.936396474401));
#30325=CARTESIAN_POINT('Ctrl Pts',(-58.8090862577616,-111.183349724129,
178.936396423256));
#30326=CARTESIAN_POINT('Ctrl Pts',(-57.5837277948587,-111.219699894207,
178.936396372111));
#30327=CARTESIAN_POINT('Ctrl Pts',(-56.7143577610805,-111.21809931942,178.072094410988));
#30328=CARTESIAN_POINT('Ctrl Pts',(-55.8449877273022,-111.216498744632,
177.207792449865));
#30329=CARTESIAN_POINT('Ctrl Pts',(-55.8350497152421,-111.123276974555,
175.985484945604));
#30330=CARTESIAN_POINT('Ctrl Pts',(-55.8251117031819,-111.030055204478,
174.763177441344));
#30331=CARTESIAN_POINT('Ctrl Pts',(-56.6746056830486,-110.845212242287,
173.89887555255));
#30332=CARTESIAN_POINT('Ctrl Pts',(-57.5240996629153,-110.660369280097,
173.034573663757));
#30333=CARTESIAN_POINT('Ctrl Pts',(-58.7295819999841,-110.437575580708,
173.034573714903));
#30334=CARTESIAN_POINT('Ctrl Pts',(-59.9350643370529,-110.214781881319,
173.034573766048));
#30335=CARTESIAN_POINT('Ctrl Pts',(-60.7845582449971,-110.029938926795,
173.898875727171));
#30336=CARTESIAN_POINT('Ctrl Pts',(-61.6340521529414,-109.845095972272,
174.763177688294));
#30337=CARTESIAN_POINT('Ctrl Pts',(-61.6241140391675,-109.751874213038,
175.985485192554));
#30338=CARTESIAN_POINT('Ctrl Pts',(-61.6141759253936,-109.658652453805,
177.207792696815));
#30339=CARTESIAN_POINT('Ctrl Pts',(-60.7448058196929,-109.657051886685,
178.072094585608));
#30340=CARTESIAN_POINT('Ctrl Pts',(-59.8754357139922,-109.655451319565,
178.936396474401));
#30341=CARTESIAN_POINT('Ctrl Pts',(-58.6500772510893,-109.691801489643,
178.936396423256));
#30342=CARTESIAN_POINT('Ctrl Pts',(-57.4247187881865,-109.728151659721,
178.936396372111));
#30343=CARTESIAN_POINT('Ctrl Pts',(-56.5553487544082,-109.726551084934,
178.072094410988));
#30344=CARTESIAN_POINT('Ctrl Pts',(-55.68597872063,-109.724950510147,177.207792449865));
#30345=CARTESIAN_POINT('Ctrl Pts',(-55.6760407085698,-109.63172874007,175.985484945604));
#30346=CARTESIAN_POINT('Ctrl Pts',(-55.6661026965097,-109.538506969993,
174.763177441344));
#30347=CARTESIAN_POINT('Ctrl Pts',(-56.5155966763764,-109.353664007802,
173.89887555255));
#30348=CARTESIAN_POINT('Ctrl Pts',(-57.365090656243,-109.168821045611,173.034573663757));
#30349=CARTESIAN_POINT('Ctrl Pts',(-58.5705729933119,-108.946027346222,
173.034573714903));
#30350=CARTESIAN_POINT('Ctrl Pts',(-59.7760553303807,-108.723233646833,
173.034573766048));
#30351=CARTESIAN_POINT('Ctrl Pts',(-60.6255492383249,-108.53839069231,173.898875727171));
#30352=CARTESIAN_POINT('Ctrl Pts',(-61.4750431462691,-108.353547737786,
174.763177688294));
#30353=CARTESIAN_POINT('Ctrl Pts',(-61.4651050324952,-108.260325978553,
175.985485192554));
#30354=CARTESIAN_POINT('Ctrl Pts',(-61.4551669187214,-108.167104219319,
177.207792696815));
#30355=CARTESIAN_POINT('Ctrl Pts',(-60.5857968130207,-108.165503652199,
178.072094585608));
#30356=CARTESIAN_POINT('Ctrl Pts',(-59.71642670732,-108.163903085079,178.936396474401));
#30357=CARTESIAN_POINT('Ctrl Pts',(-58.4910682444171,-108.200253255158,
178.936396423256));
#30358=CARTESIAN_POINT('Ctrl Pts',(-57.2657097815143,-108.236603425236,
178.936396372111));
#30359=CARTESIAN_POINT('Ctrl Pts',(-56.396339747736,-108.235002850448,178.072094410988));
#30360=CARTESIAN_POINT('Ctrl Pts',(-55.5269697139578,-108.233402275661,
177.207792449865));
#30361=CARTESIAN_POINT('Ctrl Pts',(-55.5170317018976,-108.140180505584,
175.985484945604));
#30362=CARTESIAN_POINT('Ctrl Pts',(-55.5070936898375,-108.046958735507,
174.763177441344));
#30363=CARTESIAN_POINT('Ctrl Pts',(-56.3565876697041,-107.862115773316,
173.89887555255));
#30364=CARTESIAN_POINT('Ctrl Pts',(-57.2060816495708,-107.677272811126,
173.034573663757));
#30365=CARTESIAN_POINT('Ctrl Pts',(-58.4115639866396,-107.454479111736,
173.034573714903));
#30366=CARTESIAN_POINT('Ctrl Pts',(-59.6170463237085,-107.231685412347,
173.034573766048));
#30367=CARTESIAN_POINT('Ctrl Pts',(-60.4665402316527,-107.046842457824,
173.898875727171));
#30368=CARTESIAN_POINT('Ctrl Pts',(-61.3160341395969,-106.861999503301,
174.763177688294));
#30369=CARTESIAN_POINT('Ctrl Pts',(-61.306096025823,-106.768777744067,175.985485192554));
#30370=CARTESIAN_POINT('Ctrl Pts',(-61.2961579120492,-106.675555984834,
177.207792696815));
#30371=CARTESIAN_POINT('Ctrl Pts',(-60.4267878063484,-106.673955417714,
178.072094585608));
#30372=CARTESIAN_POINT('Ctrl Pts',(-59.5574177006478,-106.672354850594,
178.936396474401));
#30373=CARTESIAN_POINT('Ctrl Pts',(-58.3320592377449,-106.708705020672,
178.936396423256));
#30374=CARTESIAN_POINT('Ctrl Pts',(-57.106700774842,-106.74505519075,178.936396372111));
#30375=CARTESIAN_POINT('Ctrl Pts',(-56.2373307410638,-106.743454615963,
178.072094410988));
#30376=CARTESIAN_POINT('Ctrl Pts',(-55.3679607072856,-106.741854041175,
177.207792449865));
#30377=CARTESIAN_POINT('Ctrl Pts',(-55.3580226952254,-106.648632271098,
175.985484945604));
#30378=CARTESIAN_POINT('Ctrl Pts',(-55.3480846831652,-106.555410501021,
174.763177441344));
#30379=CARTESIAN_POINT('Ctrl Pts',(-56.1975786630319,-106.370567538831,
173.89887555255));
#30380=CARTESIAN_POINT('Ctrl Pts',(-57.0470726428986,-106.18572457664,173.034573663757));
#30381=CARTESIAN_POINT('Ctrl Pts',(-58.2525549799674,-105.962930877251,
173.034573714903));
#30382=CARTESIAN_POINT('Ctrl Pts',(-59.4580373170363,-105.740137177862,
173.034573766048));
#30383=CARTESIAN_POINT('Ctrl Pts',(-60.3075312249805,-105.555294223339,
173.898875727171));
#30384=CARTESIAN_POINT('Ctrl Pts',(-61.1570251329247,-105.370451268815,
174.763177688294));
#30385=CARTESIAN_POINT('Ctrl Pts',(-61.1470870191508,-105.277229509582,
175.985485192554));
#30386=CARTESIAN_POINT('Ctrl Pts',(-61.1371489053769,-105.184007750348,
177.207792696815));
#30387=CARTESIAN_POINT('Ctrl Pts',(-60.2677787996762,-105.182407183228,
178.072094585608));
#30388=CARTESIAN_POINT('Ctrl Pts',(-59.3984086939755,-105.180806616108,
178.936396474401));
#30389=CARTESIAN_POINT('Ctrl Pts',(-58.1730502310727,-105.217156786186,
178.936396423256));
#30390=CARTESIAN_POINT('Ctrl Pts',(-56.9476917681698,-105.253506956265,
178.936396372111));
#30391=CARTESIAN_POINT('Ctrl Pts',(-56.0783217343916,-105.251906381477,
178.072094410988));
#30392=CARTESIAN_POINT('Ctrl Pts',(-55.2089517006133,-105.25030580669,177.207792449865));
#30393=CARTESIAN_POINT('Ctrl Pts',(-55.1990136885532,-105.157084036613,
175.985484945604));
#30394=CARTESIAN_POINT('Ctrl Pts',(-55.189075676493,-105.063862266536,174.763177441344));
#30395=CARTESIAN_POINT('Ctrl Pts',(-56.0385696563597,-104.879019304345,
173.89887555255));
#30396=CARTESIAN_POINT('Ctrl Pts',(-56.8880636362264,-104.694176342154,
173.034573663757));
#30397=CARTESIAN_POINT('Ctrl Pts',(-58.0935459732952,-104.471382642765,
173.034573714903));
#30398=CARTESIAN_POINT('Ctrl Pts',(-59.299028310364,-104.248588943376,173.034573766048));
#30399=CARTESIAN_POINT('Ctrl Pts',(-60.1485222183082,-104.063745988853,
173.898875727171));
#30400=CARTESIAN_POINT('Ctrl Pts',(-60.9980161262524,-103.87890303433,174.763177688294));
#30401=CARTESIAN_POINT('Ctrl Pts',(-60.9880780124786,-103.785681275096,
175.985485192554));
#30402=CARTESIAN_POINT('Ctrl Pts',(-60.9781398987047,-103.692459515862,
177.207792696815));
#30403=CARTESIAN_POINT('Ctrl Pts',(-60.108769793004,-103.690858948742,178.072094585608));
#30404=CARTESIAN_POINT('Ctrl Pts',(-59.2393996873033,-103.689258381622,
178.936396474401));
#30405=CARTESIAN_POINT('Ctrl Pts',(-58.0140412244004,-103.725608551701,
178.936396423256));
#30406=CARTESIAN_POINT('Ctrl Pts',(-56.7886827614976,-103.761958721779,
178.936396372111));
#30407=CARTESIAN_POINT('Ctrl Pts',(-55.9193127277193,-103.760358146992,
178.072094410988));
#30408=CARTESIAN_POINT('Ctrl Pts',(-55.0499426939411,-103.758757572204,
177.207792449865));
#30409=CARTESIAN_POINT('Ctrl Pts',(-55.0400046818809,-103.665535802127,
175.985484945604));
#30410=CARTESIAN_POINT('Ctrl Pts',(-55.0300666698208,-103.57231403205,174.763177441344));
#30411=CARTESIAN_POINT('Ctrl Pts',(-55.8795606496874,-103.387471069859,
173.89887555255));
#30412=CARTESIAN_POINT('Ctrl Pts',(-56.7290546295541,-103.202628107669,
173.034573663757));
#30413=CARTESIAN_POINT('Ctrl Pts',(-57.934536966623,-102.97983440828,173.034573714903));
#30414=CARTESIAN_POINT('Ctrl Pts',(-59.1400193036918,-102.757040708891,
173.034573766048));
#30415=CARTESIAN_POINT('Ctrl Pts',(-59.989513211636,-102.572197754367,173.898875727171));
#30416=CARTESIAN_POINT('Ctrl Pts',(-60.8390071195802,-102.387354799844,
174.763177688294));
#30417=CARTESIAN_POINT('Ctrl Pts',(-60.8290690058063,-102.29413304061,175.985485192554));
#30418=CARTESIAN_POINT('Ctrl Pts',(-60.8191308920325,-102.200911281377,
177.207792696815));
#30419=CARTESIAN_POINT('Ctrl Pts',(-59.9497607863318,-102.199310714257,
178.072094585608));
#30420=CARTESIAN_POINT('Ctrl Pts',(-59.0803906806311,-102.197710147137,
178.936396474401));
#30421=CARTESIAN_POINT('Ctrl Pts',(-57.8550322177282,-102.234060317215,
178.936396423256));
#30422=CARTESIAN_POINT('Ctrl Pts',(-56.6296737548253,-102.270410487293,
178.936396372111));
#30423=CARTESIAN_POINT('Ctrl Pts',(-55.7603037210471,-102.268809912506,
178.072094410988));
#30424=CARTESIAN_POINT('Ctrl Pts',(-54.8909336872689,-102.267209337719,
177.207792449865));
#30425=CARTESIAN_POINT('Ctrl Pts',(-54.8809956752087,-102.173987567642,
175.985484945604));
#30426=CARTESIAN_POINT('Ctrl Pts',(-54.8710576631486,-102.080765797565,
174.763177441344));
#30427=CARTESIAN_POINT('Ctrl Pts',(-55.7205516430152,-101.895922835374,
173.89887555255));
#30428=CARTESIAN_POINT('Ctrl Pts',(-56.5700456228819,-101.711079873183,
173.034573663757));
#30429=CARTESIAN_POINT('Ctrl Pts',(-57.7755279599507,-101.488286173794,
173.034573714903));
#30430=CARTESIAN_POINT('Ctrl Pts',(-58.9810102970196,-101.265492474405,
173.034573766048));
#30431=CARTESIAN_POINT('Ctrl Pts',(-59.8305042049638,-101.080649519882,
173.898875727171));
#30432=CARTESIAN_POINT('Ctrl Pts',(-60.679998112908,-100.895806565358,174.763177688294));
#30433=CARTESIAN_POINT('Ctrl Pts',(-60.6700599991341,-100.802584806125,
175.985485192554));
#30434=CARTESIAN_POINT('Ctrl Pts',(-60.6601218853602,-100.709363046891,
177.207792696815));
#30435=CARTESIAN_POINT('Ctrl Pts',(-59.7907517796595,-100.707762479771,
178.072094585608));
#30436=CARTESIAN_POINT('Ctrl Pts',(-58.9213816739588,-100.706161912651,
178.936396474401));
#30437=CARTESIAN_POINT('Ctrl Pts',(-57.696023211056,-100.742512082729,178.936396423256));
#30438=CARTESIAN_POINT('Ctrl Pts',(-56.4706647481531,-100.778862252808,
178.936396372111));
#30439=CARTESIAN_POINT('Ctrl Pts',(-55.6012947143749,-100.77726167802,178.072094410988));
#30440=CARTESIAN_POINT('Ctrl Pts',(-54.7319246805966,-100.775661103233,
177.207792449865));
#30441=CARTESIAN_POINT('Ctrl Pts',(-54.7219866685365,-100.682439333156,
175.985484945604));
#30442=CARTESIAN_POINT('Ctrl Pts',(-54.7120486564763,-100.589217563079,
174.763177441344));
#30443=CARTESIAN_POINT('Ctrl Pts',(-55.561542636343,-100.404374600888,173.89887555255));
#30444=CARTESIAN_POINT('Ctrl Pts',(-56.4110366162097,-100.219531638698,
173.034573663757));
#30445=CARTESIAN_POINT('Ctrl Pts',(-57.6165189532785,-99.9967379393085,
173.034573714903));
#30446=CARTESIAN_POINT('Ctrl Pts',(-58.8220012903473,-99.7739442399195,
173.034573766048));
#30447=CARTESIAN_POINT('Ctrl Pts',(-59.6714951982915,-99.5891012853962,
173.898875727171));
#30448=CARTESIAN_POINT('Ctrl Pts',(-60.5209891062358,-99.4042583308729,
174.763177688294));
#30449=CARTESIAN_POINT('Ctrl Pts',(-60.5110509924619,-99.3110365716392,
175.985485192554));
#30450=CARTESIAN_POINT('Ctrl Pts',(-60.501112878688,-99.2178148124055,177.207792696815));
#30451=CARTESIAN_POINT('Ctrl Pts',(-59.6317427729873,-99.2162142452855,
178.072094585608));
#30452=CARTESIAN_POINT('Ctrl Pts',(-58.7623726672866,-99.2146136781656,
178.936396474401));
#30453=CARTESIAN_POINT('Ctrl Pts',(-57.5370142043838,-99.2509638482439,
178.936396423256));
#30454=CARTESIAN_POINT('Ctrl Pts',(-56.3116557414809,-99.2873140183222,
178.936396372111));
#30455=CARTESIAN_POINT('Ctrl Pts',(-55.4422857077027,-99.2857134435348,
178.072094410988));
#30456=CARTESIAN_POINT('Ctrl Pts',(-54.5729156739244,-99.2841128687474,
177.207792449865));
#30457=CARTESIAN_POINT('Ctrl Pts',(-54.5629776618643,-99.1908910986704,
175.985484945604));
#30458=CARTESIAN_POINT('Ctrl Pts',(-54.5530396498041,-99.0976693285933,
174.763177441344));
#30459=CARTESIAN_POINT('Ctrl Pts',(-55.4025336296708,-98.9128263664026,
173.89887555255));
#30460=CARTESIAN_POINT('Ctrl Pts',(-56.2520276095374,-98.727983404212,173.034573663757));
#30461=CARTESIAN_POINT('Ctrl Pts',(-57.4575099466063,-98.5051897048229,
173.034573714903));
#30462=CARTESIAN_POINT('Ctrl Pts',(-58.6629922836751,-98.2823960054338,
173.034573766048));
#30463=CARTESIAN_POINT('Ctrl Pts',(-59.5124861916193,-98.0975530509106,
173.898875727171));
#30464=CARTESIAN_POINT('Ctrl Pts',(-60.3619800995635,-97.9127100963873,
174.763177688294));
#30465=CARTESIAN_POINT('Ctrl Pts',(-60.3520419857897,-97.8194883371536,
175.985485192554));
#30466=CARTESIAN_POINT('Ctrl Pts',(-60.3421038720158,-97.7262665779199,
177.207792696815));
#30467=CARTESIAN_POINT('Ctrl Pts',(-59.4727337663151,-97.7246660108,178.072094585608));
#30468=CARTESIAN_POINT('Ctrl Pts',(-58.6033636606144,-97.72306544368,178.936396474401));
#30469=CARTESIAN_POINT('Ctrl Pts',(-57.3780051977115,-97.7594156137583,
178.936396423256));
#30470=CARTESIAN_POINT('Ctrl Pts',(-56.1526467348087,-97.7957657838366,
178.936396372111));
#30471=CARTESIAN_POINT('Ctrl Pts',(-55.2832767010304,-97.7941652090492,
178.072094410988));
#30472=CARTESIAN_POINT('Ctrl Pts',(-56.1707931031902,-113.117197303651,
178.813912075476));
#30473=CARTESIAN_POINT('Ctrl Pts',(-54.9958834532485,-113.148169293224,
177.6423391512));
#30474=CARTESIAN_POINT('Ctrl Pts',(-54.9859454592686,-113.05494752122,175.985484901707));
#30475=CARTESIAN_POINT('Ctrl Pts',(-54.9760074652888,-112.961725749215,
174.328630652215));
#30476=CARTESIAN_POINT('Ctrl Pts',(-56.1310410868884,-112.744310219938,
173.157057825983));
#30477=CARTESIAN_POINT('Ctrl Pts',(-57.286074708488,-112.52689469066,171.985484999752));
#30478=CARTESIAN_POINT('Ctrl Pts',(-58.9236553326579,-112.258036427063,
171.985485069079));
#30479=CARTESIAN_POINT('Ctrl Pts',(-60.5612359568277,-111.989178163466,
171.985485138407));
#30480=CARTESIAN_POINT('Ctrl Pts',(-61.7162694809355,-111.771762644582,
173.157058062683));
#30481=CARTESIAN_POINT('Ctrl Pts',(-62.8713030050432,-111.554347125698,
174.328630986959));
#30482=CARTESIAN_POINT('Ctrl Pts',(-62.861364873189,-111.461125368392,175.985485236451));
#30483=CARTESIAN_POINT('Ctrl Pts',(-62.8514267413349,-111.367903611086,
177.642339485944));
#30484=CARTESIAN_POINT('Ctrl Pts',(-61.6765169939012,-111.398875611052,
178.813912312176));
#30485=CARTESIAN_POINT('Ctrl Pts',(-60.5016072464676,-111.429847611019,
179.985485138407));
#30486=CARTESIAN_POINT('Ctrl Pts',(-58.8441504964637,-111.512262345305,
179.985485069079));
#30487=CARTESIAN_POINT('Ctrl Pts',(-57.1866937464598,-111.594677079592,
179.985484999752));
#30488=CARTESIAN_POINT('Ctrl Pts',(-56.011784096518,-111.625649069165,178.813912075476));
#30489=CARTESIAN_POINT('Ctrl Pts',(-54.8368744465762,-111.656621058739,
177.6423391512));
#30490=CARTESIAN_POINT('Ctrl Pts',(-54.8269364525964,-111.563399286734,
175.985484901707));
#30491=CARTESIAN_POINT('Ctrl Pts',(-54.8169984586165,-111.47017751473,174.328630652215));
#30492=CARTESIAN_POINT('Ctrl Pts',(-55.9720320802161,-111.252761985452,
173.157057825983));
#30493=CARTESIAN_POINT('Ctrl Pts',(-57.1270657018158,-111.035346456175,
171.985484999752));
#30494=CARTESIAN_POINT('Ctrl Pts',(-58.7646463259856,-110.766488192578,
171.985485069079));
#30495=CARTESIAN_POINT('Ctrl Pts',(-60.4022269501555,-110.497629928981,
171.985485138407));
#30496=CARTESIAN_POINT('Ctrl Pts',(-61.5572604742632,-110.280214410097,
173.157058062683));
#30497=CARTESIAN_POINT('Ctrl Pts',(-62.712293998371,-110.062798891212,174.328630986959));
#30498=CARTESIAN_POINT('Ctrl Pts',(-62.7023558665168,-109.969577133906,
175.985485236451));
#30499=CARTESIAN_POINT('Ctrl Pts',(-62.6924177346626,-109.8763553766,177.642339485944));
#30500=CARTESIAN_POINT('Ctrl Pts',(-61.517507987229,-109.907327376567,178.813912312176));
#30501=CARTESIAN_POINT('Ctrl Pts',(-60.3425982397954,-109.938299376534,
179.985485138407));
#30502=CARTESIAN_POINT('Ctrl Pts',(-58.6851414897915,-110.02071411082,179.985485069079));
#30503=CARTESIAN_POINT('Ctrl Pts',(-57.0276847397876,-110.103128845106,
179.985484999752));
#30504=CARTESIAN_POINT('Ctrl Pts',(-55.8527750898458,-110.13410083468,178.813912075476));
#30505=CARTESIAN_POINT('Ctrl Pts',(-54.677865439904,-110.165072824253,177.6423391512));
#30506=CARTESIAN_POINT('Ctrl Pts',(-54.6679274459242,-110.071851052249,
175.985484901707));
#30507=CARTESIAN_POINT('Ctrl Pts',(-54.6579894519443,-109.978629280244,
174.328630652215));
#30508=CARTESIAN_POINT('Ctrl Pts',(-55.8130230735439,-109.761213750967,
173.157057825983));
#30509=CARTESIAN_POINT('Ctrl Pts',(-56.9680566951435,-109.543798221689,
171.985484999752));
#30510=CARTESIAN_POINT('Ctrl Pts',(-58.6056373193134,-109.274939958092,
171.985485069079));
#30511=CARTESIAN_POINT('Ctrl Pts',(-60.2432179434833,-109.006081694495,
171.985485138407));
#30512=CARTESIAN_POINT('Ctrl Pts',(-61.398251467591,-108.788666175611,173.157058062683));
#30513=CARTESIAN_POINT('Ctrl Pts',(-62.5532849916988,-108.571250656727,
174.328630986959));
#30514=CARTESIAN_POINT('Ctrl Pts',(-62.5433468598446,-108.478028899421,
175.985485236451));
#30515=CARTESIAN_POINT('Ctrl Pts',(-62.5334087279904,-108.384807142114,
177.642339485944));
#30516=CARTESIAN_POINT('Ctrl Pts',(-61.3584989805568,-108.415779142081,
178.813912312176));
#30517=CARTESIAN_POINT('Ctrl Pts',(-60.1835892331231,-108.446751142048,
179.985485138407));
#30518=CARTESIAN_POINT('Ctrl Pts',(-58.5261324831192,-108.529165876334,
179.985485069079));
#30519=CARTESIAN_POINT('Ctrl Pts',(-56.8686757331153,-108.611580610621,
179.985484999752));
#30520=CARTESIAN_POINT('Ctrl Pts',(-55.6937660831736,-108.642552600194,
178.813912075476));
#30521=CARTESIAN_POINT('Ctrl Pts',(-54.5188564332318,-108.673524589768,
177.6423391512));
#30522=CARTESIAN_POINT('Ctrl Pts',(-54.5089184392519,-108.580302817763,
175.985484901707));
#30523=CARTESIAN_POINT('Ctrl Pts',(-54.4989804452721,-108.487081045759,
174.328630652215));
#30524=CARTESIAN_POINT('Ctrl Pts',(-55.6540140668717,-108.269665516481,
173.157057825983));
#30525=CARTESIAN_POINT('Ctrl Pts',(-56.8090476884713,-108.052249987204,
171.985484999752));
#30526=CARTESIAN_POINT('Ctrl Pts',(-58.4466283126412,-107.783391723607,
171.985485069079));
#30527=CARTESIAN_POINT('Ctrl Pts',(-60.084208936811,-107.51453346001,171.985485138407));
#30528=CARTESIAN_POINT('Ctrl Pts',(-61.2392424609188,-107.297117941125,
173.157058062683));
#30529=CARTESIAN_POINT('Ctrl Pts',(-62.3942759850265,-107.079702422241,
174.328630986959));
#30530=CARTESIAN_POINT('Ctrl Pts',(-62.3843378531723,-106.986480664935,
175.985485236451));
#30531=CARTESIAN_POINT('Ctrl Pts',(-62.3743997213182,-106.893258907629,
177.642339485944));
#30532=CARTESIAN_POINT('Ctrl Pts',(-61.1994899738845,-106.924230907596,
178.813912312176));
#30533=CARTESIAN_POINT('Ctrl Pts',(-60.0245802264509,-106.955202907562,
179.985485138407));
#30534=CARTESIAN_POINT('Ctrl Pts',(-58.367123476447,-107.037617641849,179.985485069079));
#30535=CARTESIAN_POINT('Ctrl Pts',(-56.7096667264431,-107.120032376135,
179.985484999752));
#30536=CARTESIAN_POINT('Ctrl Pts',(-55.5347570765013,-107.151004365708,
178.813912075476));
#30537=CARTESIAN_POINT('Ctrl Pts',(-54.3598474265596,-107.181976355282,
177.6423391512));
#30538=CARTESIAN_POINT('Ctrl Pts',(-54.3499094325797,-107.088754583277,
175.985484901707));
#30539=CARTESIAN_POINT('Ctrl Pts',(-54.3399714385998,-106.995532811273,
174.328630652215));
#30540=CARTESIAN_POINT('Ctrl Pts',(-55.4950050601995,-106.778117281995,
173.157057825983));
#30541=CARTESIAN_POINT('Ctrl Pts',(-56.6500386817991,-106.560701752718,
171.985484999752));
#30542=CARTESIAN_POINT('Ctrl Pts',(-58.2876193059689,-106.291843489121,
171.985485069079));
#30543=CARTESIAN_POINT('Ctrl Pts',(-59.9251999301388,-106.022985225524,
171.985485138407));
#30544=CARTESIAN_POINT('Ctrl Pts',(-61.0802334542465,-105.80556970664,173.157058062683));
#30545=CARTESIAN_POINT('Ctrl Pts',(-62.2352669783543,-105.588154187756,
174.328630986959));
#30546=CARTESIAN_POINT('Ctrl Pts',(-62.2253288465001,-105.494932430449,
175.985485236451));
#30547=CARTESIAN_POINT('Ctrl Pts',(-62.2153907146459,-105.401710673143,
177.642339485944));
#30548=CARTESIAN_POINT('Ctrl Pts',(-61.0404809672123,-105.43268267311,178.813912312176));
#30549=CARTESIAN_POINT('Ctrl Pts',(-59.8655712197787,-105.463654673077,
179.985485138407));
#30550=CARTESIAN_POINT('Ctrl Pts',(-58.2081144697748,-105.546069407363,
179.985485069079));
#30551=CARTESIAN_POINT('Ctrl Pts',(-56.5506577197709,-105.628484141649,
179.985484999752));
#30552=CARTESIAN_POINT('Ctrl Pts',(-55.3757480698291,-105.659456131223,
178.813912075476));
#30553=CARTESIAN_POINT('Ctrl Pts',(-54.2008384198873,-105.690428120796,
177.6423391512));
#30554=CARTESIAN_POINT('Ctrl Pts',(-54.1909004259075,-105.597206348792,
175.985484901707));
#30555=CARTESIAN_POINT('Ctrl Pts',(-54.1809624319276,-105.503984576787,
174.328630652215));
#30556=CARTESIAN_POINT('Ctrl Pts',(-55.3359960535272,-105.28656904751,173.157057825983));
#30557=CARTESIAN_POINT('Ctrl Pts',(-56.4910296751268,-105.069153518232,
171.985484999752));
#30558=CARTESIAN_POINT('Ctrl Pts',(-58.1286102992967,-104.800295254635,
171.985485069079));
#30559=CARTESIAN_POINT('Ctrl Pts',(-59.7661909234666,-104.531436991038,
171.985485138407));
#30560=CARTESIAN_POINT('Ctrl Pts',(-60.9212244475743,-104.314021472154,
173.157058062683));
#30561=CARTESIAN_POINT('Ctrl Pts',(-62.0762579716821,-104.09660595327,174.328630986959));
#30562=CARTESIAN_POINT('Ctrl Pts',(-62.0663198398279,-104.003384195964,
175.985485236451));
#30563=CARTESIAN_POINT('Ctrl Pts',(-62.0563817079737,-103.910162438658,
177.642339485944));
#30564=CARTESIAN_POINT('Ctrl Pts',(-60.8814719605401,-103.941134438624,
178.813912312176));
#30565=CARTESIAN_POINT('Ctrl Pts',(-59.7065622131064,-103.972106438591,
179.985485138407));
#30566=CARTESIAN_POINT('Ctrl Pts',(-58.0491054631025,-104.054521172878,
179.985485069079));
#30567=CARTESIAN_POINT('Ctrl Pts',(-56.3916487130987,-104.136935907164,
179.985484999752));
#30568=CARTESIAN_POINT('Ctrl Pts',(-55.2167390631569,-104.167907896737,
178.813912075476));
#30569=CARTESIAN_POINT('Ctrl Pts',(-54.0418294132151,-104.198879886311,
177.6423391512));
#30570=CARTESIAN_POINT('Ctrl Pts',(-54.0318914192353,-104.105658114306,
175.985484901707));
#30571=CARTESIAN_POINT('Ctrl Pts',(-54.0219534252554,-104.012436342302,
174.328630652215));
#30572=CARTESIAN_POINT('Ctrl Pts',(-55.176987046855,-103.795020813024,173.157057825983));
#30573=CARTESIAN_POINT('Ctrl Pts',(-56.3320206684546,-103.577605283747,
171.985484999752));
#30574=CARTESIAN_POINT('Ctrl Pts',(-57.9696012926245,-103.30874702015,171.985485069079));
#30575=CARTESIAN_POINT('Ctrl Pts',(-59.6071819167943,-103.039888756553,
171.985485138407));
#30576=CARTESIAN_POINT('Ctrl Pts',(-60.7622154409021,-102.822473237669,
173.157058062683));
#30577=CARTESIAN_POINT('Ctrl Pts',(-61.9172489650099,-102.605057718784,
174.328630986959));
#30578=CARTESIAN_POINT('Ctrl Pts',(-61.9073108331557,-102.511835961478,
175.985485236451));
#30579=CARTESIAN_POINT('Ctrl Pts',(-61.8973727013015,-102.418614204172,
177.642339485944));
#30580=CARTESIAN_POINT('Ctrl Pts',(-60.7224629538678,-102.449586204139,
178.813912312176));
#30581=CARTESIAN_POINT('Ctrl Pts',(-59.5475532064342,-102.480558204106,
179.985485138407));
#30582=CARTESIAN_POINT('Ctrl Pts',(-57.8900964564303,-102.562972938392,
179.985485069079));
#30583=CARTESIAN_POINT('Ctrl Pts',(-56.2326397064264,-102.645387672678,
179.985484999752));
#30584=CARTESIAN_POINT('Ctrl Pts',(-55.0577300564847,-102.676359662252,
178.813912075476));
#30585=CARTESIAN_POINT('Ctrl Pts',(-53.8828204065429,-102.707331651825,
177.6423391512));
#30586=CARTESIAN_POINT('Ctrl Pts',(-53.872882412563,-102.614109879821,175.985484901707));
#30587=CARTESIAN_POINT('Ctrl Pts',(-53.8629444185832,-102.520888107816,
174.328630652215));
#30588=CARTESIAN_POINT('Ctrl Pts',(-55.0179780401828,-102.303472578539,
173.157057825983));
#30589=CARTESIAN_POINT('Ctrl Pts',(-56.1730116617824,-102.086057049261,
171.985484999752));
#30590=CARTESIAN_POINT('Ctrl Pts',(-57.8105922859523,-101.817198785664,
171.985485069079));
#30591=CARTESIAN_POINT('Ctrl Pts',(-59.4481729101221,-101.548340522067,
171.985485138407));
#30592=CARTESIAN_POINT('Ctrl Pts',(-60.6032064342299,-101.330925003183,
173.157058062683));
#30593=CARTESIAN_POINT('Ctrl Pts',(-61.7582399583376,-101.113509484299,
174.328630986959));
#30594=CARTESIAN_POINT('Ctrl Pts',(-61.7483018264834,-101.020287726993,
175.985485236451));
#30595=CARTESIAN_POINT('Ctrl Pts',(-61.7383636946293,-100.927065969686,
177.642339485944));
#30596=CARTESIAN_POINT('Ctrl Pts',(-60.5634539471956,-100.958037969653,
178.813912312176));
#30597=CARTESIAN_POINT('Ctrl Pts',(-59.388544199762,-100.98900996962,179.985485138407));
#30598=CARTESIAN_POINT('Ctrl Pts',(-57.7310874497581,-101.071424703906,
179.985485069079));
#30599=CARTESIAN_POINT('Ctrl Pts',(-56.0736306997542,-101.153839438193,
179.985484999752));
#30600=CARTESIAN_POINT('Ctrl Pts',(-54.8987210498124,-101.184811427766,
178.813912075476));
#30601=CARTESIAN_POINT('Ctrl Pts',(-53.7238113998707,-101.21578341734,177.6423391512));
#30602=CARTESIAN_POINT('Ctrl Pts',(-53.7138734058908,-101.122561645335,
175.985484901707));
#30603=CARTESIAN_POINT('Ctrl Pts',(-53.7039354119109,-101.029339873331,
174.328630652215));
#30604=CARTESIAN_POINT('Ctrl Pts',(-54.8589690335105,-100.811924344053,
173.157057825983));
#30605=CARTESIAN_POINT('Ctrl Pts',(-56.0140026551102,-100.594508814776,
171.985484999752));
#30606=CARTESIAN_POINT('Ctrl Pts',(-57.65158327928,-100.325650551179,171.985485069079));
#30607=CARTESIAN_POINT('Ctrl Pts',(-59.2891639034499,-100.056792287582,
171.985485138407));
#30608=CARTESIAN_POINT('Ctrl Pts',(-60.4441974275576,-99.8393767686974,
173.157058062683));
#30609=CARTESIAN_POINT('Ctrl Pts',(-61.5992309516654,-99.6219612498133,
174.328630986959));
#30610=CARTESIAN_POINT('Ctrl Pts',(-61.5892928198112,-99.528739492507,175.985485236451));
#30611=CARTESIAN_POINT('Ctrl Pts',(-61.579354687957,-99.4355177352008,177.642339485944));
#30612=CARTESIAN_POINT('Ctrl Pts',(-60.4044449405234,-99.4664897351676,
178.813912312176));
#30613=CARTESIAN_POINT('Ctrl Pts',(-59.2295351930898,-99.4974617351344,
179.985485138407));
#30614=CARTESIAN_POINT('Ctrl Pts',(-57.5720784430859,-99.5798764694207,
179.985485069079));
#30615=CARTESIAN_POINT('Ctrl Pts',(-55.914621693082,-99.662291203707,179.985484999752));
#30616=CARTESIAN_POINT('Ctrl Pts',(-54.7397120431402,-99.6932631932805,
178.813912075476));
#30617=CARTESIAN_POINT('Ctrl Pts',(-53.5648023931984,-99.724235182854,177.6423391512));
#30618=CARTESIAN_POINT('Ctrl Pts',(-53.5548643992186,-99.6310134108495,
175.985484901707));
#30619=CARTESIAN_POINT('Ctrl Pts',(-53.5449264052387,-99.5377916388449,
174.328630652215));
#30620=CARTESIAN_POINT('Ctrl Pts',(-54.6999600268383,-99.3203761095675,
173.157057825983));
#30621=CARTESIAN_POINT('Ctrl Pts',(-55.8549936484379,-99.10296058029,171.985484999752));
#30622=CARTESIAN_POINT('Ctrl Pts',(-57.4925742726078,-98.834102316693,171.985485069079));
#30623=CARTESIAN_POINT('Ctrl Pts',(-59.1301548967777,-98.565244053096,171.985485138407));
#30624=CARTESIAN_POINT('Ctrl Pts',(-60.2851884208854,-98.3478285342118,
173.157058062683));
#30625=CARTESIAN_POINT('Ctrl Pts',(-61.4402219449932,-98.1304130153276,
174.328630986959));
#30626=CARTESIAN_POINT('Ctrl Pts',(-61.430283813139,-98.0371912580215,175.985485236451));
#30627=CARTESIAN_POINT('Ctrl Pts',(-61.4203456812848,-97.9439695007152,
177.642339485944));
#30628=CARTESIAN_POINT('Ctrl Pts',(-60.2454359338512,-97.974941500682,178.813912312176));
#30629=CARTESIAN_POINT('Ctrl Pts',(-59.0705261864175,-98.0059135006488,
179.985485138407));
#30630=CARTESIAN_POINT('Ctrl Pts',(-57.4130694364136,-98.0883282349351,
179.985485069079));
#30631=CARTESIAN_POINT('Ctrl Pts',(-55.7556126864097,-98.1707429692214,
179.985484999752));
#30632=CARTESIAN_POINT('Ctrl Pts',(-54.580703036468,-98.2017149587949,178.813912075476));
#30633=CARTESIAN_POINT('Ctrl Pts',(-61.176587584573,-103.935293252465,178.485485069079));
#30634=CARTESIAN_POINT('Ctrl Pts',(-61.0380153802162,-103.937007770342,
178.657813499464));
#30635=CARTESIAN_POINT('Ctrl Pts',(-60.8814719605401,-103.941134438624,
178.813912312176));
#30636=CARTESIAN_POINT('Ctrl Pts',(-59.7065622131064,-103.972106438591,
179.985485138407));
#30637=CARTESIAN_POINT('Ctrl Pts',(-58.0491054631025,-104.054521172878,
179.985485069079));
#30638=CARTESIAN_POINT('Ctrl Pts',(-56.3916487130987,-104.136935907164,
179.985484999752));
#30639=CARTESIAN_POINT('Ctrl Pts',(-55.2167390631569,-104.167907896737,
178.813912075476));
#30640=CARTESIAN_POINT('Ctrl Pts',(-54.0418294132151,-104.198879886311,
177.6423391512));
#30641=CARTESIAN_POINT('Ctrl Pts',(-54.0318914192353,-104.105658114306,
175.985484901707));
#30642=CARTESIAN_POINT('Ctrl Pts',(-54.0219534252554,-104.012436342302,
174.328630652215));
#30643=CARTESIAN_POINT('Ctrl Pts',(-55.176987046855,-103.795020813024,173.157057825983));
#30644=CARTESIAN_POINT('Ctrl Pts',(-56.3320206684546,-103.577605283747,
171.985484999752));
#30645=CARTESIAN_POINT('Ctrl Pts',(-57.9696012926245,-103.30874702015,171.985485069079));
#30646=CARTESIAN_POINT('Ctrl Pts',(-59.6071819167943,-103.039888756553,
171.985485138407));
#30647=CARTESIAN_POINT('Ctrl Pts',(-60.7622154409021,-102.822473237669,
173.157058062683));
#30648=CARTESIAN_POINT('Ctrl Pts',(-60.9161104618553,-102.793505103726,
173.313156769748));
#30649=CARTESIAN_POINT('Ctrl Pts',(-61.0519296658261,-102.765967674544,
173.485485069079));
#30650=CARTESIAN_POINT('Ctrl Pts',(-56.1707931031902,-113.117197303651,
178.813912075476));
#30651=CARTESIAN_POINT('Ctrl Pts',(-54.9958834532485,-113.148169293224,
177.6423391512));
#30652=CARTESIAN_POINT('Ctrl Pts',(-54.9859454592686,-113.05494752122,175.985484901707));
#30653=CARTESIAN_POINT('Ctrl Pts',(-54.9760074652888,-112.961725749215,
174.328630652215));
#30654=CARTESIAN_POINT('Ctrl Pts',(-56.1310410868884,-112.744310219938,
173.157057825983));
#30655=CARTESIAN_POINT('Ctrl Pts',(-57.286074708488,-112.52689469066,171.985484999752));
#30656=CARTESIAN_POINT('Ctrl Pts',(-58.9236553326578,-112.258036427063,
171.985485069079));
#30657=CARTESIAN_POINT('Ctrl Pts',(-60.5612359568277,-111.989178163466,
171.985485138407));
#30658=CARTESIAN_POINT('Ctrl Pts',(-61.7162694809355,-111.771762644582,
173.157058062683));
#30659=CARTESIAN_POINT('Ctrl Pts',(-62.8713030050432,-111.554347125698,
174.328630986959));
#30660=CARTESIAN_POINT('Ctrl Pts',(-62.861364873189,-111.461125368392,175.985485236451));
#30661=CARTESIAN_POINT('Ctrl Pts',(-62.8514267413349,-111.367903611086,
177.642339485944));
#30662=CARTESIAN_POINT('Ctrl Pts',(-61.6765169939012,-111.398875611052,
178.813912312176));
#30663=CARTESIAN_POINT('Ctrl Pts',(-60.5016072464676,-111.429847611019,
179.985485138407));
#30664=CARTESIAN_POINT('Ctrl Pts',(-58.8441504964637,-111.512262345305,
179.985485069079));
#30665=CARTESIAN_POINT('Ctrl Pts',(-57.1866937464598,-111.594677079592,
179.985484999752));
#30666=CARTESIAN_POINT('Ctrl Pts',(-56.011784096518,-111.625649069165,178.813912075476));
#30667=CARTESIAN_POINT('Ctrl Pts',(-54.8368744465763,-111.656621058739,
177.6423391512));
#30668=CARTESIAN_POINT('Ctrl Pts',(-54.8269364525964,-111.563399286734,
175.985484901707));
#30669=CARTESIAN_POINT('Ctrl Pts',(-54.8169984586165,-111.47017751473,174.328630652215));
#30670=CARTESIAN_POINT('Ctrl Pts',(-55.9720320802161,-111.252761985452,
173.157057825983));
#30671=CARTESIAN_POINT('Ctrl Pts',(-57.1270657018158,-111.035346456175,
171.985484999752));
#30672=CARTESIAN_POINT('Ctrl Pts',(-58.7646463259856,-110.766488192578,
171.985485069079));
#30673=CARTESIAN_POINT('Ctrl Pts',(-60.4022269501555,-110.497629928981,
171.985485138407));
#30674=CARTESIAN_POINT('Ctrl Pts',(-61.5572604742632,-110.280214410097,
173.157058062683));
#30675=CARTESIAN_POINT('Ctrl Pts',(-62.712293998371,-110.062798891212,174.328630986959));
#30676=CARTESIAN_POINT('Ctrl Pts',(-62.7023558665168,-109.969577133906,
175.985485236451));
#30677=CARTESIAN_POINT('Ctrl Pts',(-62.6924177346626,-109.8763553766,177.642339485944));
#30678=CARTESIAN_POINT('Ctrl Pts',(-61.517507987229,-109.907327376567,178.813912312176));
#30679=CARTESIAN_POINT('Ctrl Pts',(-60.3425982397954,-109.938299376534,
179.985485138407));
#30680=CARTESIAN_POINT('Ctrl Pts',(-58.6851414897915,-110.02071411082,179.985485069079));
#30681=CARTESIAN_POINT('Ctrl Pts',(-57.0276847397876,-110.103128845106,
179.985484999752));
#30682=CARTESIAN_POINT('Ctrl Pts',(-55.8527750898458,-110.13410083468,178.813912075476));
#30683=CARTESIAN_POINT('Ctrl Pts',(-54.677865439904,-110.165072824253,177.6423391512));
#30684=CARTESIAN_POINT('Ctrl Pts',(-54.6679274459242,-110.071851052249,
175.985484901707));
#30685=CARTESIAN_POINT('Ctrl Pts',(-54.6579894519443,-109.978629280244,
174.328630652215));
#30686=CARTESIAN_POINT('Ctrl Pts',(-55.8130230735439,-109.761213750967,
173.157057825983));
#30687=CARTESIAN_POINT('Ctrl Pts',(-56.9680566951435,-109.543798221689,
171.985484999752));
#30688=CARTESIAN_POINT('Ctrl Pts',(-58.6056373193134,-109.274939958092,
171.985485069079));
#30689=CARTESIAN_POINT('Ctrl Pts',(-60.2432179434833,-109.006081694495,
171.985485138407));
#30690=CARTESIAN_POINT('Ctrl Pts',(-61.398251467591,-108.788666175611,173.157058062683));
#30691=CARTESIAN_POINT('Ctrl Pts',(-62.5532849916988,-108.571250656727,
174.328630986959));
#30692=CARTESIAN_POINT('Ctrl Pts',(-62.5433468598446,-108.478028899421,
175.985485236451));
#30693=CARTESIAN_POINT('Ctrl Pts',(-62.5334087279904,-108.384807142114,
177.642339485944));
#30694=CARTESIAN_POINT('Ctrl Pts',(-61.3584989805568,-108.415779142081,
178.813912312176));
#30695=CARTESIAN_POINT('Ctrl Pts',(-60.1835892331231,-108.446751142048,
179.985485138407));
#30696=CARTESIAN_POINT('Ctrl Pts',(-58.5261324831192,-108.529165876334,
179.985485069079));
#30697=CARTESIAN_POINT('Ctrl Pts',(-56.8686757331153,-108.611580610621,
179.985484999752));
#30698=CARTESIAN_POINT('Ctrl Pts',(-55.6937660831736,-108.642552600194,
178.813912075476));
#30699=CARTESIAN_POINT('Ctrl Pts',(-54.5188564332318,-108.673524589768,
177.6423391512));
#30700=CARTESIAN_POINT('Ctrl Pts',(-54.5089184392519,-108.580302817763,
175.985484901707));
#30701=CARTESIAN_POINT('Ctrl Pts',(-54.4989804452721,-108.487081045759,
174.328630652215));
#30702=CARTESIAN_POINT('Ctrl Pts',(-55.6540140668717,-108.269665516481,
173.157057825983));
#30703=CARTESIAN_POINT('Ctrl Pts',(-56.8090476884713,-108.052249987204,
171.985484999752));
#30704=CARTESIAN_POINT('Ctrl Pts',(-58.4466283126412,-107.783391723607,
171.985485069079));
#30705=CARTESIAN_POINT('Ctrl Pts',(-60.084208936811,-107.51453346001,171.985485138407));
#30706=CARTESIAN_POINT('Ctrl Pts',(-61.2392424609188,-107.297117941125,
173.157058062683));
#30707=CARTESIAN_POINT('Ctrl Pts',(-62.3942759850265,-107.079702422241,
174.328630986959));
#30708=CARTESIAN_POINT('Ctrl Pts',(-62.3843378531723,-106.986480664935,
175.985485236451));
#30709=CARTESIAN_POINT('Ctrl Pts',(-62.3743997213182,-106.893258907629,
177.642339485944));
#30710=CARTESIAN_POINT('Ctrl Pts',(-61.1994899738845,-106.924230907596,
178.813912312176));
#30711=CARTESIAN_POINT('Ctrl Pts',(-60.0245802264509,-106.955202907562,
179.985485138407));
#30712=CARTESIAN_POINT('Ctrl Pts',(-58.367123476447,-107.037617641849,179.985485069079));
#30713=CARTESIAN_POINT('Ctrl Pts',(-56.7096667264431,-107.120032376135,
179.985484999752));
#30714=CARTESIAN_POINT('Ctrl Pts',(-55.5347570765013,-107.151004365708,
178.813912075476));
#30715=CARTESIAN_POINT('Ctrl Pts',(-54.3598474265596,-107.181976355282,
177.6423391512));
#30716=CARTESIAN_POINT('Ctrl Pts',(-54.3499094325797,-107.088754583277,
175.985484901707));
#30717=CARTESIAN_POINT('Ctrl Pts',(-54.3399714385998,-106.995532811273,
174.328630652215));
#30718=CARTESIAN_POINT('Ctrl Pts',(-55.4950050601995,-106.778117281995,
173.157057825983));
#30719=CARTESIAN_POINT('Ctrl Pts',(-56.6500386817991,-106.560701752718,
171.985484999752));
#30720=CARTESIAN_POINT('Ctrl Pts',(-58.2876193059689,-106.291843489121,
171.985485069079));
#30721=CARTESIAN_POINT('Ctrl Pts',(-59.9251999301388,-106.022985225524,
171.985485138407));
#30722=CARTESIAN_POINT('Ctrl Pts',(-61.0802334542465,-105.80556970664,173.157058062683));
#30723=CARTESIAN_POINT('Ctrl Pts',(-62.2352669783543,-105.588154187756,
174.328630986959));
#30724=CARTESIAN_POINT('Ctrl Pts',(-62.2253288465001,-105.494932430449,
175.985485236451));
#30725=CARTESIAN_POINT('Ctrl Pts',(-62.2153907146459,-105.401710673143,
177.642339485944));
#30726=CARTESIAN_POINT('Ctrl Pts',(-61.0404809672123,-105.43268267311,178.813912312176));
#30727=CARTESIAN_POINT('Ctrl Pts',(-59.8655712197787,-105.463654673077,
179.985485138407));
#30728=CARTESIAN_POINT('Ctrl Pts',(-58.2081144697748,-105.546069407363,
179.985485069079));
#30729=CARTESIAN_POINT('Ctrl Pts',(-56.5506577197709,-105.628484141649,
179.985484999752));
#30730=CARTESIAN_POINT('Ctrl Pts',(-55.3757480698291,-105.659456131223,
178.813912075476));
#30731=CARTESIAN_POINT('Ctrl Pts',(-54.2008384198873,-105.690428120796,
177.6423391512));
#30732=CARTESIAN_POINT('Ctrl Pts',(-54.1909004259075,-105.597206348792,
175.985484901707));
#30733=CARTESIAN_POINT('Ctrl Pts',(-54.1809624319276,-105.503984576787,
174.328630652215));
#30734=CARTESIAN_POINT('Ctrl Pts',(-55.3359960535272,-105.28656904751,173.157057825983));
#30735=CARTESIAN_POINT('Ctrl Pts',(-56.4910296751268,-105.069153518232,
171.985484999752));
#30736=CARTESIAN_POINT('Ctrl Pts',(-58.1286102992967,-104.800295254635,
171.985485069079));
#30737=CARTESIAN_POINT('Ctrl Pts',(-59.7661909234666,-104.531436991038,
171.985485138407));
#30738=CARTESIAN_POINT('Ctrl Pts',(-60.9212244475743,-104.314021472154,
173.157058062683));
#30739=CARTESIAN_POINT('Ctrl Pts',(-62.0762579716821,-104.09660595327,174.328630986959));
#30740=CARTESIAN_POINT('Ctrl Pts',(-62.0663198398279,-104.003384195964,
175.985485236451));
#30741=CARTESIAN_POINT('Ctrl Pts',(-62.0563817079737,-103.910162438658,
177.642339485944));
#30742=CARTESIAN_POINT('Ctrl Pts',(-60.8814719605401,-103.941134438624,
178.813912312176));
#30743=CARTESIAN_POINT('Ctrl Pts',(-59.7065622131064,-103.972106438591,
179.985485138407));
#30744=CARTESIAN_POINT('Ctrl Pts',(-58.0491054631025,-104.054521172878,
179.985485069079));
#30745=CARTESIAN_POINT('Ctrl Pts',(-56.3916487130987,-104.136935907164,
179.985484999752));
#30746=CARTESIAN_POINT('Ctrl Pts',(-55.2167390631569,-104.167907896737,
178.813912075476));
#30747=CARTESIAN_POINT('Ctrl Pts',(-54.0418294132151,-104.198879886311,
177.6423391512));
#30748=CARTESIAN_POINT('Ctrl Pts',(-54.0318914192353,-104.105658114306,
175.985484901707));
#30749=CARTESIAN_POINT('Ctrl Pts',(-54.0219534252554,-104.012436342302,
174.328630652215));
#30750=CARTESIAN_POINT('Ctrl Pts',(-55.176987046855,-103.795020813024,173.157057825983));
#30751=CARTESIAN_POINT('Ctrl Pts',(-56.3320206684546,-103.577605283747,
171.985484999752));
#30752=CARTESIAN_POINT('Ctrl Pts',(-57.9696012926245,-103.30874702015,171.985485069079));
#30753=CARTESIAN_POINT('Ctrl Pts',(-59.6071819167943,-103.039888756553,
171.985485138407));
#30754=CARTESIAN_POINT('Ctrl Pts',(-60.7622154409021,-102.822473237669,
173.157058062683));
#30755=CARTESIAN_POINT('Ctrl Pts',(-61.9172489650099,-102.605057718784,
174.328630986959));
#30756=CARTESIAN_POINT('Ctrl Pts',(-61.9073108331557,-102.511835961478,
175.985485236451));
#30757=CARTESIAN_POINT('Ctrl Pts',(-61.8973727013015,-102.418614204172,
177.642339485944));
#30758=CARTESIAN_POINT('Ctrl Pts',(-60.7224629538678,-102.449586204139,
178.813912312176));
#30759=CARTESIAN_POINT('Ctrl Pts',(-59.5475532064342,-102.480558204106,
179.985485138407));
#30760=CARTESIAN_POINT('Ctrl Pts',(-57.8900964564303,-102.562972938392,
179.985485069079));
#30761=CARTESIAN_POINT('Ctrl Pts',(-56.2326397064264,-102.645387672678,
179.985484999752));
#30762=CARTESIAN_POINT('Ctrl Pts',(-55.0577300564847,-102.676359662252,
178.813912075476));
#30763=CARTESIAN_POINT('Ctrl Pts',(-53.8828204065429,-102.707331651825,
177.6423391512));
#30764=CARTESIAN_POINT('Ctrl Pts',(-53.872882412563,-102.614109879821,175.985484901707));
#30765=CARTESIAN_POINT('Ctrl Pts',(-53.8629444185832,-102.520888107816,
174.328630652215));
#30766=CARTESIAN_POINT('Ctrl Pts',(-55.0179780401828,-102.303472578539,
173.157057825983));
#30767=CARTESIAN_POINT('Ctrl Pts',(-56.1730116617824,-102.086057049261,
171.985484999752));
#30768=CARTESIAN_POINT('Ctrl Pts',(-57.8105922859523,-101.817198785664,
171.985485069079));
#30769=CARTESIAN_POINT('Ctrl Pts',(-59.4481729101221,-101.548340522067,
171.985485138407));
#30770=CARTESIAN_POINT('Ctrl Pts',(-60.6032064342299,-101.330925003183,
173.157058062683));
#30771=CARTESIAN_POINT('Ctrl Pts',(-61.7582399583376,-101.113509484299,
174.328630986959));
#30772=CARTESIAN_POINT('Ctrl Pts',(-61.7483018264834,-101.020287726993,
175.985485236451));
#30773=CARTESIAN_POINT('Ctrl Pts',(-61.7383636946293,-100.927065969686,
177.642339485944));
#30774=CARTESIAN_POINT('Ctrl Pts',(-60.5634539471956,-100.958037969653,
178.813912312176));
#30775=CARTESIAN_POINT('Ctrl Pts',(-59.388544199762,-100.98900996962,179.985485138407));
#30776=CARTESIAN_POINT('Ctrl Pts',(-57.7310874497581,-101.071424703906,
179.985485069079));
#30777=CARTESIAN_POINT('Ctrl Pts',(-56.0736306997542,-101.153839438193,
179.985484999752));
#30778=CARTESIAN_POINT('Ctrl Pts',(-54.8987210498124,-101.184811427766,
178.813912075476));
#30779=CARTESIAN_POINT('Ctrl Pts',(-53.7238113998707,-101.21578341734,177.6423391512));
#30780=CARTESIAN_POINT('Ctrl Pts',(-53.7138734058908,-101.122561645335,
175.985484901707));
#30781=CARTESIAN_POINT('Ctrl Pts',(-53.7039354119109,-101.029339873331,
174.328630652215));
#30782=CARTESIAN_POINT('Ctrl Pts',(-54.8589690335105,-100.811924344053,
173.157057825983));
#30783=CARTESIAN_POINT('Ctrl Pts',(-56.0140026551102,-100.594508814776,
171.985484999752));
#30784=CARTESIAN_POINT('Ctrl Pts',(-57.65158327928,-100.325650551179,171.985485069079));
#30785=CARTESIAN_POINT('Ctrl Pts',(-59.2891639034499,-100.056792287582,
171.985485138407));
#30786=CARTESIAN_POINT('Ctrl Pts',(-60.4441974275576,-99.8393767686974,
173.157058062683));
#30787=CARTESIAN_POINT('Ctrl Pts',(-61.5992309516654,-99.6219612498133,
174.328630986959));
#30788=CARTESIAN_POINT('Ctrl Pts',(-61.5892928198112,-99.528739492507,175.985485236451));
#30789=CARTESIAN_POINT('Ctrl Pts',(-61.579354687957,-99.4355177352008,177.642339485944));
#30790=CARTESIAN_POINT('Ctrl Pts',(-60.4044449405234,-99.4664897351676,
178.813912312176));
#30791=CARTESIAN_POINT('Ctrl Pts',(-59.2295351930898,-99.4974617351344,
179.985485138407));
#30792=CARTESIAN_POINT('Ctrl Pts',(-57.5720784430859,-99.5798764694207,
179.985485069079));
#30793=CARTESIAN_POINT('Ctrl Pts',(-55.914621693082,-99.662291203707,179.985484999752));
#30794=CARTESIAN_POINT('Ctrl Pts',(-54.7397120431402,-99.6932631932805,
178.813912075476));
#30795=CARTESIAN_POINT('Ctrl Pts',(-53.5648023931984,-99.724235182854,177.6423391512));
#30796=CARTESIAN_POINT('Ctrl Pts',(-53.5548643992186,-99.6310134108495,
175.985484901707));
#30797=CARTESIAN_POINT('Ctrl Pts',(-53.5449264052387,-99.5377916388449,
174.328630652215));
#30798=CARTESIAN_POINT('Ctrl Pts',(-54.6999600268383,-99.3203761095675,
173.157057825983));
#30799=CARTESIAN_POINT('Ctrl Pts',(-55.8549936484379,-99.10296058029,171.985484999752));
#30800=CARTESIAN_POINT('Ctrl Pts',(-57.4925742726078,-98.834102316693,171.985485069079));
#30801=CARTESIAN_POINT('Ctrl Pts',(-59.1301548967777,-98.5652440530961,
171.985485138407));
#30802=CARTESIAN_POINT('Ctrl Pts',(-60.2851884208854,-98.3478285342118,
173.157058062683));
#30803=CARTESIAN_POINT('Ctrl Pts',(-61.4402219449932,-98.1304130153276,
174.328630986959));
#30804=CARTESIAN_POINT('Ctrl Pts',(-61.430283813139,-98.0371912580215,175.985485236451));
#30805=CARTESIAN_POINT('Ctrl Pts',(-61.4203456812848,-97.9439695007152,
177.642339485944));
#30806=CARTESIAN_POINT('Ctrl Pts',(-60.2454359338512,-97.974941500682,178.813912312176));
#30807=CARTESIAN_POINT('Ctrl Pts',(-59.0705261864175,-98.0059135006488,
179.985485138407));
#30808=CARTESIAN_POINT('Ctrl Pts',(-57.4130694364136,-98.0883282349351,
179.985485069079));
#30809=CARTESIAN_POINT('Ctrl Pts',(-55.7556126864097,-98.1707429692214,
179.985484999752));
#30810=CARTESIAN_POINT('Ctrl Pts',(-54.580703036468,-98.2017149587949,178.813912075476));
#30811=CARTESIAN_POINT('Ctrl Pts',(-56.181115489574,-113.283598570176,178.821287383467));
#30812=CARTESIAN_POINT('Ctrl Pts',(-55.0031681001975,-113.314894403068,
177.646659506339));
#30813=CARTESIAN_POINT('Ctrl Pts',(-54.9932301063974,-113.221672631044,
175.985484901271));
#30814=CARTESIAN_POINT('Ctrl Pts',(-54.9832921125973,-113.12845085902,174.324310296203));
#30815=CARTESIAN_POINT('Ctrl Pts',(-56.1413634738858,-112.910711486397,
173.149682517375));
#30816=CARTESIAN_POINT('Ctrl Pts',(-57.2994348351743,-112.692972113774,
171.975054738546));
#30817=CARTESIAN_POINT('Ctrl Pts',(-58.9413114718314,-112.423655866545,
171.975054808055));
#30818=CARTESIAN_POINT('Ctrl Pts',(-60.5831881084886,-112.154339619316,
171.975054877564));
#30819=CARTESIAN_POINT('Ctrl Pts',(-61.741259372031,-111.936600257113,173.149682754692));
#30820=CARTESIAN_POINT('Ctrl Pts',(-62.8993306355734,-111.71886089491,174.32431063182));
#30821=CARTESIAN_POINT('Ctrl Pts',(-62.8893925035395,-111.625639137623,
175.985485236888));
#30822=CARTESIAN_POINT('Ctrl Pts',(-62.8794543715055,-111.532417380336,
177.646659841956));
#30823=CARTESIAN_POINT('Ctrl Pts',(-61.701506884383,-111.563713223648,178.821287620784));
#30824=CARTESIAN_POINT('Ctrl Pts',(-60.5235593972605,-111.595009066961,
179.995915399612));
#30825=CARTESIAN_POINT('Ctrl Pts',(-58.8618066347693,-111.677881784879,
179.995915330104));
#30826=CARTESIAN_POINT('Ctrl Pts',(-57.2000538722782,-111.760754502798,
179.995915260595));
#30827=CARTESIAN_POINT('Ctrl Pts',(-56.0221064829017,-111.79205033569,178.821287383467));
#30828=CARTESIAN_POINT('Ctrl Pts',(-54.8441590935253,-111.823346168582,
177.646659506339));
#30829=CARTESIAN_POINT('Ctrl Pts',(-54.8342210997252,-111.730124396559,
175.985484901271));
#30830=CARTESIAN_POINT('Ctrl Pts',(-54.8242831059251,-111.636902624535,
174.324310296203));
#30831=CARTESIAN_POINT('Ctrl Pts',(-55.9823544672136,-111.419163251912,
173.149682517375));
#30832=CARTESIAN_POINT('Ctrl Pts',(-57.1404258285021,-111.201423879289,
171.975054738546));
#30833=CARTESIAN_POINT('Ctrl Pts',(-58.7823024651592,-110.932107632059,
171.975054808055));
#30834=CARTESIAN_POINT('Ctrl Pts',(-60.4241791018163,-110.66279138483,171.975054877564));
#30835=CARTESIAN_POINT('Ctrl Pts',(-61.5822503653587,-110.445052022627,
173.149682754692));
#30836=CARTESIAN_POINT('Ctrl Pts',(-62.7403216289012,-110.227312660424,
174.32431063182));
#30837=CARTESIAN_POINT('Ctrl Pts',(-62.7303834968672,-110.134090903137,
175.985485236888));
#30838=CARTESIAN_POINT('Ctrl Pts',(-62.7204453648333,-110.04086914585,177.646659841956));
#30839=CARTESIAN_POINT('Ctrl Pts',(-61.5424978777108,-110.072164989163,
178.821287620784));
#30840=CARTESIAN_POINT('Ctrl Pts',(-60.3645503905882,-110.103460832475,
179.995915399612));
#30841=CARTESIAN_POINT('Ctrl Pts',(-58.7027976280971,-110.186333550394,
179.995915330104));
#30842=CARTESIAN_POINT('Ctrl Pts',(-57.041044865606,-110.269206268313,179.995915260595));
#30843=CARTESIAN_POINT('Ctrl Pts',(-55.8630974762295,-110.300502101205,
178.821287383467));
#30844=CARTESIAN_POINT('Ctrl Pts',(-54.6851500868531,-110.331797934097,
177.646659506339));
#30845=CARTESIAN_POINT('Ctrl Pts',(-54.675212093053,-110.238576162073,175.985484901271));
#30846=CARTESIAN_POINT('Ctrl Pts',(-54.6652740992529,-110.145354390049,
174.324310296203));
#30847=CARTESIAN_POINT('Ctrl Pts',(-55.8233454605414,-109.927615017426,
173.149682517375));
#30848=CARTESIAN_POINT('Ctrl Pts',(-56.9814168218299,-109.709875644803,
171.975054738546));
#30849=CARTESIAN_POINT('Ctrl Pts',(-58.623293458487,-109.440559397574,171.975054808055));
#30850=CARTESIAN_POINT('Ctrl Pts',(-60.2651700951441,-109.171243150344,
171.975054877564));
#30851=CARTESIAN_POINT('Ctrl Pts',(-61.4232413586865,-108.953503788142,
173.149682754692));
#30852=CARTESIAN_POINT('Ctrl Pts',(-62.581312622229,-108.735764425939,174.32431063182));
#30853=CARTESIAN_POINT('Ctrl Pts',(-62.571374490195,-108.642542668652,175.985485236888));
#30854=CARTESIAN_POINT('Ctrl Pts',(-62.5614363581611,-108.549320911365,
177.646659841956));
#30855=CARTESIAN_POINT('Ctrl Pts',(-61.3834888710385,-108.580616754677,
178.821287620784));
#30856=CARTESIAN_POINT('Ctrl Pts',(-60.205541383916,-108.61191259799,179.995915399612));
#30857=CARTESIAN_POINT('Ctrl Pts',(-58.5437886214249,-108.694785315908,
179.995915330104));
#30858=CARTESIAN_POINT('Ctrl Pts',(-56.8820358589338,-108.777658033827,
179.995915260595));
#30859=CARTESIAN_POINT('Ctrl Pts',(-55.7040884695573,-108.808953866719,
178.821287383467));
#30860=CARTESIAN_POINT('Ctrl Pts',(-54.5261410801808,-108.840249699611,
177.646659506339));
#30861=CARTESIAN_POINT('Ctrl Pts',(-54.5162030863807,-108.747027927587,
175.985484901271));
#30862=CARTESIAN_POINT('Ctrl Pts',(-54.5062650925806,-108.653806155564,
174.324310296203));
#30863=CARTESIAN_POINT('Ctrl Pts',(-55.6643364538691,-108.436066782941,
173.149682517375));
#30864=CARTESIAN_POINT('Ctrl Pts',(-56.8224078151577,-108.218327410317,
171.975054738546));
#30865=CARTESIAN_POINT('Ctrl Pts',(-58.4642844518147,-107.949011163088,
171.975054808055));
#30866=CARTESIAN_POINT('Ctrl Pts',(-60.1061610884719,-107.679694915859,
171.975054877564));
#30867=CARTESIAN_POINT('Ctrl Pts',(-61.2642323520143,-107.461955553656,
173.149682754692));
#30868=CARTESIAN_POINT('Ctrl Pts',(-62.4223036155567,-107.244216191453,
174.32431063182));
#30869=CARTESIAN_POINT('Ctrl Pts',(-62.4123654835228,-107.150994434166,
175.985485236888));
#30870=CARTESIAN_POINT('Ctrl Pts',(-62.4024273514889,-107.057772676879,
177.646659841956));
#30871=CARTESIAN_POINT('Ctrl Pts',(-61.2244798643663,-107.089068520192,
178.821287620784));
#30872=CARTESIAN_POINT('Ctrl Pts',(-60.0465323772438,-107.120364363504,
179.995915399612));
#30873=CARTESIAN_POINT('Ctrl Pts',(-58.3847796147526,-107.203237081423,
179.995915330104));
#30874=CARTESIAN_POINT('Ctrl Pts',(-56.7230268522615,-107.286109799341,
179.995915260595));
#30875=CARTESIAN_POINT('Ctrl Pts',(-55.5450794628851,-107.317405632233,
178.821287383467));
#30876=CARTESIAN_POINT('Ctrl Pts',(-54.3671320735086,-107.348701465125,
177.646659506339));
#30877=CARTESIAN_POINT('Ctrl Pts',(-54.3571940797085,-107.255479693102,
175.985484901271));
#30878=CARTESIAN_POINT('Ctrl Pts',(-54.3472560859084,-107.162257921078,
174.324310296203));
#30879=CARTESIAN_POINT('Ctrl Pts',(-55.5053274471969,-106.944518548455,
173.149682517375));
#30880=CARTESIAN_POINT('Ctrl Pts',(-56.6633988084854,-106.726779175832,
171.975054738546));
#30881=CARTESIAN_POINT('Ctrl Pts',(-58.3052754451425,-106.457462928602,
171.975054808055));
#30882=CARTESIAN_POINT('Ctrl Pts',(-59.9471520817997,-106.188146681373,
171.975054877564));
#30883=CARTESIAN_POINT('Ctrl Pts',(-61.1052233453421,-105.97040731917,173.149682754692));
#30884=CARTESIAN_POINT('Ctrl Pts',(-62.2632946088845,-105.752667956968,
174.32431063182));
#30885=CARTESIAN_POINT('Ctrl Pts',(-62.2533564768505,-105.659446199681,
175.985485236888));
#30886=CARTESIAN_POINT('Ctrl Pts',(-62.2434183448166,-105.566224442394,
177.646659841956));
#30887=CARTESIAN_POINT('Ctrl Pts',(-61.0654708576941,-105.597520285706,
178.821287620784));
#30888=CARTESIAN_POINT('Ctrl Pts',(-59.8875233705716,-105.628816129018,
179.995915399612));
#30889=CARTESIAN_POINT('Ctrl Pts',(-58.2257706080804,-105.711688846937,
179.995915330104));
#30890=CARTESIAN_POINT('Ctrl Pts',(-56.5640178455893,-105.794561564856,
179.995915260595));
#30891=CARTESIAN_POINT('Ctrl Pts',(-55.3860704562128,-105.825857397748,
178.821287383467));
#30892=CARTESIAN_POINT('Ctrl Pts',(-54.2081230668364,-105.85715323064,177.646659506339));
#30893=CARTESIAN_POINT('Ctrl Pts',(-54.1981850730363,-105.763931458616,
175.985484901271));
#30894=CARTESIAN_POINT('Ctrl Pts',(-54.1882470792362,-105.670709686593,
174.324310296203));
#30895=CARTESIAN_POINT('Ctrl Pts',(-55.3463184405247,-105.452970313969,
173.149682517375));
#30896=CARTESIAN_POINT('Ctrl Pts',(-56.5043898018132,-105.235230941346,
171.975054738546));
#30897=CARTESIAN_POINT('Ctrl Pts',(-58.1462664384703,-104.965914694117,
171.975054808055));
#30898=CARTESIAN_POINT('Ctrl Pts',(-59.7881430751274,-104.696598446888,
171.975054877564));
#30899=CARTESIAN_POINT('Ctrl Pts',(-60.9462143386698,-104.478859084685,
173.149682754692));
#30900=CARTESIAN_POINT('Ctrl Pts',(-62.1042856022123,-104.261119722482,
174.32431063182));
#30901=CARTESIAN_POINT('Ctrl Pts',(-62.0943474701783,-104.167897965195,
175.985485236888));
#30902=CARTESIAN_POINT('Ctrl Pts',(-62.0844093381444,-104.074676207908,
177.646659841956));
#30903=CARTESIAN_POINT('Ctrl Pts',(-60.9064618510219,-104.10597205122,178.821287620784));
#30904=CARTESIAN_POINT('Ctrl Pts',(-59.7285143638993,-104.137267894533,
179.995915399612));
#30905=CARTESIAN_POINT('Ctrl Pts',(-58.0667616014082,-104.220140612451,
179.995915330104));
#30906=CARTESIAN_POINT('Ctrl Pts',(-56.4050088389171,-104.30301333037,179.995915260595));
#30907=CARTESIAN_POINT('Ctrl Pts',(-55.2270614495406,-104.334309163262,
178.821287383467));
#30908=CARTESIAN_POINT('Ctrl Pts',(-54.0491140601642,-104.365604996154,
177.646659506339));
#30909=CARTESIAN_POINT('Ctrl Pts',(-54.039176066364,-104.272383224131,175.985484901271));
#30910=CARTESIAN_POINT('Ctrl Pts',(-54.029238072564,-104.179161452107,174.324310296203));
#30911=CARTESIAN_POINT('Ctrl Pts',(-55.1873094338524,-103.961422079484,
173.149682517375));
#30912=CARTESIAN_POINT('Ctrl Pts',(-56.345380795141,-103.743682706861,171.975054738546));
#30913=CARTESIAN_POINT('Ctrl Pts',(-57.9872574317981,-103.474366459631,
171.975054808055));
#30914=CARTESIAN_POINT('Ctrl Pts',(-59.6291340684552,-103.205050212402,
171.975054877564));
#30915=CARTESIAN_POINT('Ctrl Pts',(-60.7872053319976,-102.987310850199,
173.149682754692));
#30916=CARTESIAN_POINT('Ctrl Pts',(-61.94527659554,-102.769571487996,174.32431063182));
#30917=CARTESIAN_POINT('Ctrl Pts',(-61.9353384635061,-102.676349730709,
175.985485236888));
#30918=CARTESIAN_POINT('Ctrl Pts',(-61.9254003314722,-102.583127973422,
177.646659841956));
#30919=CARTESIAN_POINT('Ctrl Pts',(-60.7474528443496,-102.614423816735,
178.821287620784));
#30920=CARTESIAN_POINT('Ctrl Pts',(-59.5695053572271,-102.645719660047,
179.995915399612));
#30921=CARTESIAN_POINT('Ctrl Pts',(-57.907752594736,-102.728592377966,179.995915330104));
#30922=CARTESIAN_POINT('Ctrl Pts',(-56.2459998322448,-102.811465095885,
179.995915260595));
#30923=CARTESIAN_POINT('Ctrl Pts',(-55.0680524428684,-102.842760928777,
178.821287383467));
#30924=CARTESIAN_POINT('Ctrl Pts',(-53.8901050534919,-102.874056761669,
177.646659506339));
#30925=CARTESIAN_POINT('Ctrl Pts',(-53.8801670596918,-102.780834989645,
175.985484901271));
#30926=CARTESIAN_POINT('Ctrl Pts',(-53.8702290658917,-102.687613217621,
174.324310296203));
#30927=CARTESIAN_POINT('Ctrl Pts',(-55.0283004271802,-102.469873844998,
173.149682517375));
#30928=CARTESIAN_POINT('Ctrl Pts',(-56.1863717884687,-102.252134472375,
171.975054738546));
#30929=CARTESIAN_POINT('Ctrl Pts',(-57.8282484251258,-101.982818225146,
171.975054808055));
#30930=CARTESIAN_POINT('Ctrl Pts',(-59.470125061783,-101.713501977916,171.975054877564));
#30931=CARTESIAN_POINT('Ctrl Pts',(-60.6281963253254,-101.495762615714,
173.149682754692));
#30932=CARTESIAN_POINT('Ctrl Pts',(-61.7862675888678,-101.278023253511,
174.32431063182));
#30933=CARTESIAN_POINT('Ctrl Pts',(-61.7763294568339,-101.184801496224,
175.985485236888));
#30934=CARTESIAN_POINT('Ctrl Pts',(-61.7663913247999,-101.091579738937,
177.646659841956));
#30935=CARTESIAN_POINT('Ctrl Pts',(-60.5884438376774,-101.122875582249,
178.821287620784));
#30936=CARTESIAN_POINT('Ctrl Pts',(-59.4104963505549,-101.154171425562,
179.995915399612));
#30937=CARTESIAN_POINT('Ctrl Pts',(-57.7487435880637,-101.23704414348,179.995915330104));
#30938=CARTESIAN_POINT('Ctrl Pts',(-56.0869908255726,-101.319916861399,
179.995915260595));
#30939=CARTESIAN_POINT('Ctrl Pts',(-54.9090434361961,-101.351212694291,
178.821287383467));
#30940=CARTESIAN_POINT('Ctrl Pts',(-53.7310960468197,-101.382508527183,
177.646659506339));
#30941=CARTESIAN_POINT('Ctrl Pts',(-53.7211580530196,-101.289286755159,
175.985484901271));
#30942=CARTESIAN_POINT('Ctrl Pts',(-53.7112200592195,-101.196064983136,
174.324310296203));
#30943=CARTESIAN_POINT('Ctrl Pts',(-54.869291420508,-100.978325610513,173.149682517375));
#30944=CARTESIAN_POINT('Ctrl Pts',(-56.0273627817965,-100.760586237889,
171.975054738546));
#30945=CARTESIAN_POINT('Ctrl Pts',(-57.6692394184536,-100.49126999066,171.975054808055));
#30946=CARTESIAN_POINT('Ctrl Pts',(-59.3111160551107,-100.221953743431,
171.975054877564));
#30947=CARTESIAN_POINT('Ctrl Pts',(-60.4691873186531,-100.004214381228,
173.149682754692));
#30948=CARTESIAN_POINT('Ctrl Pts',(-61.6272585821956,-99.7864750190253,
174.32431063182));
#30949=CARTESIAN_POINT('Ctrl Pts',(-61.6173204501616,-99.6932532617382,
175.985485236888));
#30950=CARTESIAN_POINT('Ctrl Pts',(-61.6073823181277,-99.6000315044512,
177.646659841956));
#30951=CARTESIAN_POINT('Ctrl Pts',(-60.4294348310052,-99.6313273477637,
178.821287620784));
#30952=CARTESIAN_POINT('Ctrl Pts',(-59.2514873438827,-99.6626231910761,
179.995915399612));
#30953=CARTESIAN_POINT('Ctrl Pts',(-57.5897345813915,-99.7454959089947,
179.995915330104));
#30954=CARTESIAN_POINT('Ctrl Pts',(-55.9279818189004,-99.8283686269133,
179.995915260595));
#30955=CARTESIAN_POINT('Ctrl Pts',(-54.7500344295239,-99.8596644598054,
178.821287383467));
#30956=CARTESIAN_POINT('Ctrl Pts',(-53.5720870401475,-99.8909602926975,
177.646659506339));
#30957=CARTESIAN_POINT('Ctrl Pts',(-53.5621490463474,-99.7977385206737,
175.985484901271));
#30958=CARTESIAN_POINT('Ctrl Pts',(-53.5522110525473,-99.7045167486501,
174.324310296203));
#30959=CARTESIAN_POINT('Ctrl Pts',(-54.7102824138358,-99.4867773760269,
173.149682517375));
#30960=CARTESIAN_POINT('Ctrl Pts',(-55.8683537751243,-99.2690380034038,
171.975054738546));
#30961=CARTESIAN_POINT('Ctrl Pts',(-57.5102304117814,-98.9997217561745,
171.975054808055));
#30962=CARTESIAN_POINT('Ctrl Pts',(-59.1521070484385,-98.7304055089452,
171.975054877564));
#30963=CARTESIAN_POINT('Ctrl Pts',(-60.3101783119809,-98.5126661467424,
173.149682754692));
#30964=CARTESIAN_POINT('Ctrl Pts',(-61.4682495755234,-98.2949267845397,
174.32431063182));
#30965=CARTESIAN_POINT('Ctrl Pts',(-61.4583114434894,-98.2017050272526,
175.985485236888));
#30966=CARTESIAN_POINT('Ctrl Pts',(-61.4483733114555,-98.1084832699656,
177.646659841956));
#30967=CARTESIAN_POINT('Ctrl Pts',(-60.2704258243329,-98.139779113278,178.821287620784));
#30968=CARTESIAN_POINT('Ctrl Pts',(-59.0924783372104,-98.1710749565905,
179.995915399612));
#30969=CARTESIAN_POINT('Ctrl Pts',(-57.4307255747193,-98.2539476745091,
179.995915330104));
#30970=CARTESIAN_POINT('Ctrl Pts',(-55.7689728122282,-98.3368203924277,
179.995915260595));
#30971=CARTESIAN_POINT('Ctrl Pts',(-54.5910254228517,-98.3681162253198,
178.821287383467));
#30972=CARTESIAN_POINT('Ctrl Pts',(-56.1988062143188,-113.449542435949,
178.821287383467));
#30973=CARTESIAN_POINT('Ctrl Pts',(-55.0208588249424,-113.480838268841,
177.646659506339));
#30974=CARTESIAN_POINT('Ctrl Pts',(-55.0109208311422,-113.387616496817,
175.985484901271));
#30975=CARTESIAN_POINT('Ctrl Pts',(-55.0009828373422,-113.294394724794,
174.324310296203));
#30976=CARTESIAN_POINT('Ctrl Pts',(-56.1590541986307,-113.07665535217,173.149682517375));
#30977=CARTESIAN_POINT('Ctrl Pts',(-57.3171255599192,-112.858915979547,
171.975054738546));
#30978=CARTESIAN_POINT('Ctrl Pts',(-58.9590021965763,-112.589599732318,
171.975054808055));
#30979=CARTESIAN_POINT('Ctrl Pts',(-60.6008788332334,-112.320283485089,
171.975054877564));
#30980=CARTESIAN_POINT('Ctrl Pts',(-61.7589500967758,-112.102544122886,
173.149682754692));
#30981=CARTESIAN_POINT('Ctrl Pts',(-62.9170213603182,-111.884804760683,
174.32431063182));
#30982=CARTESIAN_POINT('Ctrl Pts',(-62.9070832282843,-111.791583003396,
175.985485236888));
#30983=CARTESIAN_POINT('Ctrl Pts',(-62.8971450962504,-111.698361246109,
177.646659841956));
#30984=CARTESIAN_POINT('Ctrl Pts',(-61.7191976091278,-111.729657089422,
178.821287620784));
#30985=CARTESIAN_POINT('Ctrl Pts',(-60.5412501220053,-111.760952932734,
179.995915399612));
#30986=CARTESIAN_POINT('Ctrl Pts',(-58.8794973595142,-111.843825650653,
179.995915330104));
#30987=CARTESIAN_POINT('Ctrl Pts',(-57.217744597023,-111.926698368571,179.995915260595));
#30988=CARTESIAN_POINT('Ctrl Pts',(-56.0397972076466,-111.957994201463,
178.821287383467));
#30989=CARTESIAN_POINT('Ctrl Pts',(-54.8618498182701,-111.989290034355,
177.646659506339));
#30990=CARTESIAN_POINT('Ctrl Pts',(-54.85191182447,-111.896068262332,175.985484901271));
#30991=CARTESIAN_POINT('Ctrl Pts',(-54.8419738306699,-111.802846490308,
174.324310296203));
#30992=CARTESIAN_POINT('Ctrl Pts',(-56.0000451919584,-111.585107117685,
173.149682517375));
#30993=CARTESIAN_POINT('Ctrl Pts',(-57.158116553247,-111.367367745062,171.975054738546));
#30994=CARTESIAN_POINT('Ctrl Pts',(-58.799993189904,-111.098051497832,171.975054808055));
#30995=CARTESIAN_POINT('Ctrl Pts',(-60.4418698265612,-110.828735250603,
171.975054877564));
#30996=CARTESIAN_POINT('Ctrl Pts',(-61.5999410901036,-110.6109958884,173.149682754692));
#30997=CARTESIAN_POINT('Ctrl Pts',(-62.758012353646,-110.393256526198,174.32431063182));
#30998=CARTESIAN_POINT('Ctrl Pts',(-62.7480742216121,-110.30003476891,175.985485236888));
#30999=CARTESIAN_POINT('Ctrl Pts',(-62.7381360895782,-110.206813011623,
177.646659841956));
#31000=CARTESIAN_POINT('Ctrl Pts',(-61.5601886024556,-110.238108854936,
178.821287620784));
#31001=CARTESIAN_POINT('Ctrl Pts',(-60.3822411153331,-110.269404698248,
179.995915399612));
#31002=CARTESIAN_POINT('Ctrl Pts',(-58.7204883528419,-110.352277416167,
179.995915330104));
#31003=CARTESIAN_POINT('Ctrl Pts',(-57.0587355903508,-110.435150134086,
179.995915260595));
#31004=CARTESIAN_POINT('Ctrl Pts',(-55.8807882009743,-110.466445966978,
178.821287383467));
#31005=CARTESIAN_POINT('Ctrl Pts',(-54.7028408115979,-110.49774179987,177.646659506339));
#31006=CARTESIAN_POINT('Ctrl Pts',(-54.6929028177978,-110.404520027846,
175.985484901271));
#31007=CARTESIAN_POINT('Ctrl Pts',(-54.6829648239977,-110.311298255822,
174.324310296203));
#31008=CARTESIAN_POINT('Ctrl Pts',(-55.8410361852862,-110.093558883199,
173.149682517375));
#31009=CARTESIAN_POINT('Ctrl Pts',(-56.9991075465747,-109.875819510576,
171.975054738546));
#31010=CARTESIAN_POINT('Ctrl Pts',(-58.6409841832318,-109.606503263347,
171.975054808055));
#31011=CARTESIAN_POINT('Ctrl Pts',(-60.2828608198889,-109.337187016117,
171.975054877564));
#31012=CARTESIAN_POINT('Ctrl Pts',(-61.4409320834313,-109.119447653915,
173.149682754692));
#31013=CARTESIAN_POINT('Ctrl Pts',(-62.5990033469738,-108.901708291712,
174.32431063182));
#31014=CARTESIAN_POINT('Ctrl Pts',(-62.5890652149398,-108.808486534425,
175.985485236888));
#31015=CARTESIAN_POINT('Ctrl Pts',(-62.5791270829059,-108.715264777138,
177.646659841956));
#31016=CARTESIAN_POINT('Ctrl Pts',(-61.4011795957834,-108.74656062045,178.821287620784));
#31017=CARTESIAN_POINT('Ctrl Pts',(-60.2232321086609,-108.777856463763,
179.995915399612));
#31018=CARTESIAN_POINT('Ctrl Pts',(-58.5614793461697,-108.860729181681,
179.995915330104));
#31019=CARTESIAN_POINT('Ctrl Pts',(-56.8997265836786,-108.9436018996,179.995915260595));
#31020=CARTESIAN_POINT('Ctrl Pts',(-55.7217791943021,-108.974897732492,
178.821287383467));
#31021=CARTESIAN_POINT('Ctrl Pts',(-54.5438318049257,-109.006193565384,
177.646659506339));
#31022=CARTESIAN_POINT('Ctrl Pts',(-54.5338938111256,-108.91297179336,175.985484901271));
#31023=CARTESIAN_POINT('Ctrl Pts',(-54.5239558173255,-108.819750021337,
174.324310296203));
#31024=CARTESIAN_POINT('Ctrl Pts',(-55.682027178614,-108.602010648714,173.149682517375));
#31025=CARTESIAN_POINT('Ctrl Pts',(-56.8400985399025,-108.384271276091,
171.975054738546));
#31026=CARTESIAN_POINT('Ctrl Pts',(-58.4819751765596,-108.114955028861,
171.975054808055));
#31027=CARTESIAN_POINT('Ctrl Pts',(-60.1238518132167,-107.845638781632,
171.975054877564));
#31028=CARTESIAN_POINT('Ctrl Pts',(-61.2819230767591,-107.627899419429,
173.149682754692));
#31029=CARTESIAN_POINT('Ctrl Pts',(-62.4399943403016,-107.410160057226,
174.32431063182));
#31030=CARTESIAN_POINT('Ctrl Pts',(-62.4300562082676,-107.316938299939,
175.985485236888));
#31031=CARTESIAN_POINT('Ctrl Pts',(-62.4201180762337,-107.223716542652,
177.646659841956));
#31032=CARTESIAN_POINT('Ctrl Pts',(-61.2421705891111,-107.255012385965,
178.821287620784));
#31033=CARTESIAN_POINT('Ctrl Pts',(-60.0642231019886,-107.286308229277,
179.995915399612));
#31034=CARTESIAN_POINT('Ctrl Pts',(-58.4024703394975,-107.369180947196,
179.995915330104));
#31035=CARTESIAN_POINT('Ctrl Pts',(-56.7407175770064,-107.452053665114,
179.995915260595));
#31036=CARTESIAN_POINT('Ctrl Pts',(-55.5627701876299,-107.483349498006,
178.821287383467));
#31037=CARTESIAN_POINT('Ctrl Pts',(-54.3848227982534,-107.514645330899,
177.646659506339));
#31038=CARTESIAN_POINT('Ctrl Pts',(-54.3748848044533,-107.421423558875,
175.985484901271));
#31039=CARTESIAN_POINT('Ctrl Pts',(-54.3649468106533,-107.328201786851,
174.324310296203));
#31040=CARTESIAN_POINT('Ctrl Pts',(-55.5230181719417,-107.110462414228,
173.149682517375));
#31041=CARTESIAN_POINT('Ctrl Pts',(-56.6810895332303,-106.892723041605,
171.975054738546));
#31042=CARTESIAN_POINT('Ctrl Pts',(-58.3229661698874,-106.623406794376,
171.975054808055));
#31043=CARTESIAN_POINT('Ctrl Pts',(-59.9648428065445,-106.354090547146,
171.975054877564));
#31044=CARTESIAN_POINT('Ctrl Pts',(-61.1229140700869,-106.136351184943,
173.149682754692));
#31045=CARTESIAN_POINT('Ctrl Pts',(-62.2809853336293,-105.918611822741,
174.32431063182));
#31046=CARTESIAN_POINT('Ctrl Pts',(-62.2710472015954,-105.825390065454,
175.985485236888));
#31047=CARTESIAN_POINT('Ctrl Pts',(-62.2611090695615,-105.732168308167,
177.646659841956));
#31048=CARTESIAN_POINT('Ctrl Pts',(-61.0831615824389,-105.763464151479,
178.821287620784));
#31049=CARTESIAN_POINT('Ctrl Pts',(-59.9052140953164,-105.794759994792,
179.995915399612));
#31050=CARTESIAN_POINT('Ctrl Pts',(-58.2434613328252,-105.87763271271,179.995915330104));
#31051=CARTESIAN_POINT('Ctrl Pts',(-56.5817085703341,-105.960505430629,
179.995915260595));
#31052=CARTESIAN_POINT('Ctrl Pts',(-55.4037611809577,-105.991801263521,
178.821287383467));
#31053=CARTESIAN_POINT('Ctrl Pts',(-54.2258137915812,-106.023097096413,
177.646659506339));
#31054=CARTESIAN_POINT('Ctrl Pts',(-54.2158757977811,-105.929875324389,
175.985484901271));
#31055=CARTESIAN_POINT('Ctrl Pts',(-54.205937803981,-105.836653552366,174.324310296203));
#31056=CARTESIAN_POINT('Ctrl Pts',(-55.3640091652695,-105.618914179742,
173.149682517375));
#31057=CARTESIAN_POINT('Ctrl Pts',(-56.522080526558,-105.401174807119,171.975054738546));
#31058=CARTESIAN_POINT('Ctrl Pts',(-58.1639571632151,-105.13185855989,171.975054808055));
#31059=CARTESIAN_POINT('Ctrl Pts',(-59.8058337998722,-104.862542312661,
171.975054877564));
#31060=CARTESIAN_POINT('Ctrl Pts',(-60.9639050634147,-104.644802950458,
173.149682754692));
#31061=CARTESIAN_POINT('Ctrl Pts',(-62.1219763269571,-104.427063588255,
174.32431063182));
#31062=CARTESIAN_POINT('Ctrl Pts',(-62.1120381949232,-104.333841830968,
175.985485236888));
#31063=CARTESIAN_POINT('Ctrl Pts',(-62.1021000628892,-104.240620073681,
177.646659841956));
#31064=CARTESIAN_POINT('Ctrl Pts',(-60.9241525757667,-104.271915916993,
178.821287620784));
#31065=CARTESIAN_POINT('Ctrl Pts',(-59.7462050886442,-104.303211760306,
179.995915399612));
#31066=CARTESIAN_POINT('Ctrl Pts',(-58.084452326153,-104.386084478225,179.995915330104));
#31067=CARTESIAN_POINT('Ctrl Pts',(-56.4226995636619,-104.468957196143,
179.995915260595));
#31068=CARTESIAN_POINT('Ctrl Pts',(-55.2447521742854,-104.500253029035,
178.821287383467));
#31069=CARTESIAN_POINT('Ctrl Pts',(-54.066804784909,-104.531548861927,177.646659506339));
#31070=CARTESIAN_POINT('Ctrl Pts',(-54.0568667911089,-104.438327089904,
175.985484901271));
#31071=CARTESIAN_POINT('Ctrl Pts',(-54.0469287973088,-104.34510531788,174.324310296203));
#31072=CARTESIAN_POINT('Ctrl Pts',(-55.2050001585973,-104.127365945257,
173.149682517375));
#31073=CARTESIAN_POINT('Ctrl Pts',(-56.3630715198858,-103.909626572634,
171.975054738546));
#31074=CARTESIAN_POINT('Ctrl Pts',(-58.0049481565429,-103.640310325404,
171.975054808055));
#31075=CARTESIAN_POINT('Ctrl Pts',(-59.6468247932,-103.370994078175,171.975054877564));
#31076=CARTESIAN_POINT('Ctrl Pts',(-60.8048960567424,-103.153254715972,
173.149682754692));
#31077=CARTESIAN_POINT('Ctrl Pts',(-61.9629673202849,-102.93551535377,174.32431063182));
#31078=CARTESIAN_POINT('Ctrl Pts',(-61.9530291882509,-102.842293596483,
175.985485236888));
#31079=CARTESIAN_POINT('Ctrl Pts',(-61.943091056217,-102.749071839196,177.646659841956));
#31080=CARTESIAN_POINT('Ctrl Pts',(-60.7651435690945,-102.780367682508,
178.821287620784));
#31081=CARTESIAN_POINT('Ctrl Pts',(-59.587196081972,-102.81166352582,179.995915399612));
#31082=CARTESIAN_POINT('Ctrl Pts',(-57.9254433194808,-102.894536243739,
179.995915330104));
#31083=CARTESIAN_POINT('Ctrl Pts',(-56.2636905569897,-102.977408961658,
179.995915260595));
#31084=CARTESIAN_POINT('Ctrl Pts',(-55.0857431676132,-103.00870479455,178.821287383467));
#31085=CARTESIAN_POINT('Ctrl Pts',(-53.9077957782368,-103.040000627442,
177.646659506339));
#31086=CARTESIAN_POINT('Ctrl Pts',(-53.8978577844367,-102.946778855418,
175.985484901271));
#31087=CARTESIAN_POINT('Ctrl Pts',(-53.8879197906366,-102.853557083394,
174.324310296203));
#31088=CARTESIAN_POINT('Ctrl Pts',(-55.0459911519251,-102.635817710771,
173.149682517375));
#31089=CARTESIAN_POINT('Ctrl Pts',(-56.2040625132136,-102.418078338148,
171.975054738546));
#31090=CARTESIAN_POINT('Ctrl Pts',(-57.8459391498707,-102.148762090919,
171.975054808055));
#31091=CARTESIAN_POINT('Ctrl Pts',(-59.4878157865278,-101.879445843689,
171.975054877564));
#31092=CARTESIAN_POINT('Ctrl Pts',(-60.6458870500702,-101.661706481487,
173.149682754692));
#31093=CARTESIAN_POINT('Ctrl Pts',(-61.8039583136126,-101.443967119284,
174.32431063182));
#31094=CARTESIAN_POINT('Ctrl Pts',(-61.7940201815787,-101.350745361997,
175.985485236888));
#31095=CARTESIAN_POINT('Ctrl Pts',(-61.7840820495448,-101.25752360471,177.646659841956));
#31096=CARTESIAN_POINT('Ctrl Pts',(-60.6061345624222,-101.288819448022,
178.821287620784));
#31097=CARTESIAN_POINT('Ctrl Pts',(-59.4281870752997,-101.320115291335,
179.995915399612));
#31098=CARTESIAN_POINT('Ctrl Pts',(-57.7664343128086,-101.402988009253,
179.995915330104));
#31099=CARTESIAN_POINT('Ctrl Pts',(-56.1046815503175,-101.485860727172,
179.995915260595));
#31100=CARTESIAN_POINT('Ctrl Pts',(-54.926734160941,-101.517156560064,178.821287383467));
#31101=CARTESIAN_POINT('Ctrl Pts',(-53.7487867715645,-101.548452392956,
177.646659506339));
#31102=CARTESIAN_POINT('Ctrl Pts',(-53.7388487777644,-101.455230620932,
175.985484901271));
#31103=CARTESIAN_POINT('Ctrl Pts',(-53.7289107839643,-101.362008848909,
174.324310296203));
#31104=CARTESIAN_POINT('Ctrl Pts',(-54.8869821452528,-101.144269476286,
173.149682517375));
#31105=CARTESIAN_POINT('Ctrl Pts',(-56.0450535065414,-100.926530103662,
171.975054738546));
#31106=CARTESIAN_POINT('Ctrl Pts',(-57.6869301431984,-100.657213856433,
171.975054808055));
#31107=CARTESIAN_POINT('Ctrl Pts',(-59.3288067798556,-100.387897609204,
171.975054877564));
#31108=CARTESIAN_POINT('Ctrl Pts',(-60.486878043398,-100.170158247001,173.149682754692));
#31109=CARTESIAN_POINT('Ctrl Pts',(-61.6449493069404,-99.9524188847983,
174.32431063182));
#31110=CARTESIAN_POINT('Ctrl Pts',(-61.6350111749065,-99.8591971275113,
175.985485236888));
#31111=CARTESIAN_POINT('Ctrl Pts',(-61.6250730428726,-99.7659753702243,
177.646659841956));
#31112=CARTESIAN_POINT('Ctrl Pts',(-60.44712555575,-99.7972712135367,178.821287620784));
#31113=CARTESIAN_POINT('Ctrl Pts',(-59.2691780686275,-99.8285670568492,
179.995915399612));
#31114=CARTESIAN_POINT('Ctrl Pts',(-57.6074253061363,-99.9114397747677,
179.995915330104));
#31115=CARTESIAN_POINT('Ctrl Pts',(-55.9456725436452,-99.9943124926864,
179.995915260595));
#31116=CARTESIAN_POINT('Ctrl Pts',(-54.7677251542687,-100.025608325578,
178.821287383467));
#31117=CARTESIAN_POINT('Ctrl Pts',(-53.5897777648923,-100.05690415847,177.646659506339));
#31118=CARTESIAN_POINT('Ctrl Pts',(-53.5798397710922,-99.9636823864468,
175.985484901271));
#31119=CARTESIAN_POINT('Ctrl Pts',(-53.5699017772921,-99.8704606144232,
174.324310296203));
#31120=CARTESIAN_POINT('Ctrl Pts',(-54.7279731385806,-99.6527212418,173.149682517375));
#31121=CARTESIAN_POINT('Ctrl Pts',(-55.8860444998691,-99.4349818691769,
171.975054738546));
#31122=CARTESIAN_POINT('Ctrl Pts',(-57.5279211365262,-99.1656656219475,
171.975054808055));
#31123=CARTESIAN_POINT('Ctrl Pts',(-59.1697977731833,-98.8963493747183,
171.975054877564));
#31124=CARTESIAN_POINT('Ctrl Pts',(-60.3278690367257,-98.6786100125155,
173.149682754692));
#31125=CARTESIAN_POINT('Ctrl Pts',(-61.4859403002682,-98.4608706503128,
174.32431063182));
#31126=CARTESIAN_POINT('Ctrl Pts',(-61.4760021682342,-98.3676488930257,
175.985485236888));
#31127=CARTESIAN_POINT('Ctrl Pts',(-61.4660640362003,-98.2744271357387,
177.646659841956));
#31128=CARTESIAN_POINT('Ctrl Pts',(-60.2881165490778,-98.3057229790511,
178.821287620784));
#31129=CARTESIAN_POINT('Ctrl Pts',(-59.1101690619552,-98.3370188223636,
179.995915399612));
#31130=CARTESIAN_POINT('Ctrl Pts',(-57.4484162994641,-98.4198915402821,
179.995915330104));
#31131=CARTESIAN_POINT('Ctrl Pts',(-55.786663536973,-98.5027642582008,179.995915260595));
#31132=CARTESIAN_POINT('Ctrl Pts',(-54.6087161475965,-98.5340600910929,
178.821287383467));
#31133=CARTESIAN_POINT('Ctrl Pts',(-56.2237961054143,-113.614380048479,
178.813912075476));
#31134=CARTESIAN_POINT('Ctrl Pts',(-55.0488864554725,-113.645352038053,
177.6423391512));
#31135=CARTESIAN_POINT('Ctrl Pts',(-55.0389484614927,-113.552130266048,
175.985484901707));
#31136=CARTESIAN_POINT('Ctrl Pts',(-55.0290104675128,-113.458908494044,
174.328630652215));
#31137=CARTESIAN_POINT('Ctrl Pts',(-56.1840440891124,-113.241492964766,
173.157057825983));
#31138=CARTESIAN_POINT('Ctrl Pts',(-57.3390777107121,-113.024077435489,
171.985484999752));
#31139=CARTESIAN_POINT('Ctrl Pts',(-58.9766583348819,-112.755219171892,
171.985485069079));
#31140=CARTESIAN_POINT('Ctrl Pts',(-60.6142389590518,-112.486360908295,
171.985485138407));
#31141=CARTESIAN_POINT('Ctrl Pts',(-61.7692724831595,-112.268945389411,
173.157058062683));
#31142=CARTESIAN_POINT('Ctrl Pts',(-62.9243060072673,-112.051529870527,
174.328630986959));
#31143=CARTESIAN_POINT('Ctrl Pts',(-62.9143678754131,-111.95830811322,175.985485236451));
#31144=CARTESIAN_POINT('Ctrl Pts',(-62.9044297435589,-111.865086355914,
177.642339485944));
#31145=CARTESIAN_POINT('Ctrl Pts',(-61.7295199961253,-111.896058355881,
178.813912312176));
#31146=CARTESIAN_POINT('Ctrl Pts',(-60.5546102486917,-111.927030355848,
179.985485138407));
#31147=CARTESIAN_POINT('Ctrl Pts',(-58.8971534986878,-112.009445090134,
179.985485069079));
#31148=CARTESIAN_POINT('Ctrl Pts',(-57.2396967486839,-112.09185982442,179.985484999752));
#31149=CARTESIAN_POINT('Ctrl Pts',(-56.0647870987421,-112.122831813994,
178.813912075476));
#31150=CARTESIAN_POINT('Ctrl Pts',(-54.8898774488003,-112.153803803567,
177.6423391512));
#31151=CARTESIAN_POINT('Ctrl Pts',(-54.8799394548205,-112.060582031563,
175.985484901707));
#31152=CARTESIAN_POINT('Ctrl Pts',(-54.8700014608406,-111.967360259558,
174.328630652215));
#31153=CARTESIAN_POINT('Ctrl Pts',(-56.0250350824402,-111.749944730281,
173.157057825983));
#31154=CARTESIAN_POINT('Ctrl Pts',(-57.1800687040398,-111.532529201003,
171.985484999752));
#31155=CARTESIAN_POINT('Ctrl Pts',(-58.8176493282097,-111.263670937406,
171.985485069079));
#31156=CARTESIAN_POINT('Ctrl Pts',(-60.4552299523796,-110.994812673809,
171.985485138407));
#31157=CARTESIAN_POINT('Ctrl Pts',(-61.6102634764873,-110.777397154925,
173.157058062683));
#31158=CARTESIAN_POINT('Ctrl Pts',(-62.7652970005951,-110.559981636041,
174.328630986959));
#31159=CARTESIAN_POINT('Ctrl Pts',(-62.7553588687409,-110.466759878735,
175.985485236451));
#31160=CARTESIAN_POINT('Ctrl Pts',(-62.7454207368867,-110.373538121429,
177.642339485944));
#31161=CARTESIAN_POINT('Ctrl Pts',(-61.5705109894531,-110.404510121395,
178.813912312176));
#31162=CARTESIAN_POINT('Ctrl Pts',(-60.3956012420194,-110.435482121362,
179.985485138407));
#31163=CARTESIAN_POINT('Ctrl Pts',(-58.7381444920155,-110.517896855648,
179.985485069079));
#31164=CARTESIAN_POINT('Ctrl Pts',(-57.0806877420116,-110.600311589935,
179.985484999752));
#31165=CARTESIAN_POINT('Ctrl Pts',(-55.9057780920699,-110.631283579508,
178.813912075476));
#31166=CARTESIAN_POINT('Ctrl Pts',(-54.7308684421281,-110.662255569082,
177.6423391512));
#31167=CARTESIAN_POINT('Ctrl Pts',(-54.7209304481482,-110.569033797077,
175.985484901707));
#31168=CARTESIAN_POINT('Ctrl Pts',(-54.7109924541684,-110.475812025073,
174.328630652215));
#31169=CARTESIAN_POINT('Ctrl Pts',(-55.866026075768,-110.258396495795,173.157057825983));
#31170=CARTESIAN_POINT('Ctrl Pts',(-57.0210596973676,-110.040980966518,
171.985484999752));
#31171=CARTESIAN_POINT('Ctrl Pts',(-58.6586403215375,-109.772122702921,
171.985485069079));
#31172=CARTESIAN_POINT('Ctrl Pts',(-60.2962209457073,-109.503264439324,
171.985485138407));
#31173=CARTESIAN_POINT('Ctrl Pts',(-61.4512544698151,-109.28584892044,173.157058062683));
#31174=CARTESIAN_POINT('Ctrl Pts',(-62.6062879939228,-109.068433401555,
174.328630986959));
#31175=CARTESIAN_POINT('Ctrl Pts',(-62.5963498620687,-108.975211644249,
175.985485236451));
#31176=CARTESIAN_POINT('Ctrl Pts',(-62.5864117302145,-108.881989886943,
177.642339485944));
#31177=CARTESIAN_POINT('Ctrl Pts',(-61.4115019827808,-108.91296188691,178.813912312176));
#31178=CARTESIAN_POINT('Ctrl Pts',(-60.2365922353472,-108.943933886877,
179.985485138407));
#31179=CARTESIAN_POINT('Ctrl Pts',(-58.5791354853433,-109.026348621163,
179.985485069079));
#31180=CARTESIAN_POINT('Ctrl Pts',(-56.9216787353394,-109.108763355449,
179.985484999752));
#31181=CARTESIAN_POINT('Ctrl Pts',(-55.7467690853976,-109.139735345023,
178.813912075476));
#31182=CARTESIAN_POINT('Ctrl Pts',(-54.5718594354559,-109.170707334596,
177.6423391512));
#31183=CARTESIAN_POINT('Ctrl Pts',(-54.561921441476,-109.077485562592,175.985484901707));
#31184=CARTESIAN_POINT('Ctrl Pts',(-54.5519834474962,-108.984263790587,
174.328630652215));
#31185=CARTESIAN_POINT('Ctrl Pts',(-55.7070170690958,-108.76684826131,173.157057825983));
#31186=CARTESIAN_POINT('Ctrl Pts',(-56.8620506906954,-108.549432732032,
171.985484999752));
#31187=CARTESIAN_POINT('Ctrl Pts',(-58.4996313148652,-108.280574468435,
171.985485069079));
#31188=CARTESIAN_POINT('Ctrl Pts',(-60.1372119390351,-108.011716204838,
171.985485138407));
#31189=CARTESIAN_POINT('Ctrl Pts',(-61.2922454631428,-107.794300685954,
173.157058062683));
#31190=CARTESIAN_POINT('Ctrl Pts',(-62.4472789872506,-107.57688516707,174.328630986959));
#31191=CARTESIAN_POINT('Ctrl Pts',(-62.4373408553964,-107.483663409764,
175.985485236451));
#31192=CARTESIAN_POINT('Ctrl Pts',(-62.4274027235423,-107.390441652457,
177.642339485944));
#31193=CARTESIAN_POINT('Ctrl Pts',(-61.2524929761086,-107.421413652424,
178.813912312176));
#31194=CARTESIAN_POINT('Ctrl Pts',(-60.077583228675,-107.452385652391,179.985485138407));
#31195=CARTESIAN_POINT('Ctrl Pts',(-58.4201264786711,-107.534800386677,
179.985485069079));
#31196=CARTESIAN_POINT('Ctrl Pts',(-56.7626697286672,-107.617215120964,
179.985484999752));
#31197=CARTESIAN_POINT('Ctrl Pts',(-55.5877600787254,-107.648187110537,
178.813912075476));
#31198=CARTESIAN_POINT('Ctrl Pts',(-54.4128504287836,-107.67915910011,177.6423391512));
#31199=CARTESIAN_POINT('Ctrl Pts',(-54.4029124348038,-107.585937328106,
175.985484901707));
#31200=CARTESIAN_POINT('Ctrl Pts',(-54.3929744408239,-107.492715556102,
174.328630652215));
#31201=CARTESIAN_POINT('Ctrl Pts',(-55.5480080624235,-107.275300026824,
173.157057825983));
#31202=CARTESIAN_POINT('Ctrl Pts',(-56.7030416840231,-107.057884497547,
171.985484999752));
#31203=CARTESIAN_POINT('Ctrl Pts',(-58.340622308193,-106.78902623395,171.985485069079));
#31204=CARTESIAN_POINT('Ctrl Pts',(-59.9782029323629,-106.520167970353,
171.985485138407));
#31205=CARTESIAN_POINT('Ctrl Pts',(-61.1332364564706,-106.302752451468,
173.157058062683));
#31206=CARTESIAN_POINT('Ctrl Pts',(-62.2882699805784,-106.085336932584,
174.328630986959));
#31207=CARTESIAN_POINT('Ctrl Pts',(-62.2783318487242,-105.992115175278,
175.985485236451));
#31208=CARTESIAN_POINT('Ctrl Pts',(-62.26839371687,-105.898893417972,177.642339485944));
#31209=CARTESIAN_POINT('Ctrl Pts',(-61.0934839694364,-105.929865417939,
178.813912312176));
#31210=CARTESIAN_POINT('Ctrl Pts',(-59.9185742220028,-105.960837417905,
179.985485138407));
#31211=CARTESIAN_POINT('Ctrl Pts',(-58.2611174719989,-106.043252152192,
179.985485069079));
#31212=CARTESIAN_POINT('Ctrl Pts',(-56.603660721995,-106.125666886478,179.985484999752));
#31213=CARTESIAN_POINT('Ctrl Pts',(-55.4287510720532,-106.156638876051,
178.813912075476));
#31214=CARTESIAN_POINT('Ctrl Pts',(-54.2538414221114,-106.187610865625,
177.6423391512));
#31215=CARTESIAN_POINT('Ctrl Pts',(-54.2439034281315,-106.09438909362,175.985484901707));
#31216=CARTESIAN_POINT('Ctrl Pts',(-54.2339654341517,-106.001167321616,
174.328630652215));
#31217=CARTESIAN_POINT('Ctrl Pts',(-55.3889990557513,-105.783751792338,
173.157057825983));
#31218=CARTESIAN_POINT('Ctrl Pts',(-56.5440326773509,-105.566336263061,
171.985484999752));
#31219=CARTESIAN_POINT('Ctrl Pts',(-58.1816133015208,-105.297477999464,
171.985485069079));
#31220=CARTESIAN_POINT('Ctrl Pts',(-59.8191939256906,-105.028619735867,
171.985485138407));
#31221=CARTESIAN_POINT('Ctrl Pts',(-60.9742274497984,-104.811204216983,
173.157058062683));
#31222=CARTESIAN_POINT('Ctrl Pts',(-62.1292609739061,-104.593788698099,
174.328630986959));
#31223=CARTESIAN_POINT('Ctrl Pts',(-62.119322842052,-104.500566940792,175.985485236451));
#31224=CARTESIAN_POINT('Ctrl Pts',(-62.1093847101978,-104.407345183486,
177.642339485944));
#31225=CARTESIAN_POINT('Ctrl Pts',(-60.9344749627642,-104.438317183453,
178.813912312176));
#31226=CARTESIAN_POINT('Ctrl Pts',(-59.7595652153305,-104.46928918342,179.985485138407));
#31227=CARTESIAN_POINT('Ctrl Pts',(-58.1021084653266,-104.551703917706,
179.985485069079));
#31228=CARTESIAN_POINT('Ctrl Pts',(-56.4446517153227,-104.634118651992,
179.985484999752));
#31229=CARTESIAN_POINT('Ctrl Pts',(-55.269742065381,-104.665090641566,178.813912075476));
#31230=CARTESIAN_POINT('Ctrl Pts',(-54.0948324154392,-104.696062631139,
177.6423391512));
#31231=CARTESIAN_POINT('Ctrl Pts',(-54.0848944214593,-104.602840859135,
175.985484901707));
#31232=CARTESIAN_POINT('Ctrl Pts',(-54.0749564274795,-104.50961908713,174.328630652215));
#31233=CARTESIAN_POINT('Ctrl Pts',(-55.2299900490791,-104.292203557853,
173.157057825983));
#31234=CARTESIAN_POINT('Ctrl Pts',(-56.3850236706787,-104.074788028575,
171.985484999752));
#31235=CARTESIAN_POINT('Ctrl Pts',(-58.0226042948486,-103.805929764978,
171.985485069079));
#31236=CARTESIAN_POINT('Ctrl Pts',(-59.6601849190184,-103.537071501381,
171.985485138407));
#31237=CARTESIAN_POINT('Ctrl Pts',(-60.8152184431262,-103.319655982497,
173.157058062683));
#31238=CARTESIAN_POINT('Ctrl Pts',(-61.9702519672339,-103.102240463613,
174.328630986959));
#31239=CARTESIAN_POINT('Ctrl Pts',(-61.9603138353797,-103.009018706307,
175.985485236451));
#31240=CARTESIAN_POINT('Ctrl Pts',(-61.9503757035256,-102.915796949001,
177.642339485944));
#31241=CARTESIAN_POINT('Ctrl Pts',(-60.7754659560919,-102.946768948967,
178.813912312176));
#31242=CARTESIAN_POINT('Ctrl Pts',(-59.6005562086583,-102.977740948934,
179.985485138407));
#31243=CARTESIAN_POINT('Ctrl Pts',(-57.9430994586544,-103.06015568322,179.985485069079));
#31244=CARTESIAN_POINT('Ctrl Pts',(-56.2856427086505,-103.142570417507,
179.985484999752));
#31245=CARTESIAN_POINT('Ctrl Pts',(-55.1107330587087,-103.17354240708,178.813912075476));
#31246=CARTESIAN_POINT('Ctrl Pts',(-53.935823408767,-103.204514396654,177.6423391512));
#31247=CARTESIAN_POINT('Ctrl Pts',(-53.9258854147871,-103.111292624649,
175.985484901707));
#31248=CARTESIAN_POINT('Ctrl Pts',(-53.9159474208072,-103.018070852645,
174.328630652215));
#31249=CARTESIAN_POINT('Ctrl Pts',(-55.0709810424069,-102.800655323367,
173.157057825983));
#31250=CARTESIAN_POINT('Ctrl Pts',(-56.2260146640065,-102.58323979409,171.985484999752));
#31251=CARTESIAN_POINT('Ctrl Pts',(-57.8635952881763,-102.314381530493,
171.985485069079));
#31252=CARTESIAN_POINT('Ctrl Pts',(-59.5011759123462,-102.045523266896,
171.985485138407));
#31253=CARTESIAN_POINT('Ctrl Pts',(-60.6562094364539,-101.828107748012,
173.157058062683));
#31254=CARTESIAN_POINT('Ctrl Pts',(-61.8112429605617,-101.610692229127,
174.328630986959));
#31255=CARTESIAN_POINT('Ctrl Pts',(-61.8013048287075,-101.517470471821,
175.985485236451));
#31256=CARTESIAN_POINT('Ctrl Pts',(-61.7913666968533,-101.424248714515,
177.642339485944));
#31257=CARTESIAN_POINT('Ctrl Pts',(-60.6164569494197,-101.455220714482,
178.813912312176));
#31258=CARTESIAN_POINT('Ctrl Pts',(-59.4415472019861,-101.486192714449,
179.985485138407));
#31259=CARTESIAN_POINT('Ctrl Pts',(-57.7840904519822,-101.568607448735,
179.985485069079));
#31260=CARTESIAN_POINT('Ctrl Pts',(-56.1266337019783,-101.651022183021,
179.985484999752));
#31261=CARTESIAN_POINT('Ctrl Pts',(-54.9517240520365,-101.681994172595,
178.813912075476));
#31262=CARTESIAN_POINT('Ctrl Pts',(-53.7768144020947,-101.712966162168,
177.6423391512));
#31263=CARTESIAN_POINT('Ctrl Pts',(-53.7668764081149,-101.619744390164,
175.985484901707));
#31264=CARTESIAN_POINT('Ctrl Pts',(-53.756938414135,-101.526522618159,174.328630652215));
#31265=CARTESIAN_POINT('Ctrl Pts',(-54.9119720357346,-101.309107088882,
173.157057825983));
#31266=CARTESIAN_POINT('Ctrl Pts',(-56.0670056573342,-101.091691559604,
171.985484999752));
#31267=CARTESIAN_POINT('Ctrl Pts',(-57.7045862815041,-100.822833296007,
171.985485069079));
#31268=CARTESIAN_POINT('Ctrl Pts',(-59.342166905674,-100.55397503241,171.985485138407));
#31269=CARTESIAN_POINT('Ctrl Pts',(-60.4972004297817,-100.336559513526,
173.157058062683));
#31270=CARTESIAN_POINT('Ctrl Pts',(-61.6522339538895,-100.119143994642,
174.328630986959));
#31271=CARTESIAN_POINT('Ctrl Pts',(-61.6422958220353,-100.025922237336,
175.985485236451));
#31272=CARTESIAN_POINT('Ctrl Pts',(-61.6323576901811,-99.9327004800294,
177.642339485944));
#31273=CARTESIAN_POINT('Ctrl Pts',(-60.4574479427475,-99.9636724799962,
178.813912312176));
#31274=CARTESIAN_POINT('Ctrl Pts',(-59.2825381953138,-99.994644479963,179.985485138407));
#31275=CARTESIAN_POINT('Ctrl Pts',(-57.6250814453099,-100.077059214249,
179.985485069079));
#31276=CARTESIAN_POINT('Ctrl Pts',(-55.9676246953061,-100.159473948536,
179.985484999752));
#31277=CARTESIAN_POINT('Ctrl Pts',(-54.7927150453643,-100.190445938109,
178.813912075476));
#31278=CARTESIAN_POINT('Ctrl Pts',(-53.6178053954225,-100.221417927683,
177.6423391512));
#31279=CARTESIAN_POINT('Ctrl Pts',(-53.6078674014426,-100.128196155678,
175.985484901707));
#31280=CARTESIAN_POINT('Ctrl Pts',(-53.5979294074628,-100.034974383673,
174.328630652215));
#31281=CARTESIAN_POINT('Ctrl Pts',(-54.7529630290624,-99.817558854396,173.157057825983));
#31282=CARTESIAN_POINT('Ctrl Pts',(-55.907996650662,-99.6001433251185,171.985484999752));
#31283=CARTESIAN_POINT('Ctrl Pts',(-57.5455772748319,-99.3312850615215,
171.985485069079));
#31284=CARTESIAN_POINT('Ctrl Pts',(-59.1831578990017,-99.0624267979246,
171.985485138407));
#31285=CARTESIAN_POINT('Ctrl Pts',(-60.3381914231095,-98.8450112790404,
173.157058062683));
#31286=CARTESIAN_POINT('Ctrl Pts',(-61.4932249472172,-98.6275957601562,
174.328630986959));
#31287=CARTESIAN_POINT('Ctrl Pts',(-61.4832868153631,-98.53437400285,175.985485236451));
#31288=CARTESIAN_POINT('Ctrl Pts',(-61.4733486835089,-98.4411522455438,
177.642339485944));
#31289=CARTESIAN_POINT('Ctrl Pts',(-60.2984389360752,-98.4721242455106,
178.813912312176));
#31290=CARTESIAN_POINT('Ctrl Pts',(-59.1235291886416,-98.5030962454774,
179.985485138407));
#31291=CARTESIAN_POINT('Ctrl Pts',(-57.4660724386377,-98.5855109797636,
179.985485069079));
#31292=CARTESIAN_POINT('Ctrl Pts',(-55.8086156886338,-98.6679257140499,
179.985484999752));
#31293=CARTESIAN_POINT('Ctrl Pts',(-54.633706038692,-98.6988977036234,178.813912075476));
#31294=CARTESIAN_POINT('Ctrl Pts',(-56.8733667677527,-112.709647553905,
178.072094410988));
#31295=CARTESIAN_POINT('Ctrl Pts',(-56.0039967339745,-112.708046979118,
177.207792449865));
#31296=CARTESIAN_POINT('Ctrl Pts',(-55.9940587219143,-112.614825209041,
175.985484945604));
#31297=CARTESIAN_POINT('Ctrl Pts',(-55.9841207098542,-112.521603438964,
174.763177441344));
#31298=CARTESIAN_POINT('Ctrl Pts',(-56.8336146897208,-112.336760476773,
173.89887555255));
#31299=CARTESIAN_POINT('Ctrl Pts',(-57.6831086695875,-112.151917514582,
173.034573663757));
#31300=CARTESIAN_POINT('Ctrl Pts',(-58.8885910066563,-111.929123815193,
173.034573714903));
#31301=CARTESIAN_POINT('Ctrl Pts',(-60.0940733437252,-111.706330115804,
173.034573766048));
#31302=CARTESIAN_POINT('Ctrl Pts',(-60.9435672516694,-111.521487161281,
173.898875727171));
#31303=CARTESIAN_POINT('Ctrl Pts',(-61.7930611596136,-111.336644206758,
174.763177688294));
#31304=CARTESIAN_POINT('Ctrl Pts',(-61.7831230458397,-111.243422447524,
175.985485192554));
#31305=CARTESIAN_POINT('Ctrl Pts',(-61.7731849320658,-111.15020068829,177.207792696815));
#31306=CARTESIAN_POINT('Ctrl Pts',(-60.9038148263651,-111.14860012117,178.072094585608));
#31307=CARTESIAN_POINT('Ctrl Pts',(-60.0344447206644,-111.14699955405,178.936396474401));
#31308=CARTESIAN_POINT('Ctrl Pts',(-58.8090862577616,-111.183349724129,
178.936396423256));
#31309=CARTESIAN_POINT('Ctrl Pts',(-57.5837277948587,-111.219699894207,
178.936396372111));
#31310=CARTESIAN_POINT('Ctrl Pts',(-56.7143577610805,-111.21809931942,178.072094410988));
#31311=CARTESIAN_POINT('Ctrl Pts',(-55.8449877273022,-111.216498744632,
177.207792449865));
#31312=CARTESIAN_POINT('Ctrl Pts',(-55.8350497152421,-111.123276974555,
175.985484945604));
#31313=CARTESIAN_POINT('Ctrl Pts',(-55.8251117031819,-111.030055204478,
174.763177441344));
#31314=CARTESIAN_POINT('Ctrl Pts',(-56.6746056830486,-110.845212242287,
173.89887555255));
#31315=CARTESIAN_POINT('Ctrl Pts',(-57.5240996629153,-110.660369280097,
173.034573663757));
#31316=CARTESIAN_POINT('Ctrl Pts',(-58.7295819999841,-110.437575580708,
173.034573714903));
#31317=CARTESIAN_POINT('Ctrl Pts',(-59.9350643370529,-110.214781881319,
173.034573766048));
#31318=CARTESIAN_POINT('Ctrl Pts',(-60.7845582449971,-110.029938926795,
173.898875727171));
#31319=CARTESIAN_POINT('Ctrl Pts',(-61.6340521529414,-109.845095972272,
174.763177688294));
#31320=CARTESIAN_POINT('Ctrl Pts',(-61.6241140391675,-109.751874213038,
175.985485192554));
#31321=CARTESIAN_POINT('Ctrl Pts',(-61.6141759253936,-109.658652453805,
177.207792696815));
#31322=CARTESIAN_POINT('Ctrl Pts',(-60.7448058196929,-109.657051886685,
178.072094585608));
#31323=CARTESIAN_POINT('Ctrl Pts',(-59.8754357139922,-109.655451319565,
178.936396474401));
#31324=CARTESIAN_POINT('Ctrl Pts',(-58.6500772510893,-109.691801489643,
178.936396423256));
#31325=CARTESIAN_POINT('Ctrl Pts',(-57.4247187881865,-109.728151659721,
178.936396372111));
#31326=CARTESIAN_POINT('Ctrl Pts',(-56.5553487544082,-109.726551084934,
178.072094410988));
#31327=CARTESIAN_POINT('Ctrl Pts',(-55.68597872063,-109.724950510147,177.207792449865));
#31328=CARTESIAN_POINT('Ctrl Pts',(-55.6760407085698,-109.63172874007,175.985484945604));
#31329=CARTESIAN_POINT('Ctrl Pts',(-55.6661026965097,-109.538506969993,
174.763177441344));
#31330=CARTESIAN_POINT('Ctrl Pts',(-56.5155966763764,-109.353664007802,
173.89887555255));
#31331=CARTESIAN_POINT('Ctrl Pts',(-57.365090656243,-109.168821045611,173.034573663757));
#31332=CARTESIAN_POINT('Ctrl Pts',(-58.5705729933119,-108.946027346222,
173.034573714903));
#31333=CARTESIAN_POINT('Ctrl Pts',(-59.7760553303807,-108.723233646833,
173.034573766048));
#31334=CARTESIAN_POINT('Ctrl Pts',(-60.6255492383249,-108.53839069231,173.898875727171));
#31335=CARTESIAN_POINT('Ctrl Pts',(-61.4750431462691,-108.353547737786,
174.763177688294));
#31336=CARTESIAN_POINT('Ctrl Pts',(-61.4651050324952,-108.260325978553,
175.985485192554));
#31337=CARTESIAN_POINT('Ctrl Pts',(-61.4551669187214,-108.167104219319,
177.207792696815));
#31338=CARTESIAN_POINT('Ctrl Pts',(-60.5857968130207,-108.165503652199,
178.072094585608));
#31339=CARTESIAN_POINT('Ctrl Pts',(-59.71642670732,-108.163903085079,178.936396474401));
#31340=CARTESIAN_POINT('Ctrl Pts',(-58.4910682444171,-108.200253255158,
178.936396423256));
#31341=CARTESIAN_POINT('Ctrl Pts',(-57.2657097815143,-108.236603425236,
178.936396372111));
#31342=CARTESIAN_POINT('Ctrl Pts',(-56.396339747736,-108.235002850448,178.072094410988));
#31343=CARTESIAN_POINT('Ctrl Pts',(-55.5269697139578,-108.233402275661,
177.207792449865));
#31344=CARTESIAN_POINT('Ctrl Pts',(-55.5170317018976,-108.140180505584,
175.985484945604));
#31345=CARTESIAN_POINT('Ctrl Pts',(-55.5070936898375,-108.046958735507,
174.763177441344));
#31346=CARTESIAN_POINT('Ctrl Pts',(-56.3565876697041,-107.862115773316,
173.89887555255));
#31347=CARTESIAN_POINT('Ctrl Pts',(-57.2060816495708,-107.677272811126,
173.034573663757));
#31348=CARTESIAN_POINT('Ctrl Pts',(-58.4115639866396,-107.454479111736,
173.034573714903));
#31349=CARTESIAN_POINT('Ctrl Pts',(-59.6170463237085,-107.231685412347,
173.034573766048));
#31350=CARTESIAN_POINT('Ctrl Pts',(-60.4665402316527,-107.046842457824,
173.898875727171));
#31351=CARTESIAN_POINT('Ctrl Pts',(-61.3160341395969,-106.861999503301,
174.763177688294));
#31352=CARTESIAN_POINT('Ctrl Pts',(-61.306096025823,-106.768777744067,175.985485192554));
#31353=CARTESIAN_POINT('Ctrl Pts',(-61.2961579120492,-106.675555984834,
177.207792696815));
#31354=CARTESIAN_POINT('Ctrl Pts',(-60.4267878063484,-106.673955417714,
178.072094585608));
#31355=CARTESIAN_POINT('Ctrl Pts',(-59.5574177006478,-106.672354850594,
178.936396474401));
#31356=CARTESIAN_POINT('Ctrl Pts',(-58.3320592377449,-106.708705020672,
178.936396423256));
#31357=CARTESIAN_POINT('Ctrl Pts',(-57.106700774842,-106.74505519075,178.936396372111));
#31358=CARTESIAN_POINT('Ctrl Pts',(-56.2373307410638,-106.743454615963,
178.072094410988));
#31359=CARTESIAN_POINT('Ctrl Pts',(-55.3679607072856,-106.741854041175,
177.207792449865));
#31360=CARTESIAN_POINT('Ctrl Pts',(-55.3580226952254,-106.648632271098,
175.985484945604));
#31361=CARTESIAN_POINT('Ctrl Pts',(-55.3480846831652,-106.555410501021,
174.763177441344));
#31362=CARTESIAN_POINT('Ctrl Pts',(-56.1975786630319,-106.370567538831,
173.89887555255));
#31363=CARTESIAN_POINT('Ctrl Pts',(-57.0470726428986,-106.18572457664,173.034573663757));
#31364=CARTESIAN_POINT('Ctrl Pts',(-58.2525549799674,-105.962930877251,
173.034573714903));
#31365=CARTESIAN_POINT('Ctrl Pts',(-59.4580373170363,-105.740137177862,
173.034573766048));
#31366=CARTESIAN_POINT('Ctrl Pts',(-60.3075312249805,-105.555294223339,
173.898875727171));
#31367=CARTESIAN_POINT('Ctrl Pts',(-61.1570251329247,-105.370451268815,
174.763177688294));
#31368=CARTESIAN_POINT('Ctrl Pts',(-61.1470870191508,-105.277229509582,
175.985485192554));
#31369=CARTESIAN_POINT('Ctrl Pts',(-61.1371489053769,-105.184007750348,
177.207792696815));
#31370=CARTESIAN_POINT('Ctrl Pts',(-60.2677787996762,-105.182407183228,
178.072094585608));
#31371=CARTESIAN_POINT('Ctrl Pts',(-59.3984086939755,-105.180806616108,
178.936396474401));
#31372=CARTESIAN_POINT('Ctrl Pts',(-58.1730502310727,-105.217156786186,
178.936396423256));
#31373=CARTESIAN_POINT('Ctrl Pts',(-56.9476917681698,-105.253506956265,
178.936396372111));
#31374=CARTESIAN_POINT('Ctrl Pts',(-56.0783217343916,-105.251906381477,
178.072094410988));
#31375=CARTESIAN_POINT('Ctrl Pts',(-55.2089517006133,-105.25030580669,177.207792449865));
#31376=CARTESIAN_POINT('Ctrl Pts',(-55.1990136885532,-105.157084036613,
175.985484945604));
#31377=CARTESIAN_POINT('Ctrl Pts',(-55.189075676493,-105.063862266536,174.763177441344));
#31378=CARTESIAN_POINT('Ctrl Pts',(-56.0385696563597,-104.879019304345,
173.89887555255));
#31379=CARTESIAN_POINT('Ctrl Pts',(-56.8880636362264,-104.694176342154,
173.034573663757));
#31380=CARTESIAN_POINT('Ctrl Pts',(-58.0935459732952,-104.471382642765,
173.034573714903));
#31381=CARTESIAN_POINT('Ctrl Pts',(-59.299028310364,-104.248588943376,173.034573766048));
#31382=CARTESIAN_POINT('Ctrl Pts',(-60.1485222183082,-104.063745988853,
173.898875727171));
#31383=CARTESIAN_POINT('Ctrl Pts',(-60.9980161262524,-103.87890303433,174.763177688294));
#31384=CARTESIAN_POINT('Ctrl Pts',(-60.9880780124786,-103.785681275096,
175.985485192554));
#31385=CARTESIAN_POINT('Ctrl Pts',(-60.9781398987047,-103.692459515862,
177.207792696815));
#31386=CARTESIAN_POINT('Ctrl Pts',(-60.108769793004,-103.690858948742,178.072094585608));
#31387=CARTESIAN_POINT('Ctrl Pts',(-59.2393996873033,-103.689258381622,
178.936396474401));
#31388=CARTESIAN_POINT('Ctrl Pts',(-58.0140412244004,-103.725608551701,
178.936396423256));
#31389=CARTESIAN_POINT('Ctrl Pts',(-56.7886827614976,-103.761958721779,
178.936396372111));
#31390=CARTESIAN_POINT('Ctrl Pts',(-55.9193127277193,-103.760358146992,
178.072094410988));
#31391=CARTESIAN_POINT('Ctrl Pts',(-55.0499426939411,-103.758757572204,
177.207792449865));
#31392=CARTESIAN_POINT('Ctrl Pts',(-55.0400046818809,-103.665535802127,
175.985484945604));
#31393=CARTESIAN_POINT('Ctrl Pts',(-55.0300666698208,-103.57231403205,174.763177441344));
#31394=CARTESIAN_POINT('Ctrl Pts',(-55.8795606496874,-103.387471069859,
173.89887555255));
#31395=CARTESIAN_POINT('Ctrl Pts',(-56.7290546295541,-103.202628107669,
173.034573663757));
#31396=CARTESIAN_POINT('Ctrl Pts',(-57.934536966623,-102.97983440828,173.034573714903));
#31397=CARTESIAN_POINT('Ctrl Pts',(-59.1400193036918,-102.757040708891,
173.034573766048));
#31398=CARTESIAN_POINT('Ctrl Pts',(-59.989513211636,-102.572197754367,173.898875727171));
#31399=CARTESIAN_POINT('Ctrl Pts',(-60.8390071195802,-102.387354799844,
174.763177688294));
#31400=CARTESIAN_POINT('Ctrl Pts',(-60.8290690058063,-102.29413304061,175.985485192554));
#31401=CARTESIAN_POINT('Ctrl Pts',(-60.8191308920325,-102.200911281377,
177.207792696815));
#31402=CARTESIAN_POINT('Ctrl Pts',(-59.9497607863318,-102.199310714257,
178.072094585608));
#31403=CARTESIAN_POINT('Ctrl Pts',(-59.0803906806311,-102.197710147137,
178.936396474401));
#31404=CARTESIAN_POINT('Ctrl Pts',(-57.8550322177282,-102.234060317215,
178.936396423256));
#31405=CARTESIAN_POINT('Ctrl Pts',(-56.6296737548253,-102.270410487293,
178.936396372111));
#31406=CARTESIAN_POINT('Ctrl Pts',(-55.7603037210471,-102.268809912506,
178.072094410988));
#31407=CARTESIAN_POINT('Ctrl Pts',(-54.8909336872689,-102.267209337719,
177.207792449865));
#31408=CARTESIAN_POINT('Ctrl Pts',(-54.8809956752087,-102.173987567642,
175.985484945604));
#31409=CARTESIAN_POINT('Ctrl Pts',(-54.8710576631486,-102.080765797565,
174.763177441344));
#31410=CARTESIAN_POINT('Ctrl Pts',(-55.7205516430152,-101.895922835374,
173.89887555255));
#31411=CARTESIAN_POINT('Ctrl Pts',(-56.5700456228819,-101.711079873183,
173.034573663757));
#31412=CARTESIAN_POINT('Ctrl Pts',(-57.7755279599507,-101.488286173794,
173.034573714903));
#31413=CARTESIAN_POINT('Ctrl Pts',(-58.9810102970196,-101.265492474405,
173.034573766048));
#31414=CARTESIAN_POINT('Ctrl Pts',(-59.8305042049638,-101.080649519882,
173.898875727171));
#31415=CARTESIAN_POINT('Ctrl Pts',(-60.679998112908,-100.895806565358,174.763177688294));
#31416=CARTESIAN_POINT('Ctrl Pts',(-60.6700599991341,-100.802584806125,
175.985485192554));
#31417=CARTESIAN_POINT('Ctrl Pts',(-60.6601218853602,-100.709363046891,
177.207792696815));
#31418=CARTESIAN_POINT('Ctrl Pts',(-59.7907517796595,-100.707762479771,
178.072094585608));
#31419=CARTESIAN_POINT('Ctrl Pts',(-58.9213816739588,-100.706161912651,
178.936396474401));
#31420=CARTESIAN_POINT('Ctrl Pts',(-57.696023211056,-100.742512082729,178.936396423256));
#31421=CARTESIAN_POINT('Ctrl Pts',(-56.4706647481531,-100.778862252808,
178.936396372111));
#31422=CARTESIAN_POINT('Ctrl Pts',(-55.6012947143749,-100.77726167802,178.072094410988));
#31423=CARTESIAN_POINT('Ctrl Pts',(-54.7319246805966,-100.775661103233,
177.207792449865));
#31424=CARTESIAN_POINT('Ctrl Pts',(-54.7219866685365,-100.682439333156,
175.985484945604));
#31425=CARTESIAN_POINT('Ctrl Pts',(-54.7120486564763,-100.589217563079,
174.763177441344));
#31426=CARTESIAN_POINT('Ctrl Pts',(-55.561542636343,-100.404374600888,173.89887555255));
#31427=CARTESIAN_POINT('Ctrl Pts',(-56.4110366162097,-100.219531638698,
173.034573663757));
#31428=CARTESIAN_POINT('Ctrl Pts',(-57.6165189532785,-99.9967379393085,
173.034573714903));
#31429=CARTESIAN_POINT('Ctrl Pts',(-58.8220012903473,-99.7739442399195,
173.034573766048));
#31430=CARTESIAN_POINT('Ctrl Pts',(-59.6714951982915,-99.5891012853962,
173.898875727171));
#31431=CARTESIAN_POINT('Ctrl Pts',(-60.5209891062358,-99.4042583308729,
174.763177688294));
#31432=CARTESIAN_POINT('Ctrl Pts',(-60.5110509924619,-99.3110365716392,
175.985485192554));
#31433=CARTESIAN_POINT('Ctrl Pts',(-60.501112878688,-99.2178148124055,177.207792696815));
#31434=CARTESIAN_POINT('Ctrl Pts',(-59.6317427729873,-99.2162142452855,
178.072094585608));
#31435=CARTESIAN_POINT('Ctrl Pts',(-58.7623726672866,-99.2146136781656,
178.936396474401));
#31436=CARTESIAN_POINT('Ctrl Pts',(-57.5370142043838,-99.2509638482439,
178.936396423256));
#31437=CARTESIAN_POINT('Ctrl Pts',(-56.3116557414809,-99.2873140183222,
178.936396372111));
#31438=CARTESIAN_POINT('Ctrl Pts',(-55.4422857077027,-99.2857134435348,
178.072094410988));
#31439=CARTESIAN_POINT('Ctrl Pts',(-54.5729156739244,-99.2841128687474,
177.207792449865));
#31440=CARTESIAN_POINT('Ctrl Pts',(-54.5629776618643,-99.1908910986704,
175.985484945604));
#31441=CARTESIAN_POINT('Ctrl Pts',(-54.5530396498041,-99.0976693285933,
174.763177441344));
#31442=CARTESIAN_POINT('Ctrl Pts',(-55.4025336296708,-98.9128263664026,
173.89887555255));
#31443=CARTESIAN_POINT('Ctrl Pts',(-56.2520276095374,-98.727983404212,173.034573663757));
#31444=CARTESIAN_POINT('Ctrl Pts',(-57.4575099466063,-98.5051897048229,
173.034573714903));
#31445=CARTESIAN_POINT('Ctrl Pts',(-58.6629922836751,-98.2823960054338,
173.034573766048));
#31446=CARTESIAN_POINT('Ctrl Pts',(-59.5124861916193,-98.0975530509106,
173.898875727171));
#31447=CARTESIAN_POINT('Ctrl Pts',(-60.3619800995635,-97.9127100963873,
174.763177688294));
#31448=CARTESIAN_POINT('Ctrl Pts',(-60.3520419857897,-97.8194883371536,
175.985485192554));
#31449=CARTESIAN_POINT('Ctrl Pts',(-60.3421038720158,-97.7262665779199,
177.207792696815));
#31450=CARTESIAN_POINT('Ctrl Pts',(-59.4727337663151,-97.7246660108,178.072094585608));
#31451=CARTESIAN_POINT('Ctrl Pts',(-58.6033636606144,-97.72306544368,178.936396474401));
#31452=CARTESIAN_POINT('Ctrl Pts',(-57.3780051977115,-97.7594156137583,
178.936396423256));
#31453=CARTESIAN_POINT('Ctrl Pts',(-56.1526467348087,-97.7957657838366,
178.936396372111));
#31454=CARTESIAN_POINT('Ctrl Pts',(-55.2832767010304,-97.7941652090492,
178.072094410988));
#31455=CARTESIAN_POINT('Ctrl Pts',(-56.1707879621501,-113.117200285871,
178.813917503681));
#31456=CARTESIAN_POINT('Ctrl Pts',(-54.9958760764408,-113.148172513793,
177.642342330969));
#31457=CARTESIAN_POINT('Ctrl Pts',(-54.9859380824611,-113.054950741788,
175.985484901707));
#31458=CARTESIAN_POINT('Ctrl Pts',(-54.9760000884813,-112.961728969784,
174.328627472445));
#31459=CARTESIAN_POINT('Ctrl Pts',(-56.1310359458487,-112.744313202158,
173.157052397777));
#31460=CARTESIAN_POINT('Ctrl Pts',(-57.2860718032161,-112.526897434533,
171.985477323109));
#31461=CARTESIAN_POINT('Ctrl Pts',(-58.9236555892389,-112.258038833861,
171.985477392437));
#31462=CARTESIAN_POINT('Ctrl Pts',(-60.5612393752617,-111.98918023319,171.985477461765));
#31463=CARTESIAN_POINT('Ctrl Pts',(-61.7162751351371,-111.771764475958,
173.157052634477));
#31464=CARTESIAN_POINT('Ctrl Pts',(-62.8713108950124,-111.554348718726,
174.32862780719));
#31465=CARTESIAN_POINT('Ctrl Pts',(-62.8613727631581,-111.46112696142,175.985485236452));
#31466=CARTESIAN_POINT('Ctrl Pts',(-62.8514346313038,-111.367905204114,
177.642342665714));
#31467=CARTESIAN_POINT('Ctrl Pts',(-61.6765226481024,-111.398877442428,
178.813917740382));
#31468=CARTESIAN_POINT('Ctrl Pts',(-60.501610664901,-111.429849680743,179.98549281505));
#31469=CARTESIAN_POINT('Ctrl Pts',(-58.8441507530441,-111.512264752104,
179.985492745722));
#31470=CARTESIAN_POINT('Ctrl Pts',(-57.1866908411873,-111.594679823465,
179.985492676394));
#31471=CARTESIAN_POINT('Ctrl Pts',(-56.0117789554779,-111.625652051386,
178.813917503681));
#31472=CARTESIAN_POINT('Ctrl Pts',(-54.8368670697686,-111.656624279307,
177.642342330969));
#31473=CARTESIAN_POINT('Ctrl Pts',(-54.8269290757888,-111.563402507303,
175.985484901707));
#31474=CARTESIAN_POINT('Ctrl Pts',(-54.8169910818091,-111.470180735298,
174.328627472445));
#31475=CARTESIAN_POINT('Ctrl Pts',(-55.9720269391765,-111.252764967673,
173.157052397777));
#31476=CARTESIAN_POINT('Ctrl Pts',(-57.1270627965439,-111.035349200047,
171.985477323109));
#31477=CARTESIAN_POINT('Ctrl Pts',(-58.7646465825667,-110.766490599376,
171.985477392437));
#31478=CARTESIAN_POINT('Ctrl Pts',(-60.4022303685895,-110.497631998704,
171.985477461765));
#31479=CARTESIAN_POINT('Ctrl Pts',(-61.5572661284649,-110.280216241472,
173.157052634477));
#31480=CARTESIAN_POINT('Ctrl Pts',(-62.7123018883402,-110.06280048424,174.32862780719));
#31481=CARTESIAN_POINT('Ctrl Pts',(-62.7023637564859,-109.969578726934,
175.985485236452));
#31482=CARTESIAN_POINT('Ctrl Pts',(-62.6924256246316,-109.876356969628,
177.642342665714));
#31483=CARTESIAN_POINT('Ctrl Pts',(-61.5175136414302,-109.907329207943,
178.813917740382));
#31484=CARTESIAN_POINT('Ctrl Pts',(-60.3426016582288,-109.938301446257,
179.98549281505));
#31485=CARTESIAN_POINT('Ctrl Pts',(-58.6851417463719,-110.020716517618,
179.985492745722));
#31486=CARTESIAN_POINT('Ctrl Pts',(-57.0276818345151,-110.103131588979,
179.985492676394));
#31487=CARTESIAN_POINT('Ctrl Pts',(-55.8527699488057,-110.1341038169,178.813917503681));
#31488=CARTESIAN_POINT('Ctrl Pts',(-54.6778580630964,-110.165076044821,
177.642342330969));
#31489=CARTESIAN_POINT('Ctrl Pts',(-54.6679200691166,-110.071854272817,
175.985484901707));
#31490=CARTESIAN_POINT('Ctrl Pts',(-54.6579820751369,-109.978632500812,
174.328627472445));
#31491=CARTESIAN_POINT('Ctrl Pts',(-55.8130179325043,-109.761216733187,
173.157052397777));
#31492=CARTESIAN_POINT('Ctrl Pts',(-56.9680537898716,-109.543800965562,
171.985477323109));
#31493=CARTESIAN_POINT('Ctrl Pts',(-58.6056375758945,-109.27494236489,171.985477392437));
#31494=CARTESIAN_POINT('Ctrl Pts',(-60.2432213619173,-109.006083764219,
171.985477461765));
#31495=CARTESIAN_POINT('Ctrl Pts',(-61.3982571217926,-108.788668006987,
173.157052634477));
#31496=CARTESIAN_POINT('Ctrl Pts',(-62.553292881668,-108.571252249755,174.32862780719));
#31497=CARTESIAN_POINT('Ctrl Pts',(-62.5433547498136,-108.478030492449,
175.985485236452));
#31498=CARTESIAN_POINT('Ctrl Pts',(-62.5334166179593,-108.384808735142,
177.642342665714));
#31499=CARTESIAN_POINT('Ctrl Pts',(-61.3585046347579,-108.415780973457,
178.813917740382));
#31500=CARTESIAN_POINT('Ctrl Pts',(-60.1835926515565,-108.446753211771,
179.98549281505));
#31501=CARTESIAN_POINT('Ctrl Pts',(-58.5261327396997,-108.529168283132,
179.985492745722));
#31502=CARTESIAN_POINT('Ctrl Pts',(-56.8686728278428,-108.611583354493,
179.985492676394));
#31503=CARTESIAN_POINT('Ctrl Pts',(-55.6937609421335,-108.642555582415,
178.813917503681));
#31504=CARTESIAN_POINT('Ctrl Pts',(-54.5188490564241,-108.673527810336,
177.642342330969));
#31505=CARTESIAN_POINT('Ctrl Pts',(-54.5089110624444,-108.580306038331,
175.985484901707));
#31506=CARTESIAN_POINT('Ctrl Pts',(-54.4989730684647,-108.487084266327,
174.328627472445));
#31507=CARTESIAN_POINT('Ctrl Pts',(-55.654008925832,-108.269668498702,173.157052397777));
#31508=CARTESIAN_POINT('Ctrl Pts',(-56.8090447831994,-108.052252731076,
171.985477323109));
#31509=CARTESIAN_POINT('Ctrl Pts',(-58.4466285692222,-107.783394130405,
171.985477392437));
#31510=CARTESIAN_POINT('Ctrl Pts',(-60.0842123552451,-107.514535529733,
171.985477461765));
#31511=CARTESIAN_POINT('Ctrl Pts',(-61.2392481151204,-107.297119772501,
173.157052634477));
#31512=CARTESIAN_POINT('Ctrl Pts',(-62.3942838749957,-107.079704015269,
174.32862780719));
#31513=CARTESIAN_POINT('Ctrl Pts',(-62.3843457431414,-106.986482257963,
175.985485236452));
#31514=CARTESIAN_POINT('Ctrl Pts',(-62.3744076112871,-106.893260500657,
177.642342665714));
#31515=CARTESIAN_POINT('Ctrl Pts',(-61.1994956280857,-106.924232738971,
178.813917740382));
#31516=CARTESIAN_POINT('Ctrl Pts',(-60.0245836448843,-106.955204977286,
179.98549281505));
#31517=CARTESIAN_POINT('Ctrl Pts',(-58.3671237330274,-107.037620048647,
179.985492745722));
#31518=CARTESIAN_POINT('Ctrl Pts',(-56.7096638211706,-107.120035120008,
179.985492676394));
#31519=CARTESIAN_POINT('Ctrl Pts',(-55.5347519354612,-107.151007347929,
178.813917503681));
#31520=CARTESIAN_POINT('Ctrl Pts',(-54.3598400497519,-107.18197957585,177.642342330969));
#31521=CARTESIAN_POINT('Ctrl Pts',(-54.3499020557721,-107.088757803846,
175.985484901707));
#31522=CARTESIAN_POINT('Ctrl Pts',(-54.3399640617924,-106.995536031841,
174.328627472445));
#31523=CARTESIAN_POINT('Ctrl Pts',(-55.4949999191598,-106.778120264216,
173.157052397777));
#31524=CARTESIAN_POINT('Ctrl Pts',(-56.6500357765272,-106.560704496591,
171.985477323109));
#31525=CARTESIAN_POINT('Ctrl Pts',(-58.28761956255,-106.291845895919,171.985477392437));
#31526=CARTESIAN_POINT('Ctrl Pts',(-59.9252033485729,-106.022987295247,
171.985477461765));
#31527=CARTESIAN_POINT('Ctrl Pts',(-61.0802391084482,-105.805571538015,
173.157052634477));
#31528=CARTESIAN_POINT('Ctrl Pts',(-62.2352748683235,-105.588155780784,
174.32862780719));
#31529=CARTESIAN_POINT('Ctrl Pts',(-62.2253367364692,-105.494934023477,
175.985485236452));
#31530=CARTESIAN_POINT('Ctrl Pts',(-62.2153986046149,-105.401712266171,
177.642342665714));
#31531=CARTESIAN_POINT('Ctrl Pts',(-61.0404866214135,-105.432684504486,
178.813917740382));
#31532=CARTESIAN_POINT('Ctrl Pts',(-59.8655746382121,-105.4636567428,179.98549281505));
#31533=CARTESIAN_POINT('Ctrl Pts',(-58.2081147263552,-105.546071814161,
179.985492745722));
#31534=CARTESIAN_POINT('Ctrl Pts',(-56.5506548144984,-105.628486885522,
179.985492676394));
#31535=CARTESIAN_POINT('Ctrl Pts',(-55.375742928789,-105.659459113443,178.813917503681));
#31536=CARTESIAN_POINT('Ctrl Pts',(-54.2008310430796,-105.690431341365,
177.642342330969));
#31537=CARTESIAN_POINT('Ctrl Pts',(-54.1908930490999,-105.59720956936,175.985484901707));
#31538=CARTESIAN_POINT('Ctrl Pts',(-54.1809550551202,-105.503987797356,
174.328627472445));
#31539=CARTESIAN_POINT('Ctrl Pts',(-55.3359909124876,-105.28657202973,173.157052397777));
#31540=CARTESIAN_POINT('Ctrl Pts',(-56.491026769855,-105.069156262105,171.985477323109));
#31541=CARTESIAN_POINT('Ctrl Pts',(-58.1286105558778,-104.800297661433,
171.985477392437));
#31542=CARTESIAN_POINT('Ctrl Pts',(-59.7661943419006,-104.531439060762,
171.985477461765));
#31543=CARTESIAN_POINT('Ctrl Pts',(-60.9212301017759,-104.31402330353,173.157052634477));
#31544=CARTESIAN_POINT('Ctrl Pts',(-62.0762658616513,-104.096607546298,
174.32862780719));
#31545=CARTESIAN_POINT('Ctrl Pts',(-62.066327729797,-104.003385788992,175.985485236452));
#31546=CARTESIAN_POINT('Ctrl Pts',(-62.0563895979427,-103.910164031686,
177.642342665714));
#31547=CARTESIAN_POINT('Ctrl Pts',(-60.8814776147413,-103.94113627,178.813917740382));
#31548=CARTESIAN_POINT('Ctrl Pts',(-59.7065656315398,-103.972108508315,
179.98549281505));
#31549=CARTESIAN_POINT('Ctrl Pts',(-58.049105719683,-104.054523579676,179.985492745722));
#31550=CARTESIAN_POINT('Ctrl Pts',(-56.3916458078261,-104.136938651037,
179.985492676394));
#31551=CARTESIAN_POINT('Ctrl Pts',(-55.2167339221168,-104.167910878958,
178.813917503681));
#31552=CARTESIAN_POINT('Ctrl Pts',(-54.0418220364074,-104.198883106879,
177.642342330969));
#31553=CARTESIAN_POINT('Ctrl Pts',(-54.0318840424277,-104.105661334875,
175.985484901707));
#31554=CARTESIAN_POINT('Ctrl Pts',(-54.021946048448,-104.01243956287,174.328627472445));
#31555=CARTESIAN_POINT('Ctrl Pts',(-55.1769819058153,-103.795023795245,
173.157052397777));
#31556=CARTESIAN_POINT('Ctrl Pts',(-56.3320177631827,-103.577608027619,
171.985477323109));
#31557=CARTESIAN_POINT('Ctrl Pts',(-57.9696015492056,-103.308749426948,
171.985477392437));
#31558=CARTESIAN_POINT('Ctrl Pts',(-59.6071853352284,-103.039890826276,
171.985477461765));
#31559=CARTESIAN_POINT('Ctrl Pts',(-60.7622210951037,-102.822475069044,
173.157052634477));
#31560=CARTESIAN_POINT('Ctrl Pts',(-61.9172568549791,-102.605059311812,
174.32862780719));
#31561=CARTESIAN_POINT('Ctrl Pts',(-61.9073187231247,-102.511837554506,
175.985485236452));
#31562=CARTESIAN_POINT('Ctrl Pts',(-61.8973805912704,-102.4186157972,177.642342665714));
#31563=CARTESIAN_POINT('Ctrl Pts',(-60.722468608069,-102.449588035515,178.813917740382));
#31564=CARTESIAN_POINT('Ctrl Pts',(-59.5475566248676,-102.480560273829,
179.98549281505));
#31565=CARTESIAN_POINT('Ctrl Pts',(-57.8900967130108,-102.56297534519,179.985492745722));
#31566=CARTESIAN_POINT('Ctrl Pts',(-56.2326368011539,-102.645390416551,
179.985492676394));
#31567=CARTESIAN_POINT('Ctrl Pts',(-55.0577249154445,-102.676362644472,
178.813917503681));
#31568=CARTESIAN_POINT('Ctrl Pts',(-53.8828130297352,-102.707334872393,
177.642342330969));
#31569=CARTESIAN_POINT('Ctrl Pts',(-53.8728750357555,-102.614113100389,
175.985484901707));
#31570=CARTESIAN_POINT('Ctrl Pts',(-53.8629370417758,-102.520891328384,
174.328627472445));
#31571=CARTESIAN_POINT('Ctrl Pts',(-55.0179728991431,-102.303475560759,
173.157052397777));
#31572=CARTESIAN_POINT('Ctrl Pts',(-56.1730087565105,-102.086059793134,
171.985477323109));
#31573=CARTESIAN_POINT('Ctrl Pts',(-57.8105925425333,-101.817201192462,
171.985477392437));
#31574=CARTESIAN_POINT('Ctrl Pts',(-59.4481763285562,-101.548342591791,
171.985477461765));
#31575=CARTESIAN_POINT('Ctrl Pts',(-60.6032120884315,-101.330926834559,
173.157052634477));
#31576=CARTESIAN_POINT('Ctrl Pts',(-61.7582478483068,-101.113511077327,
174.32862780719));
#31577=CARTESIAN_POINT('Ctrl Pts',(-61.7483097164525,-101.020289320021,
175.985485236452));
#31578=CARTESIAN_POINT('Ctrl Pts',(-61.7383715845982,-100.927067562714,
177.642342665714));
#31579=CARTESIAN_POINT('Ctrl Pts',(-60.5634596013968,-100.958039801029,
178.813917740382));
#31580=CARTESIAN_POINT('Ctrl Pts',(-59.3885476181954,-100.989012039343,
179.98549281505));
#31581=CARTESIAN_POINT('Ctrl Pts',(-57.7310877063385,-101.071427110704,
179.985492745722));
#31582=CARTESIAN_POINT('Ctrl Pts',(-56.0736277944817,-101.153842182065,
179.985492676394));
#31583=CARTESIAN_POINT('Ctrl Pts',(-54.8987159087723,-101.184814409987,
178.813917503681));
#31584=CARTESIAN_POINT('Ctrl Pts',(-53.723804023063,-101.215786637908,177.642342330969));
#31585=CARTESIAN_POINT('Ctrl Pts',(-53.7138660290832,-101.122564865903,
175.985484901707));
#31586=CARTESIAN_POINT('Ctrl Pts',(-53.7039280351035,-101.029343093899,
174.328627472445));
#31587=CARTESIAN_POINT('Ctrl Pts',(-54.8589638924709,-100.811927326274,
173.157052397777));
#31588=CARTESIAN_POINT('Ctrl Pts',(-56.0139997498383,-100.594511558648,
171.985477323109));
#31589=CARTESIAN_POINT('Ctrl Pts',(-57.6515835358611,-100.325652957977,
171.985477392437));
#31590=CARTESIAN_POINT('Ctrl Pts',(-59.2891673218839,-100.056794357305,
171.985477461765));
#31591=CARTESIAN_POINT('Ctrl Pts',(-60.4442030817593,-99.8393786000731,
173.157052634477));
#31592=CARTESIAN_POINT('Ctrl Pts',(-61.5992388416346,-99.6219628428411,
174.32862780719));
#31593=CARTESIAN_POINT('Ctrl Pts',(-61.5893007097803,-99.5287410855349,
175.985485236452));
#31594=CARTESIAN_POINT('Ctrl Pts',(-61.579362577926,-99.4355193282287,177.642342665714));
#31595=CARTESIAN_POINT('Ctrl Pts',(-60.4044505947246,-99.4664915665433,
178.813917740382));
#31596=CARTESIAN_POINT('Ctrl Pts',(-59.2295386115232,-99.4974638048579,
179.98549281505));
#31597=CARTESIAN_POINT('Ctrl Pts',(-57.5720786996663,-99.5798788762188,
179.985492745722));
#31598=CARTESIAN_POINT('Ctrl Pts',(-55.9146187878095,-99.6622939475797,
179.985492676394));
#31599=CARTESIAN_POINT('Ctrl Pts',(-54.7397069021001,-99.693266175501,178.813917503681));
#31600=CARTESIAN_POINT('Ctrl Pts',(-53.5647950163907,-99.7242384034223,
177.642342330969));
#31601=CARTESIAN_POINT('Ctrl Pts',(-53.554857022411,-99.6310166314178,175.985484901707));
#31602=CARTESIAN_POINT('Ctrl Pts',(-53.5449190284313,-99.5377948594132,
174.328627472445));
#31603=CARTESIAN_POINT('Ctrl Pts',(-54.6999548857987,-99.3203790917879,
173.157052397777));
#31604=CARTESIAN_POINT('Ctrl Pts',(-55.854990743166,-99.1029633241627,171.985477323109));
#31605=CARTESIAN_POINT('Ctrl Pts',(-57.4925745291889,-98.8341047234911,
171.985477392437));
#31606=CARTESIAN_POINT('Ctrl Pts',(-59.1301583152117,-98.5652461228194,
171.985477461765));
#31607=CARTESIAN_POINT('Ctrl Pts',(-60.285194075087,-98.3478303655875,173.157052634477));
#31608=CARTESIAN_POINT('Ctrl Pts',(-61.4402298349624,-98.1304146083555,
174.32862780719));
#31609=CARTESIAN_POINT('Ctrl Pts',(-61.430291703108,-98.0371928510493,175.985485236452));
#31610=CARTESIAN_POINT('Ctrl Pts',(-61.4203535712537,-97.9439710937432,
177.642342665714));
#31611=CARTESIAN_POINT('Ctrl Pts',(-60.2454415880523,-97.9749433320577,
178.813917740382));
#31612=CARTESIAN_POINT('Ctrl Pts',(-59.0705296048509,-98.0059155703723,
179.98549281505));
#31613=CARTESIAN_POINT('Ctrl Pts',(-57.4130696929941,-98.0883306417332,
179.985492745722));
#31614=CARTESIAN_POINT('Ctrl Pts',(-55.7556097811372,-98.1707457130942,
179.985492676394));
#31615=CARTESIAN_POINT('Ctrl Pts',(-54.5806978954278,-98.2017179410154,
178.813917503681));
#31616=CARTESIAN_POINT('Ctrl Pts',(-60.8888270505345,-111.922827698136,
172.515418850865));
#31617=CARTESIAN_POINT('Ctrl Pts',(-61.3449147819398,-111.841663883713,
172.780385782991));
#31618=CARTESIAN_POINT('Ctrl Pts',(-61.7162694809355,-111.771762644582,
173.157058062683));
#31619=CARTESIAN_POINT('Ctrl Pts',(-61.8701645018886,-111.74279451064,173.313156769748));
#31620=CARTESIAN_POINT('Ctrl Pts',(-62.0059837058594,-111.715257081458,
173.485485069079));
#31621=CARTESIAN_POINT('Ctrl Pts',(-56.1707931031902,-113.117197303651,
178.813912075476));
#31622=CARTESIAN_POINT('Ctrl Pts',(-54.9958834532485,-113.148169293224,
177.6423391512));
#31623=CARTESIAN_POINT('Ctrl Pts',(-54.9859454592686,-113.05494752122,175.985484901707));
#31624=CARTESIAN_POINT('Ctrl Pts',(-54.9760074652888,-112.961725749215,
174.328630652215));
#31625=CARTESIAN_POINT('Ctrl Pts',(-56.1310410868884,-112.744310219938,
173.157057825983));
#31626=CARTESIAN_POINT('Ctrl Pts',(-57.286074708488,-112.52689469066,171.985484999752));
#31627=CARTESIAN_POINT('Ctrl Pts',(-58.9236553326578,-112.258036427063,
171.985485069079));
#31628=CARTESIAN_POINT('Ctrl Pts',(-60.5612359568277,-111.989178163466,
171.985485138407));
#31629=CARTESIAN_POINT('Ctrl Pts',(-61.7162694809355,-111.771762644582,
173.157058062683));
#31630=CARTESIAN_POINT('Ctrl Pts',(-62.8713030050432,-111.554347125698,
174.328630986959));
#31631=CARTESIAN_POINT('Ctrl Pts',(-62.861364873189,-111.461125368392,175.985485236451));
#31632=CARTESIAN_POINT('Ctrl Pts',(-62.8514267413349,-111.367903611086,
177.642339485944));
#31633=CARTESIAN_POINT('Ctrl Pts',(-61.6765169939012,-111.398875611052,
178.813912312176));
#31634=CARTESIAN_POINT('Ctrl Pts',(-60.5016072464676,-111.429847611019,
179.985485138407));
#31635=CARTESIAN_POINT('Ctrl Pts',(-58.8441504964637,-111.512262345305,
179.985485069079));
#31636=CARTESIAN_POINT('Ctrl Pts',(-57.1866937464598,-111.594677079592,
179.985484999752));
#31637=CARTESIAN_POINT('Ctrl Pts',(-56.011784096518,-111.625649069165,178.813912075476));
#31638=CARTESIAN_POINT('Ctrl Pts',(-54.8368744465763,-111.656621058739,
177.6423391512));
#31639=CARTESIAN_POINT('Ctrl Pts',(-54.8269364525964,-111.563399286734,
175.985484901707));
#31640=CARTESIAN_POINT('Ctrl Pts',(-54.8169984586165,-111.47017751473,174.328630652215));
#31641=CARTESIAN_POINT('Ctrl Pts',(-55.9720320802161,-111.252761985452,
173.157057825983));
#31642=CARTESIAN_POINT('Ctrl Pts',(-57.1270657018158,-111.035346456175,
171.985484999752));
#31643=CARTESIAN_POINT('Ctrl Pts',(-58.7646463259856,-110.766488192578,
171.985485069079));
#31644=CARTESIAN_POINT('Ctrl Pts',(-60.4022269501555,-110.497629928981,
171.985485138407));
#31645=CARTESIAN_POINT('Ctrl Pts',(-61.5572604742632,-110.280214410097,
173.157058062683));
#31646=CARTESIAN_POINT('Ctrl Pts',(-62.712293998371,-110.062798891212,174.328630986959));
#31647=CARTESIAN_POINT('Ctrl Pts',(-62.7023558665168,-109.969577133906,
175.985485236451));
#31648=CARTESIAN_POINT('Ctrl Pts',(-62.6924177346626,-109.8763553766,177.642339485944));
#31649=CARTESIAN_POINT('Ctrl Pts',(-61.517507987229,-109.907327376567,178.813912312176));
#31650=CARTESIAN_POINT('Ctrl Pts',(-60.3425982397954,-109.938299376534,
179.985485138407));
#31651=CARTESIAN_POINT('Ctrl Pts',(-58.6851414897915,-110.02071411082,179.985485069079));
#31652=CARTESIAN_POINT('Ctrl Pts',(-57.0276847397876,-110.103128845106,
179.985484999752));
#31653=CARTESIAN_POINT('Ctrl Pts',(-55.8527750898458,-110.13410083468,178.813912075476));
#31654=CARTESIAN_POINT('Ctrl Pts',(-54.677865439904,-110.165072824253,177.6423391512));
#31655=CARTESIAN_POINT('Ctrl Pts',(-54.6679274459242,-110.071851052249,
175.985484901707));
#31656=CARTESIAN_POINT('Ctrl Pts',(-54.6579894519443,-109.978629280244,
174.328630652215));
#31657=CARTESIAN_POINT('Ctrl Pts',(-55.8130230735439,-109.761213750967,
173.157057825983));
#31658=CARTESIAN_POINT('Ctrl Pts',(-56.9680566951435,-109.543798221689,
171.985484999752));
#31659=CARTESIAN_POINT('Ctrl Pts',(-58.6056373193134,-109.274939958092,
171.985485069079));
#31660=CARTESIAN_POINT('Ctrl Pts',(-60.2432179434833,-109.006081694495,
171.985485138407));
#31661=CARTESIAN_POINT('Ctrl Pts',(-61.398251467591,-108.788666175611,173.157058062683));
#31662=CARTESIAN_POINT('Ctrl Pts',(-62.5532849916988,-108.571250656727,
174.328630986959));
#31663=CARTESIAN_POINT('Ctrl Pts',(-62.5433468598446,-108.478028899421,
175.985485236451));
#31664=CARTESIAN_POINT('Ctrl Pts',(-62.5334087279904,-108.384807142114,
177.642339485944));
#31665=CARTESIAN_POINT('Ctrl Pts',(-61.3584989805568,-108.415779142081,
178.813912312176));
#31666=CARTESIAN_POINT('Ctrl Pts',(-60.1835892331231,-108.446751142048,
179.985485138407));
#31667=CARTESIAN_POINT('Ctrl Pts',(-58.5261324831192,-108.529165876334,
179.985485069079));
#31668=CARTESIAN_POINT('Ctrl Pts',(-56.8686757331153,-108.611580610621,
179.985484999752));
#31669=CARTESIAN_POINT('Ctrl Pts',(-55.6937660831736,-108.642552600194,
178.813912075476));
#31670=CARTESIAN_POINT('Ctrl Pts',(-54.5188564332318,-108.673524589768,
177.6423391512));
#31671=CARTESIAN_POINT('Ctrl Pts',(-54.5089184392519,-108.580302817763,
175.985484901707));
#31672=CARTESIAN_POINT('Ctrl Pts',(-54.4989804452721,-108.487081045759,
174.328630652215));
#31673=CARTESIAN_POINT('Ctrl Pts',(-55.6540140668717,-108.269665516481,
173.157057825983));
#31674=CARTESIAN_POINT('Ctrl Pts',(-56.8090476884713,-108.052249987204,
171.985484999752));
#31675=CARTESIAN_POINT('Ctrl Pts',(-58.4466283126412,-107.783391723607,
171.985485069079));
#31676=CARTESIAN_POINT('Ctrl Pts',(-60.084208936811,-107.51453346001,171.985485138407));
#31677=CARTESIAN_POINT('Ctrl Pts',(-61.2392424609188,-107.297117941125,
173.157058062683));
#31678=CARTESIAN_POINT('Ctrl Pts',(-62.3942759850265,-107.079702422241,
174.328630986959));
#31679=CARTESIAN_POINT('Ctrl Pts',(-62.3843378531723,-106.986480664935,
175.985485236451));
#31680=CARTESIAN_POINT('Ctrl Pts',(-62.3743997213182,-106.893258907629,
177.642339485944));
#31681=CARTESIAN_POINT('Ctrl Pts',(-61.1994899738845,-106.924230907596,
178.813912312176));
#31682=CARTESIAN_POINT('Ctrl Pts',(-60.0245802264509,-106.955202907562,
179.985485138407));
#31683=CARTESIAN_POINT('Ctrl Pts',(-58.367123476447,-107.037617641849,179.985485069079));
#31684=CARTESIAN_POINT('Ctrl Pts',(-56.7096667264431,-107.120032376135,
179.985484999752));
#31685=CARTESIAN_POINT('Ctrl Pts',(-55.5347570765013,-107.151004365708,
178.813912075476));
#31686=CARTESIAN_POINT('Ctrl Pts',(-54.3598474265596,-107.181976355282,
177.6423391512));
#31687=CARTESIAN_POINT('Ctrl Pts',(-54.3499094325797,-107.088754583277,
175.985484901707));
#31688=CARTESIAN_POINT('Ctrl Pts',(-54.3399714385998,-106.995532811273,
174.328630652215));
#31689=CARTESIAN_POINT('Ctrl Pts',(-55.4950050601995,-106.778117281995,
173.157057825983));
#31690=CARTESIAN_POINT('Ctrl Pts',(-56.6500386817991,-106.560701752718,
171.985484999752));
#31691=CARTESIAN_POINT('Ctrl Pts',(-58.2876193059689,-106.291843489121,
171.985485069079));
#31692=CARTESIAN_POINT('Ctrl Pts',(-59.9251999301388,-106.022985225524,
171.985485138407));
#31693=CARTESIAN_POINT('Ctrl Pts',(-61.0802334542465,-105.80556970664,173.157058062683));
#31694=CARTESIAN_POINT('Ctrl Pts',(-62.2352669783543,-105.588154187756,
174.328630986959));
#31695=CARTESIAN_POINT('Ctrl Pts',(-62.2253288465001,-105.494932430449,
175.985485236451));
#31696=CARTESIAN_POINT('Ctrl Pts',(-62.2153907146459,-105.401710673143,
177.642339485944));
#31697=CARTESIAN_POINT('Ctrl Pts',(-61.0404809672123,-105.43268267311,178.813912312176));
#31698=CARTESIAN_POINT('Ctrl Pts',(-59.8655712197787,-105.463654673077,
179.985485138407));
#31699=CARTESIAN_POINT('Ctrl Pts',(-58.2081144697748,-105.546069407363,
179.985485069079));
#31700=CARTESIAN_POINT('Ctrl Pts',(-56.5506577197709,-105.628484141649,
179.985484999752));
#31701=CARTESIAN_POINT('Ctrl Pts',(-55.3757480698291,-105.659456131223,
178.813912075476));
#31702=CARTESIAN_POINT('Ctrl Pts',(-54.2008384198873,-105.690428120796,
177.6423391512));
#31703=CARTESIAN_POINT('Ctrl Pts',(-54.1909004259075,-105.597206348792,
175.985484901707));
#31704=CARTESIAN_POINT('Ctrl Pts',(-54.1809624319276,-105.503984576787,
174.328630652215));
#31705=CARTESIAN_POINT('Ctrl Pts',(-55.3359960535272,-105.28656904751,173.157057825983));
#31706=CARTESIAN_POINT('Ctrl Pts',(-56.4910296751268,-105.069153518232,
171.985484999752));
#31707=CARTESIAN_POINT('Ctrl Pts',(-58.1286102992967,-104.800295254635,
171.985485069079));
#31708=CARTESIAN_POINT('Ctrl Pts',(-59.7661909234666,-104.531436991038,
171.985485138407));
#31709=CARTESIAN_POINT('Ctrl Pts',(-60.9212244475743,-104.314021472154,
173.157058062683));
#31710=CARTESIAN_POINT('Ctrl Pts',(-62.0762579716821,-104.09660595327,174.328630986959));
#31711=CARTESIAN_POINT('Ctrl Pts',(-62.0663198398279,-104.003384195964,
175.985485236451));
#31712=CARTESIAN_POINT('Ctrl Pts',(-62.0563817079737,-103.910162438658,
177.642339485944));
#31713=CARTESIAN_POINT('Ctrl Pts',(-60.8814719605401,-103.941134438624,
178.813912312176));
#31714=CARTESIAN_POINT('Ctrl Pts',(-59.7065622131064,-103.972106438591,
179.985485138407));
#31715=CARTESIAN_POINT('Ctrl Pts',(-58.0491054631025,-104.054521172878,
179.985485069079));
#31716=CARTESIAN_POINT('Ctrl Pts',(-56.3916487130987,-104.136935907164,
179.985484999752));
#31717=CARTESIAN_POINT('Ctrl Pts',(-55.2167390631569,-104.167907896737,
178.813912075476));
#31718=CARTESIAN_POINT('Ctrl Pts',(-54.0418294132151,-104.198879886311,
177.6423391512));
#31719=CARTESIAN_POINT('Ctrl Pts',(-54.0318914192353,-104.105658114306,
175.985484901707));
#31720=CARTESIAN_POINT('Ctrl Pts',(-54.0219534252554,-104.012436342302,
174.328630652215));
#31721=CARTESIAN_POINT('Ctrl Pts',(-55.176987046855,-103.795020813024,173.157057825983));
#31722=CARTESIAN_POINT('Ctrl Pts',(-56.3320206684546,-103.577605283747,
171.985484999752));
#31723=CARTESIAN_POINT('Ctrl Pts',(-57.9696012926245,-103.30874702015,171.985485069079));
#31724=CARTESIAN_POINT('Ctrl Pts',(-59.6071819167943,-103.039888756553,
171.985485138407));
#31725=CARTESIAN_POINT('Ctrl Pts',(-60.7622154409021,-102.822473237669,
173.157058062683));
#31726=CARTESIAN_POINT('Ctrl Pts',(-61.9172489650099,-102.605057718784,
174.328630986959));
#31727=CARTESIAN_POINT('Ctrl Pts',(-61.9073108331557,-102.511835961478,
175.985485236451));
#31728=CARTESIAN_POINT('Ctrl Pts',(-61.8973727013015,-102.418614204172,
177.642339485944));
#31729=CARTESIAN_POINT('Ctrl Pts',(-60.7224629538678,-102.449586204139,
178.813912312176));
#31730=CARTESIAN_POINT('Ctrl Pts',(-59.5475532064342,-102.480558204106,
179.985485138407));
#31731=CARTESIAN_POINT('Ctrl Pts',(-57.8900964564303,-102.562972938392,
179.985485069079));
#31732=CARTESIAN_POINT('Ctrl Pts',(-56.2326397064264,-102.645387672678,
179.985484999752));
#31733=CARTESIAN_POINT('Ctrl Pts',(-55.0577300564847,-102.676359662252,
178.813912075476));
#31734=CARTESIAN_POINT('Ctrl Pts',(-53.8828204065429,-102.707331651825,
177.6423391512));
#31735=CARTESIAN_POINT('Ctrl Pts',(-53.872882412563,-102.614109879821,175.985484901707));
#31736=CARTESIAN_POINT('Ctrl Pts',(-53.8629444185832,-102.520888107816,
174.328630652215));
#31737=CARTESIAN_POINT('Ctrl Pts',(-55.0179780401828,-102.303472578539,
173.157057825983));
#31738=CARTESIAN_POINT('Ctrl Pts',(-56.1730116617824,-102.086057049261,
171.985484999752));
#31739=CARTESIAN_POINT('Ctrl Pts',(-57.8105922859523,-101.817198785664,
171.985485069079));
#31740=CARTESIAN_POINT('Ctrl Pts',(-59.4481729101221,-101.548340522067,
171.985485138407));
#31741=CARTESIAN_POINT('Ctrl Pts',(-60.6032064342299,-101.330925003183,
173.157058062683));
#31742=CARTESIAN_POINT('Ctrl Pts',(-61.7582399583376,-101.113509484299,
174.328630986959));
#31743=CARTESIAN_POINT('Ctrl Pts',(-61.7483018264834,-101.020287726993,
175.985485236451));
#31744=CARTESIAN_POINT('Ctrl Pts',(-61.7383636946293,-100.927065969686,
177.642339485944));
#31745=CARTESIAN_POINT('Ctrl Pts',(-60.5634539471956,-100.958037969653,
178.813912312176));
#31746=CARTESIAN_POINT('Ctrl Pts',(-59.388544199762,-100.98900996962,179.985485138407));
#31747=CARTESIAN_POINT('Ctrl Pts',(-57.7310874497581,-101.071424703906,
179.985485069079));
#31748=CARTESIAN_POINT('Ctrl Pts',(-56.0736306997542,-101.153839438193,
179.985484999752));
#31749=CARTESIAN_POINT('Ctrl Pts',(-54.8987210498124,-101.184811427766,
178.813912075476));
#31750=CARTESIAN_POINT('Ctrl Pts',(-53.7238113998707,-101.21578341734,177.6423391512));
#31751=CARTESIAN_POINT('Ctrl Pts',(-53.7138734058908,-101.122561645335,
175.985484901707));
#31752=CARTESIAN_POINT('Ctrl Pts',(-53.7039354119109,-101.029339873331,
174.328630652215));
#31753=CARTESIAN_POINT('Ctrl Pts',(-54.8589690335105,-100.811924344053,
173.157057825983));
#31754=CARTESIAN_POINT('Ctrl Pts',(-56.0140026551102,-100.594508814776,
171.985484999752));
#31755=CARTESIAN_POINT('Ctrl Pts',(-57.65158327928,-100.325650551179,171.985485069079));
#31756=CARTESIAN_POINT('Ctrl Pts',(-59.2891639034499,-100.056792287582,
171.985485138407));
#31757=CARTESIAN_POINT('Ctrl Pts',(-60.4441974275576,-99.8393767686974,
173.157058062683));
#31758=CARTESIAN_POINT('Ctrl Pts',(-61.5992309516654,-99.6219612498133,
174.328630986959));
#31759=CARTESIAN_POINT('Ctrl Pts',(-61.5892928198112,-99.528739492507,175.985485236451));
#31760=CARTESIAN_POINT('Ctrl Pts',(-61.579354687957,-99.4355177352008,177.642339485944));
#31761=CARTESIAN_POINT('Ctrl Pts',(-60.4044449405234,-99.4664897351676,
178.813912312176));
#31762=CARTESIAN_POINT('Ctrl Pts',(-59.2295351930898,-99.4974617351344,
179.985485138407));
#31763=CARTESIAN_POINT('Ctrl Pts',(-57.5720784430859,-99.5798764694207,
179.985485069079));
#31764=CARTESIAN_POINT('Ctrl Pts',(-55.914621693082,-99.662291203707,179.985484999752));
#31765=CARTESIAN_POINT('Ctrl Pts',(-54.7397120431402,-99.6932631932805,
178.813912075476));
#31766=CARTESIAN_POINT('Ctrl Pts',(-53.5648023931984,-99.724235182854,177.6423391512));
#31767=CARTESIAN_POINT('Ctrl Pts',(-53.5548643992186,-99.6310134108495,
175.985484901707));
#31768=CARTESIAN_POINT('Ctrl Pts',(-53.5449264052387,-99.5377916388449,
174.328630652215));
#31769=CARTESIAN_POINT('Ctrl Pts',(-54.6999600268383,-99.3203761095675,
173.157057825983));
#31770=CARTESIAN_POINT('Ctrl Pts',(-55.8549936484379,-99.10296058029,171.985484999752));
#31771=CARTESIAN_POINT('Ctrl Pts',(-57.4925742726078,-98.834102316693,171.985485069079));
#31772=CARTESIAN_POINT('Ctrl Pts',(-59.1301548967777,-98.5652440530961,
171.985485138407));
#31773=CARTESIAN_POINT('Ctrl Pts',(-60.2851884208854,-98.3478285342118,
173.157058062683));
#31774=CARTESIAN_POINT('Ctrl Pts',(-61.4402219449932,-98.1304130153276,
174.328630986959));
#31775=CARTESIAN_POINT('Ctrl Pts',(-61.430283813139,-98.0371912580215,175.985485236451));
#31776=CARTESIAN_POINT('Ctrl Pts',(-61.4203456812848,-97.9439695007152,
177.642339485944));
#31777=CARTESIAN_POINT('Ctrl Pts',(-60.2454359338512,-97.974941500682,178.813912312176));
#31778=CARTESIAN_POINT('Ctrl Pts',(-59.0705261864175,-98.0059135006488,
179.985485138407));
#31779=CARTESIAN_POINT('Ctrl Pts',(-57.4130694364136,-98.0883282349351,
179.985485069079));
#31780=CARTESIAN_POINT('Ctrl Pts',(-55.7556126864097,-98.1707429692214,
179.985484999752));
#31781=CARTESIAN_POINT('Ctrl Pts',(-54.580703036468,-98.2017149587949,178.813912075476));
#31782=CARTESIAN_POINT('Ctrl Pts',(-56.181115489574,-113.283598570176,178.821287383467));
#31783=CARTESIAN_POINT('Ctrl Pts',(-55.0031681001975,-113.314894403068,
177.646659506339));
#31784=CARTESIAN_POINT('Ctrl Pts',(-54.9932301063974,-113.221672631044,
175.985484901271));
#31785=CARTESIAN_POINT('Ctrl Pts',(-54.9832921125973,-113.12845085902,174.324310296203));
#31786=CARTESIAN_POINT('Ctrl Pts',(-56.1413634738858,-112.910711486397,
173.149682517375));
#31787=CARTESIAN_POINT('Ctrl Pts',(-57.2994348351743,-112.692972113774,
171.975054738546));
#31788=CARTESIAN_POINT('Ctrl Pts',(-58.9413114718314,-112.423655866545,
171.975054808055));
#31789=CARTESIAN_POINT('Ctrl Pts',(-60.5831881084886,-112.154339619316,
171.975054877564));
#31790=CARTESIAN_POINT('Ctrl Pts',(-61.741259372031,-111.936600257113,173.149682754692));
#31791=CARTESIAN_POINT('Ctrl Pts',(-62.8993306355734,-111.71886089491,174.32431063182));
#31792=CARTESIAN_POINT('Ctrl Pts',(-62.8893925035395,-111.625639137623,
175.985485236888));
#31793=CARTESIAN_POINT('Ctrl Pts',(-62.8794543715055,-111.532417380336,
177.646659841956));
#31794=CARTESIAN_POINT('Ctrl Pts',(-61.701506884383,-111.563713223648,178.821287620784));
#31795=CARTESIAN_POINT('Ctrl Pts',(-60.5235593972605,-111.595009066961,
179.995915399612));
#31796=CARTESIAN_POINT('Ctrl Pts',(-58.8618066347693,-111.677881784879,
179.995915330104));
#31797=CARTESIAN_POINT('Ctrl Pts',(-57.2000538722782,-111.760754502798,
179.995915260595));
#31798=CARTESIAN_POINT('Ctrl Pts',(-56.0221064829017,-111.79205033569,178.821287383467));
#31799=CARTESIAN_POINT('Ctrl Pts',(-54.8441590935253,-111.823346168582,
177.646659506339));
#31800=CARTESIAN_POINT('Ctrl Pts',(-54.8342210997252,-111.730124396559,
175.985484901271));
#31801=CARTESIAN_POINT('Ctrl Pts',(-54.8242831059251,-111.636902624535,
174.324310296203));
#31802=CARTESIAN_POINT('Ctrl Pts',(-55.9823544672136,-111.419163251912,
173.149682517375));
#31803=CARTESIAN_POINT('Ctrl Pts',(-57.1404258285021,-111.201423879289,
171.975054738546));
#31804=CARTESIAN_POINT('Ctrl Pts',(-58.7823024651592,-110.932107632059,
171.975054808055));
#31805=CARTESIAN_POINT('Ctrl Pts',(-60.4241791018163,-110.66279138483,171.975054877564));
#31806=CARTESIAN_POINT('Ctrl Pts',(-61.5822503653587,-110.445052022627,
173.149682754692));
#31807=CARTESIAN_POINT('Ctrl Pts',(-62.7403216289012,-110.227312660424,
174.32431063182));
#31808=CARTESIAN_POINT('Ctrl Pts',(-62.7303834968672,-110.134090903137,
175.985485236888));
#31809=CARTESIAN_POINT('Ctrl Pts',(-62.7204453648333,-110.04086914585,177.646659841956));
#31810=CARTESIAN_POINT('Ctrl Pts',(-61.5424978777108,-110.072164989163,
178.821287620784));
#31811=CARTESIAN_POINT('Ctrl Pts',(-60.3645503905882,-110.103460832475,
179.995915399612));
#31812=CARTESIAN_POINT('Ctrl Pts',(-58.7027976280971,-110.186333550394,
179.995915330104));
#31813=CARTESIAN_POINT('Ctrl Pts',(-57.041044865606,-110.269206268313,179.995915260595));
#31814=CARTESIAN_POINT('Ctrl Pts',(-55.8630974762295,-110.300502101205,
178.821287383467));
#31815=CARTESIAN_POINT('Ctrl Pts',(-54.6851500868531,-110.331797934097,
177.646659506339));
#31816=CARTESIAN_POINT('Ctrl Pts',(-54.675212093053,-110.238576162073,175.985484901271));
#31817=CARTESIAN_POINT('Ctrl Pts',(-54.6652740992529,-110.145354390049,
174.324310296203));
#31818=CARTESIAN_POINT('Ctrl Pts',(-55.8233454605414,-109.927615017426,
173.149682517375));
#31819=CARTESIAN_POINT('Ctrl Pts',(-56.9814168218299,-109.709875644803,
171.975054738546));
#31820=CARTESIAN_POINT('Ctrl Pts',(-58.623293458487,-109.440559397574,171.975054808055));
#31821=CARTESIAN_POINT('Ctrl Pts',(-60.2651700951441,-109.171243150344,
171.975054877564));
#31822=CARTESIAN_POINT('Ctrl Pts',(-61.4232413586865,-108.953503788142,
173.149682754692));
#31823=CARTESIAN_POINT('Ctrl Pts',(-62.581312622229,-108.735764425939,174.32431063182));
#31824=CARTESIAN_POINT('Ctrl Pts',(-62.571374490195,-108.642542668652,175.985485236888));
#31825=CARTESIAN_POINT('Ctrl Pts',(-62.5614363581611,-108.549320911365,
177.646659841956));
#31826=CARTESIAN_POINT('Ctrl Pts',(-61.3834888710385,-108.580616754677,
178.821287620784));
#31827=CARTESIAN_POINT('Ctrl Pts',(-60.205541383916,-108.61191259799,179.995915399612));
#31828=CARTESIAN_POINT('Ctrl Pts',(-58.5437886214249,-108.694785315908,
179.995915330104));
#31829=CARTESIAN_POINT('Ctrl Pts',(-56.8820358589338,-108.777658033827,
179.995915260595));
#31830=CARTESIAN_POINT('Ctrl Pts',(-55.7040884695573,-108.808953866719,
178.821287383467));
#31831=CARTESIAN_POINT('Ctrl Pts',(-54.5261410801808,-108.840249699611,
177.646659506339));
#31832=CARTESIAN_POINT('Ctrl Pts',(-54.5162030863807,-108.747027927587,
175.985484901271));
#31833=CARTESIAN_POINT('Ctrl Pts',(-54.5062650925806,-108.653806155564,
174.324310296203));
#31834=CARTESIAN_POINT('Ctrl Pts',(-55.6643364538691,-108.436066782941,
173.149682517375));
#31835=CARTESIAN_POINT('Ctrl Pts',(-56.8224078151577,-108.218327410317,
171.975054738546));
#31836=CARTESIAN_POINT('Ctrl Pts',(-58.4642844518147,-107.949011163088,
171.975054808055));
#31837=CARTESIAN_POINT('Ctrl Pts',(-60.1061610884719,-107.679694915859,
171.975054877564));
#31838=CARTESIAN_POINT('Ctrl Pts',(-61.2642323520143,-107.461955553656,
173.149682754692));
#31839=CARTESIAN_POINT('Ctrl Pts',(-62.4223036155567,-107.244216191453,
174.32431063182));
#31840=CARTESIAN_POINT('Ctrl Pts',(-62.4123654835228,-107.150994434166,
175.985485236888));
#31841=CARTESIAN_POINT('Ctrl Pts',(-62.4024273514889,-107.057772676879,
177.646659841956));
#31842=CARTESIAN_POINT('Ctrl Pts',(-61.2244798643663,-107.089068520192,
178.821287620784));
#31843=CARTESIAN_POINT('Ctrl Pts',(-60.0465323772438,-107.120364363504,
179.995915399612));
#31844=CARTESIAN_POINT('Ctrl Pts',(-58.3847796147526,-107.203237081423,
179.995915330104));
#31845=CARTESIAN_POINT('Ctrl Pts',(-56.7230268522615,-107.286109799341,
179.995915260595));
#31846=CARTESIAN_POINT('Ctrl Pts',(-55.5450794628851,-107.317405632233,
178.821287383467));
#31847=CARTESIAN_POINT('Ctrl Pts',(-54.3671320735086,-107.348701465125,
177.646659506339));
#31848=CARTESIAN_POINT('Ctrl Pts',(-54.3571940797085,-107.255479693102,
175.985484901271));
#31849=CARTESIAN_POINT('Ctrl Pts',(-54.3472560859084,-107.162257921078,
174.324310296203));
#31850=CARTESIAN_POINT('Ctrl Pts',(-55.5053274471969,-106.944518548455,
173.149682517375));
#31851=CARTESIAN_POINT('Ctrl Pts',(-56.6633988084854,-106.726779175832,
171.975054738546));
#31852=CARTESIAN_POINT('Ctrl Pts',(-58.3052754451425,-106.457462928602,
171.975054808055));
#31853=CARTESIAN_POINT('Ctrl Pts',(-59.9471520817997,-106.188146681373,
171.975054877564));
#31854=CARTESIAN_POINT('Ctrl Pts',(-61.1052233453421,-105.97040731917,173.149682754692));
#31855=CARTESIAN_POINT('Ctrl Pts',(-62.2632946088845,-105.752667956968,
174.32431063182));
#31856=CARTESIAN_POINT('Ctrl Pts',(-62.2533564768505,-105.659446199681,
175.985485236888));
#31857=CARTESIAN_POINT('Ctrl Pts',(-62.2434183448166,-105.566224442394,
177.646659841956));
#31858=CARTESIAN_POINT('Ctrl Pts',(-61.0654708576941,-105.597520285706,
178.821287620784));
#31859=CARTESIAN_POINT('Ctrl Pts',(-59.8875233705716,-105.628816129018,
179.995915399612));
#31860=CARTESIAN_POINT('Ctrl Pts',(-58.2257706080804,-105.711688846937,
179.995915330104));
#31861=CARTESIAN_POINT('Ctrl Pts',(-56.5640178455893,-105.794561564856,
179.995915260595));
#31862=CARTESIAN_POINT('Ctrl Pts',(-55.3860704562128,-105.825857397748,
178.821287383467));
#31863=CARTESIAN_POINT('Ctrl Pts',(-54.2081230668364,-105.85715323064,177.646659506339));
#31864=CARTESIAN_POINT('Ctrl Pts',(-54.1981850730363,-105.763931458616,
175.985484901271));
#31865=CARTESIAN_POINT('Ctrl Pts',(-54.1882470792362,-105.670709686593,
174.324310296203));
#31866=CARTESIAN_POINT('Ctrl Pts',(-55.3463184405247,-105.452970313969,
173.149682517375));
#31867=CARTESIAN_POINT('Ctrl Pts',(-56.5043898018132,-105.235230941346,
171.975054738546));
#31868=CARTESIAN_POINT('Ctrl Pts',(-58.1462664384703,-104.965914694117,
171.975054808055));
#31869=CARTESIAN_POINT('Ctrl Pts',(-59.7881430751274,-104.696598446888,
171.975054877564));
#31870=CARTESIAN_POINT('Ctrl Pts',(-60.9462143386698,-104.478859084685,
173.149682754692));
#31871=CARTESIAN_POINT('Ctrl Pts',(-62.1042856022123,-104.261119722482,
174.32431063182));
#31872=CARTESIAN_POINT('Ctrl Pts',(-62.0943474701783,-104.167897965195,
175.985485236888));
#31873=CARTESIAN_POINT('Ctrl Pts',(-62.0844093381444,-104.074676207908,
177.646659841956));
#31874=CARTESIAN_POINT('Ctrl Pts',(-60.9064618510219,-104.10597205122,178.821287620784));
#31875=CARTESIAN_POINT('Ctrl Pts',(-59.7285143638993,-104.137267894533,
179.995915399612));
#31876=CARTESIAN_POINT('Ctrl Pts',(-58.0667616014082,-104.220140612451,
179.995915330104));
#31877=CARTESIAN_POINT('Ctrl Pts',(-56.4050088389171,-104.30301333037,179.995915260595));
#31878=CARTESIAN_POINT('Ctrl Pts',(-55.2270614495406,-104.334309163262,
178.821287383467));
#31879=CARTESIAN_POINT('Ctrl Pts',(-54.0491140601642,-104.365604996154,
177.646659506339));
#31880=CARTESIAN_POINT('Ctrl Pts',(-54.039176066364,-104.272383224131,175.985484901271));
#31881=CARTESIAN_POINT('Ctrl Pts',(-54.029238072564,-104.179161452107,174.324310296203));
#31882=CARTESIAN_POINT('Ctrl Pts',(-55.1873094338524,-103.961422079484,
173.149682517375));
#31883=CARTESIAN_POINT('Ctrl Pts',(-56.345380795141,-103.743682706861,171.975054738546));
#31884=CARTESIAN_POINT('Ctrl Pts',(-57.9872574317981,-103.474366459631,
171.975054808055));
#31885=CARTESIAN_POINT('Ctrl Pts',(-59.6291340684552,-103.205050212402,
171.975054877564));
#31886=CARTESIAN_POINT('Ctrl Pts',(-60.7872053319976,-102.987310850199,
173.149682754692));
#31887=CARTESIAN_POINT('Ctrl Pts',(-61.94527659554,-102.769571487996,174.32431063182));
#31888=CARTESIAN_POINT('Ctrl Pts',(-61.9353384635061,-102.676349730709,
175.985485236888));
#31889=CARTESIAN_POINT('Ctrl Pts',(-61.9254003314722,-102.583127973422,
177.646659841956));
#31890=CARTESIAN_POINT('Ctrl Pts',(-60.7474528443496,-102.614423816735,
178.821287620784));
#31891=CARTESIAN_POINT('Ctrl Pts',(-59.5695053572271,-102.645719660047,
179.995915399612));
#31892=CARTESIAN_POINT('Ctrl Pts',(-57.907752594736,-102.728592377966,179.995915330104));
#31893=CARTESIAN_POINT('Ctrl Pts',(-56.2459998322448,-102.811465095885,
179.995915260595));
#31894=CARTESIAN_POINT('Ctrl Pts',(-55.0680524428684,-102.842760928777,
178.821287383467));
#31895=CARTESIAN_POINT('Ctrl Pts',(-53.8901050534919,-102.874056761669,
177.646659506339));
#31896=CARTESIAN_POINT('Ctrl Pts',(-53.8801670596918,-102.780834989645,
175.985484901271));
#31897=CARTESIAN_POINT('Ctrl Pts',(-53.8702290658917,-102.687613217621,
174.324310296203));
#31898=CARTESIAN_POINT('Ctrl Pts',(-55.0283004271802,-102.469873844998,
173.149682517375));
#31899=CARTESIAN_POINT('Ctrl Pts',(-56.1863717884687,-102.252134472375,
171.975054738546));
#31900=CARTESIAN_POINT('Ctrl Pts',(-57.8282484251258,-101.982818225146,
171.975054808055));
#31901=CARTESIAN_POINT('Ctrl Pts',(-59.470125061783,-101.713501977916,171.975054877564));
#31902=CARTESIAN_POINT('Ctrl Pts',(-60.6281963253254,-101.495762615714,
173.149682754692));
#31903=CARTESIAN_POINT('Ctrl Pts',(-61.7862675888678,-101.278023253511,
174.32431063182));
#31904=CARTESIAN_POINT('Ctrl Pts',(-61.7763294568339,-101.184801496224,
175.985485236888));
#31905=CARTESIAN_POINT('Ctrl Pts',(-61.7663913247999,-101.091579738937,
177.646659841956));
#31906=CARTESIAN_POINT('Ctrl Pts',(-60.5884438376774,-101.122875582249,
178.821287620784));
#31907=CARTESIAN_POINT('Ctrl Pts',(-59.4104963505549,-101.154171425562,
179.995915399612));
#31908=CARTESIAN_POINT('Ctrl Pts',(-57.7487435880637,-101.23704414348,179.995915330104));
#31909=CARTESIAN_POINT('Ctrl Pts',(-56.0869908255726,-101.319916861399,
179.995915260595));
#31910=CARTESIAN_POINT('Ctrl Pts',(-54.9090434361961,-101.351212694291,
178.821287383467));
#31911=CARTESIAN_POINT('Ctrl Pts',(-53.7310960468197,-101.382508527183,
177.646659506339));
#31912=CARTESIAN_POINT('Ctrl Pts',(-53.7211580530196,-101.289286755159,
175.985484901271));
#31913=CARTESIAN_POINT('Ctrl Pts',(-53.7112200592195,-101.196064983136,
174.324310296203));
#31914=CARTESIAN_POINT('Ctrl Pts',(-54.869291420508,-100.978325610513,173.149682517375));
#31915=CARTESIAN_POINT('Ctrl Pts',(-56.0273627817965,-100.760586237889,
171.975054738546));
#31916=CARTESIAN_POINT('Ctrl Pts',(-57.6692394184536,-100.49126999066,171.975054808055));
#31917=CARTESIAN_POINT('Ctrl Pts',(-59.3111160551107,-100.221953743431,
171.975054877564));
#31918=CARTESIAN_POINT('Ctrl Pts',(-60.4691873186531,-100.004214381228,
173.149682754692));
#31919=CARTESIAN_POINT('Ctrl Pts',(-61.6272585821956,-99.7864750190253,
174.32431063182));
#31920=CARTESIAN_POINT('Ctrl Pts',(-61.6173204501616,-99.6932532617382,
175.985485236888));
#31921=CARTESIAN_POINT('Ctrl Pts',(-61.6073823181277,-99.6000315044512,
177.646659841956));
#31922=CARTESIAN_POINT('Ctrl Pts',(-60.4294348310052,-99.6313273477637,
178.821287620784));
#31923=CARTESIAN_POINT('Ctrl Pts',(-59.2514873438827,-99.6626231910761,
179.995915399612));
#31924=CARTESIAN_POINT('Ctrl Pts',(-57.5897345813915,-99.7454959089947,
179.995915330104));
#31925=CARTESIAN_POINT('Ctrl Pts',(-55.9279818189004,-99.8283686269133,
179.995915260595));
#31926=CARTESIAN_POINT('Ctrl Pts',(-54.7500344295239,-99.8596644598054,
178.821287383467));
#31927=CARTESIAN_POINT('Ctrl Pts',(-53.5720870401475,-99.8909602926975,
177.646659506339));
#31928=CARTESIAN_POINT('Ctrl Pts',(-53.5621490463474,-99.7977385206737,
175.985484901271));
#31929=CARTESIAN_POINT('Ctrl Pts',(-53.5522110525473,-99.7045167486501,
174.324310296203));
#31930=CARTESIAN_POINT('Ctrl Pts',(-54.7102824138358,-99.4867773760269,
173.149682517375));
#31931=CARTESIAN_POINT('Ctrl Pts',(-55.8683537751243,-99.2690380034038,
171.975054738546));
#31932=CARTESIAN_POINT('Ctrl Pts',(-57.5102304117814,-98.9997217561745,
171.975054808055));
#31933=CARTESIAN_POINT('Ctrl Pts',(-59.1521070484385,-98.7304055089452,
171.975054877564));
#31934=CARTESIAN_POINT('Ctrl Pts',(-60.3101783119809,-98.5126661467424,
173.149682754692));
#31935=CARTESIAN_POINT('Ctrl Pts',(-61.4682495755234,-98.2949267845397,
174.32431063182));
#31936=CARTESIAN_POINT('Ctrl Pts',(-61.4583114434894,-98.2017050272526,
175.985485236888));
#31937=CARTESIAN_POINT('Ctrl Pts',(-61.4483733114555,-98.1084832699656,
177.646659841956));
#31938=CARTESIAN_POINT('Ctrl Pts',(-60.2704258243329,-98.139779113278,178.821287620784));
#31939=CARTESIAN_POINT('Ctrl Pts',(-59.0924783372104,-98.1710749565905,
179.995915399612));
#31940=CARTESIAN_POINT('Ctrl Pts',(-57.4307255747193,-98.2539476745091,
179.995915330104));
#31941=CARTESIAN_POINT('Ctrl Pts',(-55.7689728122282,-98.3368203924277,
179.995915260595));
#31942=CARTESIAN_POINT('Ctrl Pts',(-54.5910254228517,-98.3681162253198,
178.821287383467));
#31943=CARTESIAN_POINT('Ctrl Pts',(-56.1988062143188,-113.449542435949,
178.821287383467));
#31944=CARTESIAN_POINT('Ctrl Pts',(-55.0208588249424,-113.480838268841,
177.646659506339));
#31945=CARTESIAN_POINT('Ctrl Pts',(-55.0109208311422,-113.387616496817,
175.985484901271));
#31946=CARTESIAN_POINT('Ctrl Pts',(-55.0009828373422,-113.294394724794,
174.324310296203));
#31947=CARTESIAN_POINT('Ctrl Pts',(-56.1590541986307,-113.07665535217,173.149682517375));
#31948=CARTESIAN_POINT('Ctrl Pts',(-57.3171255599192,-112.858915979547,
171.975054738546));
#31949=CARTESIAN_POINT('Ctrl Pts',(-58.9590021965763,-112.589599732318,
171.975054808055));
#31950=CARTESIAN_POINT('Ctrl Pts',(-60.6008788332334,-112.320283485089,
171.975054877564));
#31951=CARTESIAN_POINT('Ctrl Pts',(-61.7589500967758,-112.102544122886,
173.149682754692));
#31952=CARTESIAN_POINT('Ctrl Pts',(-62.9170213603182,-111.884804760683,
174.32431063182));
#31953=CARTESIAN_POINT('Ctrl Pts',(-62.9070832282843,-111.791583003396,
175.985485236888));
#31954=CARTESIAN_POINT('Ctrl Pts',(-62.8971450962504,-111.698361246109,
177.646659841956));
#31955=CARTESIAN_POINT('Ctrl Pts',(-61.7191976091278,-111.729657089422,
178.821287620784));
#31956=CARTESIAN_POINT('Ctrl Pts',(-60.5412501220053,-111.760952932734,
179.995915399612));
#31957=CARTESIAN_POINT('Ctrl Pts',(-58.8794973595142,-111.843825650653,
179.995915330104));
#31958=CARTESIAN_POINT('Ctrl Pts',(-57.217744597023,-111.926698368571,179.995915260595));
#31959=CARTESIAN_POINT('Ctrl Pts',(-56.0397972076466,-111.957994201463,
178.821287383467));
#31960=CARTESIAN_POINT('Ctrl Pts',(-54.8618498182701,-111.989290034355,
177.646659506339));
#31961=CARTESIAN_POINT('Ctrl Pts',(-54.85191182447,-111.896068262332,175.985484901271));
#31962=CARTESIAN_POINT('Ctrl Pts',(-54.8419738306699,-111.802846490308,
174.324310296203));
#31963=CARTESIAN_POINT('Ctrl Pts',(-56.0000451919584,-111.585107117685,
173.149682517375));
#31964=CARTESIAN_POINT('Ctrl Pts',(-57.158116553247,-111.367367745062,171.975054738546));
#31965=CARTESIAN_POINT('Ctrl Pts',(-58.799993189904,-111.098051497832,171.975054808055));
#31966=CARTESIAN_POINT('Ctrl Pts',(-60.4418698265612,-110.828735250603,
171.975054877564));
#31967=CARTESIAN_POINT('Ctrl Pts',(-61.5999410901036,-110.6109958884,173.149682754692));
#31968=CARTESIAN_POINT('Ctrl Pts',(-62.758012353646,-110.393256526198,174.32431063182));
#31969=CARTESIAN_POINT('Ctrl Pts',(-62.7480742216121,-110.30003476891,175.985485236888));
#31970=CARTESIAN_POINT('Ctrl Pts',(-62.7381360895782,-110.206813011623,
177.646659841956));
#31971=CARTESIAN_POINT('Ctrl Pts',(-61.5601886024556,-110.238108854936,
178.821287620784));
#31972=CARTESIAN_POINT('Ctrl Pts',(-60.3822411153331,-110.269404698248,
179.995915399612));
#31973=CARTESIAN_POINT('Ctrl Pts',(-58.7204883528419,-110.352277416167,
179.995915330104));
#31974=CARTESIAN_POINT('Ctrl Pts',(-57.0587355903508,-110.435150134086,
179.995915260595));
#31975=CARTESIAN_POINT('Ctrl Pts',(-55.8807882009743,-110.466445966978,
178.821287383467));
#31976=CARTESIAN_POINT('Ctrl Pts',(-54.7028408115979,-110.49774179987,177.646659506339));
#31977=CARTESIAN_POINT('Ctrl Pts',(-54.6929028177978,-110.404520027846,
175.985484901271));
#31978=CARTESIAN_POINT('Ctrl Pts',(-54.6829648239977,-110.311298255822,
174.324310296203));
#31979=CARTESIAN_POINT('Ctrl Pts',(-55.8410361852862,-110.093558883199,
173.149682517375));
#31980=CARTESIAN_POINT('Ctrl Pts',(-56.9991075465747,-109.875819510576,
171.975054738546));
#31981=CARTESIAN_POINT('Ctrl Pts',(-58.6409841832318,-109.606503263347,
171.975054808055));
#31982=CARTESIAN_POINT('Ctrl Pts',(-60.2828608198889,-109.337187016117,
171.975054877564));
#31983=CARTESIAN_POINT('Ctrl Pts',(-61.4409320834313,-109.119447653915,
173.149682754692));
#31984=CARTESIAN_POINT('Ctrl Pts',(-62.5990033469738,-108.901708291712,
174.32431063182));
#31985=CARTESIAN_POINT('Ctrl Pts',(-62.5890652149398,-108.808486534425,
175.985485236888));
#31986=CARTESIAN_POINT('Ctrl Pts',(-62.5791270829059,-108.715264777138,
177.646659841956));
#31987=CARTESIAN_POINT('Ctrl Pts',(-61.4011795957834,-108.74656062045,178.821287620784));
#31988=CARTESIAN_POINT('Ctrl Pts',(-60.2232321086609,-108.777856463763,
179.995915399612));
#31989=CARTESIAN_POINT('Ctrl Pts',(-58.5614793461697,-108.860729181681,
179.995915330104));
#31990=CARTESIAN_POINT('Ctrl Pts',(-56.8997265836786,-108.9436018996,179.995915260595));
#31991=CARTESIAN_POINT('Ctrl Pts',(-55.7217791943021,-108.974897732492,
178.821287383467));
#31992=CARTESIAN_POINT('Ctrl Pts',(-54.5438318049257,-109.006193565384,
177.646659506339));
#31993=CARTESIAN_POINT('Ctrl Pts',(-54.5338938111256,-108.91297179336,175.985484901271));
#31994=CARTESIAN_POINT('Ctrl Pts',(-54.5239558173255,-108.819750021337,
174.324310296203));
#31995=CARTESIAN_POINT('Ctrl Pts',(-55.682027178614,-108.602010648714,173.149682517375));
#31996=CARTESIAN_POINT('Ctrl Pts',(-56.8400985399025,-108.384271276091,
171.975054738546));
#31997=CARTESIAN_POINT('Ctrl Pts',(-58.4819751765596,-108.114955028861,
171.975054808055));
#31998=CARTESIAN_POINT('Ctrl Pts',(-60.1238518132167,-107.845638781632,
171.975054877564));
#31999=CARTESIAN_POINT('Ctrl Pts',(-61.2819230767591,-107.627899419429,
173.149682754692));
#32000=CARTESIAN_POINT('Ctrl Pts',(-62.4399943403016,-107.410160057226,
174.32431063182));
#32001=CARTESIAN_POINT('Ctrl Pts',(-62.4300562082676,-107.316938299939,
175.985485236888));
#32002=CARTESIAN_POINT('Ctrl Pts',(-62.4201180762337,-107.223716542652,
177.646659841956));
#32003=CARTESIAN_POINT('Ctrl Pts',(-61.2421705891111,-107.255012385965,
178.821287620784));
#32004=CARTESIAN_POINT('Ctrl Pts',(-60.0642231019886,-107.286308229277,
179.995915399612));
#32005=CARTESIAN_POINT('Ctrl Pts',(-58.4024703394975,-107.369180947196,
179.995915330104));
#32006=CARTESIAN_POINT('Ctrl Pts',(-56.7407175770064,-107.452053665114,
179.995915260595));
#32007=CARTESIAN_POINT('Ctrl Pts',(-55.5627701876299,-107.483349498006,
178.821287383467));
#32008=CARTESIAN_POINT('Ctrl Pts',(-54.3848227982534,-107.514645330899,
177.646659506339));
#32009=CARTESIAN_POINT('Ctrl Pts',(-54.3748848044533,-107.421423558875,
175.985484901271));
#32010=CARTESIAN_POINT('Ctrl Pts',(-54.3649468106533,-107.328201786851,
174.324310296203));
#32011=CARTESIAN_POINT('Ctrl Pts',(-55.5230181719417,-107.110462414228,
173.149682517375));
#32012=CARTESIAN_POINT('Ctrl Pts',(-56.6810895332303,-106.892723041605,
171.975054738546));
#32013=CARTESIAN_POINT('Ctrl Pts',(-58.3229661698874,-106.623406794376,
171.975054808055));
#32014=CARTESIAN_POINT('Ctrl Pts',(-59.9648428065445,-106.354090547146,
171.975054877564));
#32015=CARTESIAN_POINT('Ctrl Pts',(-61.1229140700869,-106.136351184943,
173.149682754692));
#32016=CARTESIAN_POINT('Ctrl Pts',(-62.2809853336293,-105.918611822741,
174.32431063182));
#32017=CARTESIAN_POINT('Ctrl Pts',(-62.2710472015954,-105.825390065454,
175.985485236888));
#32018=CARTESIAN_POINT('Ctrl Pts',(-62.2611090695615,-105.732168308167,
177.646659841956));
#32019=CARTESIAN_POINT('Ctrl Pts',(-61.0831615824389,-105.763464151479,
178.821287620784));
#32020=CARTESIAN_POINT('Ctrl Pts',(-59.9052140953164,-105.794759994792,
179.995915399612));
#32021=CARTESIAN_POINT('Ctrl Pts',(-58.2434613328252,-105.87763271271,179.995915330104));
#32022=CARTESIAN_POINT('Ctrl Pts',(-56.5817085703341,-105.960505430629,
179.995915260595));
#32023=CARTESIAN_POINT('Ctrl Pts',(-55.4037611809577,-105.991801263521,
178.821287383467));
#32024=CARTESIAN_POINT('Ctrl Pts',(-54.2258137915812,-106.023097096413,
177.646659506339));
#32025=CARTESIAN_POINT('Ctrl Pts',(-54.2158757977811,-105.929875324389,
175.985484901271));
#32026=CARTESIAN_POINT('Ctrl Pts',(-54.205937803981,-105.836653552366,174.324310296203));
#32027=CARTESIAN_POINT('Ctrl Pts',(-55.3640091652695,-105.618914179742,
173.149682517375));
#32028=CARTESIAN_POINT('Ctrl Pts',(-56.522080526558,-105.401174807119,171.975054738546));
#32029=CARTESIAN_POINT('Ctrl Pts',(-58.1639571632151,-105.13185855989,171.975054808055));
#32030=CARTESIAN_POINT('Ctrl Pts',(-59.8058337998722,-104.862542312661,
171.975054877564));
#32031=CARTESIAN_POINT('Ctrl Pts',(-60.9639050634147,-104.644802950458,
173.149682754692));
#32032=CARTESIAN_POINT('Ctrl Pts',(-62.1219763269571,-104.427063588255,
174.32431063182));
#32033=CARTESIAN_POINT('Ctrl Pts',(-62.1120381949232,-104.333841830968,
175.985485236888));
#32034=CARTESIAN_POINT('Ctrl Pts',(-62.1021000628892,-104.240620073681,
177.646659841956));
#32035=CARTESIAN_POINT('Ctrl Pts',(-60.9241525757667,-104.271915916993,
178.821287620784));
#32036=CARTESIAN_POINT('Ctrl Pts',(-59.7462050886442,-104.303211760306,
179.995915399612));
#32037=CARTESIAN_POINT('Ctrl Pts',(-58.084452326153,-104.386084478225,179.995915330104));
#32038=CARTESIAN_POINT('Ctrl Pts',(-56.4226995636619,-104.468957196143,
179.995915260595));
#32039=CARTESIAN_POINT('Ctrl Pts',(-55.2447521742854,-104.500253029035,
178.821287383467));
#32040=CARTESIAN_POINT('Ctrl Pts',(-54.066804784909,-104.531548861927,177.646659506339));
#32041=CARTESIAN_POINT('Ctrl Pts',(-54.0568667911089,-104.438327089904,
175.985484901271));
#32042=CARTESIAN_POINT('Ctrl Pts',(-54.0469287973088,-104.34510531788,174.324310296203));
#32043=CARTESIAN_POINT('Ctrl Pts',(-55.2050001585973,-104.127365945257,
173.149682517375));
#32044=CARTESIAN_POINT('Ctrl Pts',(-56.3630715198858,-103.909626572634,
171.975054738546));
#32045=CARTESIAN_POINT('Ctrl Pts',(-58.0049481565429,-103.640310325404,
171.975054808055));
#32046=CARTESIAN_POINT('Ctrl Pts',(-59.6468247932,-103.370994078175,171.975054877564));
#32047=CARTESIAN_POINT('Ctrl Pts',(-60.8048960567424,-103.153254715972,
173.149682754692));
#32048=CARTESIAN_POINT('Ctrl Pts',(-61.9629673202849,-102.93551535377,174.32431063182));
#32049=CARTESIAN_POINT('Ctrl Pts',(-61.9530291882509,-102.842293596483,
175.985485236888));
#32050=CARTESIAN_POINT('Ctrl Pts',(-61.943091056217,-102.749071839196,177.646659841956));
#32051=CARTESIAN_POINT('Ctrl Pts',(-60.7651435690945,-102.780367682508,
178.821287620784));
#32052=CARTESIAN_POINT('Ctrl Pts',(-59.587196081972,-102.81166352582,179.995915399612));
#32053=CARTESIAN_POINT('Ctrl Pts',(-57.9254433194808,-102.894536243739,
179.995915330104));
#32054=CARTESIAN_POINT('Ctrl Pts',(-56.2636905569897,-102.977408961658,
179.995915260595));
#32055=CARTESIAN_POINT('Ctrl Pts',(-55.0857431676132,-103.00870479455,178.821287383467));
#32056=CARTESIAN_POINT('Ctrl Pts',(-53.9077957782368,-103.040000627442,
177.646659506339));
#32057=CARTESIAN_POINT('Ctrl Pts',(-53.8978577844367,-102.946778855418,
175.985484901271));
#32058=CARTESIAN_POINT('Ctrl Pts',(-53.8879197906366,-102.853557083394,
174.324310296203));
#32059=CARTESIAN_POINT('Ctrl Pts',(-55.0459911519251,-102.635817710771,
173.149682517375));
#32060=CARTESIAN_POINT('Ctrl Pts',(-56.2040625132136,-102.418078338148,
171.975054738546));
#32061=CARTESIAN_POINT('Ctrl Pts',(-57.8459391498707,-102.148762090919,
171.975054808055));
#32062=CARTESIAN_POINT('Ctrl Pts',(-59.4878157865278,-101.879445843689,
171.975054877564));
#32063=CARTESIAN_POINT('Ctrl Pts',(-60.6458870500702,-101.661706481487,
173.149682754692));
#32064=CARTESIAN_POINT('Ctrl Pts',(-61.8039583136126,-101.443967119284,
174.32431063182));
#32065=CARTESIAN_POINT('Ctrl Pts',(-61.7940201815787,-101.350745361997,
175.985485236888));
#32066=CARTESIAN_POINT('Ctrl Pts',(-61.7840820495448,-101.25752360471,177.646659841956));
#32067=CARTESIAN_POINT('Ctrl Pts',(-60.6061345624222,-101.288819448022,
178.821287620784));
#32068=CARTESIAN_POINT('Ctrl Pts',(-59.4281870752997,-101.320115291335,
179.995915399612));
#32069=CARTESIAN_POINT('Ctrl Pts',(-57.7664343128086,-101.402988009253,
179.995915330104));
#32070=CARTESIAN_POINT('Ctrl Pts',(-56.1046815503175,-101.485860727172,
179.995915260595));
#32071=CARTESIAN_POINT('Ctrl Pts',(-54.926734160941,-101.517156560064,178.821287383467));
#32072=CARTESIAN_POINT('Ctrl Pts',(-53.7487867715645,-101.548452392956,
177.646659506339));
#32073=CARTESIAN_POINT('Ctrl Pts',(-53.7388487777644,-101.455230620932,
175.985484901271));
#32074=CARTESIAN_POINT('Ctrl Pts',(-53.7289107839643,-101.362008848909,
174.324310296203));
#32075=CARTESIAN_POINT('Ctrl Pts',(-54.8869821452528,-101.144269476286,
173.149682517375));
#32076=CARTESIAN_POINT('Ctrl Pts',(-56.0450535065414,-100.926530103662,
171.975054738546));
#32077=CARTESIAN_POINT('Ctrl Pts',(-57.6869301431984,-100.657213856433,
171.975054808055));
#32078=CARTESIAN_POINT('Ctrl Pts',(-59.3288067798556,-100.387897609204,
171.975054877564));
#32079=CARTESIAN_POINT('Ctrl Pts',(-60.486878043398,-100.170158247001,173.149682754692));
#32080=CARTESIAN_POINT('Ctrl Pts',(-61.6449493069404,-99.9524188847983,
174.32431063182));
#32081=CARTESIAN_POINT('Ctrl Pts',(-61.6350111749065,-99.8591971275113,
175.985485236888));
#32082=CARTESIAN_POINT('Ctrl Pts',(-61.6250730428726,-99.7659753702243,
177.646659841956));
#32083=CARTESIAN_POINT('Ctrl Pts',(-60.44712555575,-99.7972712135367,178.821287620784));
#32084=CARTESIAN_POINT('Ctrl Pts',(-59.2691780686275,-99.8285670568492,
179.995915399612));
#32085=CARTESIAN_POINT('Ctrl Pts',(-57.6074253061363,-99.9114397747677,
179.995915330104));
#32086=CARTESIAN_POINT('Ctrl Pts',(-55.9456725436452,-99.9943124926864,
179.995915260595));
#32087=CARTESIAN_POINT('Ctrl Pts',(-54.7677251542687,-100.025608325578,
178.821287383467));
#32088=CARTESIAN_POINT('Ctrl Pts',(-53.5897777648923,-100.05690415847,177.646659506339));
#32089=CARTESIAN_POINT('Ctrl Pts',(-53.5798397710922,-99.9636823864468,
175.985484901271));
#32090=CARTESIAN_POINT('Ctrl Pts',(-53.5699017772921,-99.8704606144232,
174.324310296203));
#32091=CARTESIAN_POINT('Ctrl Pts',(-54.7279731385806,-99.6527212418,173.149682517375));
#32092=CARTESIAN_POINT('Ctrl Pts',(-55.8860444998691,-99.4349818691769,
171.975054738546));
#32093=CARTESIAN_POINT('Ctrl Pts',(-57.5279211365262,-99.1656656219475,
171.975054808055));
#32094=CARTESIAN_POINT('Ctrl Pts',(-59.1697977731833,-98.8963493747183,
171.975054877564));
#32095=CARTESIAN_POINT('Ctrl Pts',(-60.3278690367257,-98.6786100125155,
173.149682754692));
#32096=CARTESIAN_POINT('Ctrl Pts',(-61.4859403002682,-98.4608706503128,
174.32431063182));
#32097=CARTESIAN_POINT('Ctrl Pts',(-61.4760021682342,-98.3676488930257,
175.985485236888));
#32098=CARTESIAN_POINT('Ctrl Pts',(-61.4660640362003,-98.2744271357387,
177.646659841956));
#32099=CARTESIAN_POINT('Ctrl Pts',(-60.2881165490778,-98.3057229790511,
178.821287620784));
#32100=CARTESIAN_POINT('Ctrl Pts',(-59.1101690619552,-98.3370188223636,
179.995915399612));
#32101=CARTESIAN_POINT('Ctrl Pts',(-57.4484162994641,-98.4198915402821,
179.995915330104));
#32102=CARTESIAN_POINT('Ctrl Pts',(-55.786663536973,-98.5027642582008,179.995915260595));
#32103=CARTESIAN_POINT('Ctrl Pts',(-54.6087161475965,-98.5340600910929,
178.821287383467));
#32104=CARTESIAN_POINT('Ctrl Pts',(-56.2237961054143,-113.614380048479,
178.813912075476));
#32105=CARTESIAN_POINT('Ctrl Pts',(-55.0488864554725,-113.645352038053,
177.6423391512));
#32106=CARTESIAN_POINT('Ctrl Pts',(-55.0389484614927,-113.552130266048,
175.985484901707));
#32107=CARTESIAN_POINT('Ctrl Pts',(-55.0290104675128,-113.458908494044,
174.328630652215));
#32108=CARTESIAN_POINT('Ctrl Pts',(-56.1840440891124,-113.241492964766,
173.157057825983));
#32109=CARTESIAN_POINT('Ctrl Pts',(-57.3390777107121,-113.024077435489,
171.985484999752));
#32110=CARTESIAN_POINT('Ctrl Pts',(-58.9766583348819,-112.755219171892,
171.985485069079));
#32111=CARTESIAN_POINT('Ctrl Pts',(-60.6142389590518,-112.486360908295,
171.985485138407));
#32112=CARTESIAN_POINT('Ctrl Pts',(-61.7692724831595,-112.268945389411,
173.157058062683));
#32113=CARTESIAN_POINT('Ctrl Pts',(-62.9243060072673,-112.051529870527,
174.328630986959));
#32114=CARTESIAN_POINT('Ctrl Pts',(-62.9143678754131,-111.95830811322,175.985485236451));
#32115=CARTESIAN_POINT('Ctrl Pts',(-62.9044297435589,-111.865086355914,
177.642339485944));
#32116=CARTESIAN_POINT('Ctrl Pts',(-61.7295199961253,-111.896058355881,
178.813912312176));
#32117=CARTESIAN_POINT('Ctrl Pts',(-60.5546102486917,-111.927030355848,
179.985485138407));
#32118=CARTESIAN_POINT('Ctrl Pts',(-58.8971534986878,-112.009445090134,
179.985485069079));
#32119=CARTESIAN_POINT('Ctrl Pts',(-57.2396967486839,-112.09185982442,179.985484999752));
#32120=CARTESIAN_POINT('Ctrl Pts',(-56.0647870987421,-112.122831813994,
178.813912075476));
#32121=CARTESIAN_POINT('Ctrl Pts',(-54.8898774488003,-112.153803803567,
177.6423391512));
#32122=CARTESIAN_POINT('Ctrl Pts',(-54.8799394548205,-112.060582031563,
175.985484901707));
#32123=CARTESIAN_POINT('Ctrl Pts',(-54.8700014608406,-111.967360259558,
174.328630652215));
#32124=CARTESIAN_POINT('Ctrl Pts',(-56.0250350824402,-111.749944730281,
173.157057825983));
#32125=CARTESIAN_POINT('Ctrl Pts',(-57.1800687040398,-111.532529201003,
171.985484999752));
#32126=CARTESIAN_POINT('Ctrl Pts',(-58.8176493282097,-111.263670937406,
171.985485069079));
#32127=CARTESIAN_POINT('Ctrl Pts',(-60.4552299523796,-110.994812673809,
171.985485138407));
#32128=CARTESIAN_POINT('Ctrl Pts',(-61.6102634764873,-110.777397154925,
173.157058062683));
#32129=CARTESIAN_POINT('Ctrl Pts',(-62.7652970005951,-110.559981636041,
174.328630986959));
#32130=CARTESIAN_POINT('Ctrl Pts',(-62.7553588687409,-110.466759878735,
175.985485236451));
#32131=CARTESIAN_POINT('Ctrl Pts',(-62.7454207368867,-110.373538121429,
177.642339485944));
#32132=CARTESIAN_POINT('Ctrl Pts',(-61.5705109894531,-110.404510121395,
178.813912312176));
#32133=CARTESIAN_POINT('Ctrl Pts',(-60.3956012420194,-110.435482121362,
179.985485138407));
#32134=CARTESIAN_POINT('Ctrl Pts',(-58.7381444920155,-110.517896855648,
179.985485069079));
#32135=CARTESIAN_POINT('Ctrl Pts',(-57.0806877420116,-110.600311589935,
179.985484999752));
#32136=CARTESIAN_POINT('Ctrl Pts',(-55.9057780920699,-110.631283579508,
178.813912075476));
#32137=CARTESIAN_POINT('Ctrl Pts',(-54.7308684421281,-110.662255569082,
177.6423391512));
#32138=CARTESIAN_POINT('Ctrl Pts',(-54.7209304481482,-110.569033797077,
175.985484901707));
#32139=CARTESIAN_POINT('Ctrl Pts',(-54.7109924541684,-110.475812025073,
174.328630652215));
#32140=CARTESIAN_POINT('Ctrl Pts',(-55.866026075768,-110.258396495795,173.157057825983));
#32141=CARTESIAN_POINT('Ctrl Pts',(-57.0210596973676,-110.040980966518,
171.985484999752));
#32142=CARTESIAN_POINT('Ctrl Pts',(-58.6586403215375,-109.772122702921,
171.985485069079));
#32143=CARTESIAN_POINT('Ctrl Pts',(-60.2962209457073,-109.503264439324,
171.985485138407));
#32144=CARTESIAN_POINT('Ctrl Pts',(-61.4512544698151,-109.28584892044,173.157058062683));
#32145=CARTESIAN_POINT('Ctrl Pts',(-62.6062879939228,-109.068433401555,
174.328630986959));
#32146=CARTESIAN_POINT('Ctrl Pts',(-62.5963498620687,-108.975211644249,
175.985485236451));
#32147=CARTESIAN_POINT('Ctrl Pts',(-62.5864117302145,-108.881989886943,
177.642339485944));
#32148=CARTESIAN_POINT('Ctrl Pts',(-61.4115019827808,-108.91296188691,178.813912312176));
#32149=CARTESIAN_POINT('Ctrl Pts',(-60.2365922353472,-108.943933886877,
179.985485138407));
#32150=CARTESIAN_POINT('Ctrl Pts',(-58.5791354853433,-109.026348621163,
179.985485069079));
#32151=CARTESIAN_POINT('Ctrl Pts',(-56.9216787353394,-109.108763355449,
179.985484999752));
#32152=CARTESIAN_POINT('Ctrl Pts',(-55.7467690853976,-109.139735345023,
178.813912075476));
#32153=CARTESIAN_POINT('Ctrl Pts',(-54.5718594354559,-109.170707334596,
177.6423391512));
#32154=CARTESIAN_POINT('Ctrl Pts',(-54.561921441476,-109.077485562592,175.985484901707));
#32155=CARTESIAN_POINT('Ctrl Pts',(-54.5519834474962,-108.984263790587,
174.328630652215));
#32156=CARTESIAN_POINT('Ctrl Pts',(-55.7070170690958,-108.76684826131,173.157057825983));
#32157=CARTESIAN_POINT('Ctrl Pts',(-56.8620506906954,-108.549432732032,
171.985484999752));
#32158=CARTESIAN_POINT('Ctrl Pts',(-58.4996313148652,-108.280574468435,
171.985485069079));
#32159=CARTESIAN_POINT('Ctrl Pts',(-60.1372119390351,-108.011716204838,
171.985485138407));
#32160=CARTESIAN_POINT('Ctrl Pts',(-61.2922454631428,-107.794300685954,
173.157058062683));
#32161=CARTESIAN_POINT('Ctrl Pts',(-62.4472789872506,-107.57688516707,174.328630986959));
#32162=CARTESIAN_POINT('Ctrl Pts',(-62.4373408553964,-107.483663409764,
175.985485236451));
#32163=CARTESIAN_POINT('Ctrl Pts',(-62.4274027235423,-107.390441652457,
177.642339485944));
#32164=CARTESIAN_POINT('Ctrl Pts',(-61.2524929761086,-107.421413652424,
178.813912312176));
#32165=CARTESIAN_POINT('Ctrl Pts',(-60.077583228675,-107.452385652391,179.985485138407));
#32166=CARTESIAN_POINT('Ctrl Pts',(-58.4201264786711,-107.534800386677,
179.985485069079));
#32167=CARTESIAN_POINT('Ctrl Pts',(-56.7626697286672,-107.617215120964,
179.985484999752));
#32168=CARTESIAN_POINT('Ctrl Pts',(-55.5877600787254,-107.648187110537,
178.813912075476));
#32169=CARTESIAN_POINT('Ctrl Pts',(-54.4128504287836,-107.67915910011,177.6423391512));
#32170=CARTESIAN_POINT('Ctrl Pts',(-54.4029124348038,-107.585937328106,
175.985484901707));
#32171=CARTESIAN_POINT('Ctrl Pts',(-54.3929744408239,-107.492715556102,
174.328630652215));
#32172=CARTESIAN_POINT('Ctrl Pts',(-55.5480080624235,-107.275300026824,
173.157057825983));
#32173=CARTESIAN_POINT('Ctrl Pts',(-56.7030416840231,-107.057884497547,
171.985484999752));
#32174=CARTESIAN_POINT('Ctrl Pts',(-58.340622308193,-106.78902623395,171.985485069079));
#32175=CARTESIAN_POINT('Ctrl Pts',(-59.9782029323629,-106.520167970353,
171.985485138407));
#32176=CARTESIAN_POINT('Ctrl Pts',(-61.1332364564706,-106.302752451468,
173.157058062683));
#32177=CARTESIAN_POINT('Ctrl Pts',(-62.2882699805784,-106.085336932584,
174.328630986959));
#32178=CARTESIAN_POINT('Ctrl Pts',(-62.2783318487242,-105.992115175278,
175.985485236451));
#32179=CARTESIAN_POINT('Ctrl Pts',(-62.26839371687,-105.898893417972,177.642339485944));
#32180=CARTESIAN_POINT('Ctrl Pts',(-61.0934839694364,-105.929865417939,
178.813912312176));
#32181=CARTESIAN_POINT('Ctrl Pts',(-59.9185742220028,-105.960837417905,
179.985485138407));
#32182=CARTESIAN_POINT('Ctrl Pts',(-58.2611174719989,-106.043252152192,
179.985485069079));
#32183=CARTESIAN_POINT('Ctrl Pts',(-56.603660721995,-106.125666886478,179.985484999752));
#32184=CARTESIAN_POINT('Ctrl Pts',(-55.4287510720532,-106.156638876051,
178.813912075476));
#32185=CARTESIAN_POINT('Ctrl Pts',(-54.2538414221114,-106.187610865625,
177.6423391512));
#32186=CARTESIAN_POINT('Ctrl Pts',(-54.2439034281315,-106.09438909362,175.985484901707));
#32187=CARTESIAN_POINT('Ctrl Pts',(-54.2339654341517,-106.001167321616,
174.328630652215));
#32188=CARTESIAN_POINT('Ctrl Pts',(-55.3889990557513,-105.783751792338,
173.157057825983));
#32189=CARTESIAN_POINT('Ctrl Pts',(-56.5440326773509,-105.566336263061,
171.985484999752));
#32190=CARTESIAN_POINT('Ctrl Pts',(-58.1816133015208,-105.297477999464,
171.985485069079));
#32191=CARTESIAN_POINT('Ctrl Pts',(-59.8191939256906,-105.028619735867,
171.985485138407));
#32192=CARTESIAN_POINT('Ctrl Pts',(-60.9742274497984,-104.811204216983,
173.157058062683));
#32193=CARTESIAN_POINT('Ctrl Pts',(-62.1292609739061,-104.593788698099,
174.328630986959));
#32194=CARTESIAN_POINT('Ctrl Pts',(-62.119322842052,-104.500566940792,175.985485236451));
#32195=CARTESIAN_POINT('Ctrl Pts',(-62.1093847101978,-104.407345183486,
177.642339485944));
#32196=CARTESIAN_POINT('Ctrl Pts',(-60.9344749627642,-104.438317183453,
178.813912312176));
#32197=CARTESIAN_POINT('Ctrl Pts',(-59.7595652153305,-104.46928918342,179.985485138407));
#32198=CARTESIAN_POINT('Ctrl Pts',(-58.1021084653266,-104.551703917706,
179.985485069079));
#32199=CARTESIAN_POINT('Ctrl Pts',(-56.4446517153227,-104.634118651992,
179.985484999752));
#32200=CARTESIAN_POINT('Ctrl Pts',(-55.269742065381,-104.665090641566,178.813912075476));
#32201=CARTESIAN_POINT('Ctrl Pts',(-54.0948324154392,-104.696062631139,
177.6423391512));
#32202=CARTESIAN_POINT('Ctrl Pts',(-54.0848944214593,-104.602840859135,
175.985484901707));
#32203=CARTESIAN_POINT('Ctrl Pts',(-54.0749564274795,-104.50961908713,174.328630652215));
#32204=CARTESIAN_POINT('Ctrl Pts',(-55.2299900490791,-104.292203557853,
173.157057825983));
#32205=CARTESIAN_POINT('Ctrl Pts',(-56.3850236706787,-104.074788028575,
171.985484999752));
#32206=CARTESIAN_POINT('Ctrl Pts',(-58.0226042948486,-103.805929764978,
171.985485069079));
#32207=CARTESIAN_POINT('Ctrl Pts',(-59.6601849190184,-103.537071501381,
171.985485138407));
#32208=CARTESIAN_POINT('Ctrl Pts',(-60.8152184431262,-103.319655982497,
173.157058062683));
#32209=CARTESIAN_POINT('Ctrl Pts',(-61.9702519672339,-103.102240463613,
174.328630986959));
#32210=CARTESIAN_POINT('Ctrl Pts',(-61.9603138353797,-103.009018706307,
175.985485236451));
#32211=CARTESIAN_POINT('Ctrl Pts',(-61.9503757035256,-102.915796949001,
177.642339485944));
#32212=CARTESIAN_POINT('Ctrl Pts',(-60.7754659560919,-102.946768948967,
178.813912312176));
#32213=CARTESIAN_POINT('Ctrl Pts',(-59.6005562086583,-102.977740948934,
179.985485138407));
#32214=CARTESIAN_POINT('Ctrl Pts',(-57.9430994586544,-103.06015568322,179.985485069079));
#32215=CARTESIAN_POINT('Ctrl Pts',(-56.2856427086505,-103.142570417507,
179.985484999752));
#32216=CARTESIAN_POINT('Ctrl Pts',(-55.1107330587087,-103.17354240708,178.813912075476));
#32217=CARTESIAN_POINT('Ctrl Pts',(-53.935823408767,-103.204514396654,177.6423391512));
#32218=CARTESIAN_POINT('Ctrl Pts',(-53.9258854147871,-103.111292624649,
175.985484901707));
#32219=CARTESIAN_POINT('Ctrl Pts',(-53.9159474208072,-103.018070852645,
174.328630652215));
#32220=CARTESIAN_POINT('Ctrl Pts',(-55.0709810424069,-102.800655323367,
173.157057825983));
#32221=CARTESIAN_POINT('Ctrl Pts',(-56.2260146640065,-102.58323979409,171.985484999752));
#32222=CARTESIAN_POINT('Ctrl Pts',(-57.8635952881763,-102.314381530493,
171.985485069079));
#32223=CARTESIAN_POINT('Ctrl Pts',(-59.5011759123462,-102.045523266896,
171.985485138407));
#32224=CARTESIAN_POINT('Ctrl Pts',(-60.6562094364539,-101.828107748012,
173.157058062683));
#32225=CARTESIAN_POINT('Ctrl Pts',(-61.8112429605617,-101.610692229127,
174.328630986959));
#32226=CARTESIAN_POINT('Ctrl Pts',(-61.8013048287075,-101.517470471821,
175.985485236451));
#32227=CARTESIAN_POINT('Ctrl Pts',(-61.7913666968533,-101.424248714515,
177.642339485944));
#32228=CARTESIAN_POINT('Ctrl Pts',(-60.6164569494197,-101.455220714482,
178.813912312176));
#32229=CARTESIAN_POINT('Ctrl Pts',(-59.4415472019861,-101.486192714449,
179.985485138407));
#32230=CARTESIAN_POINT('Ctrl Pts',(-57.7840904519822,-101.568607448735,
179.985485069079));
#32231=CARTESIAN_POINT('Ctrl Pts',(-56.1266337019783,-101.651022183021,
179.985484999752));
#32232=CARTESIAN_POINT('Ctrl Pts',(-54.9517240520365,-101.681994172595,
178.813912075476));
#32233=CARTESIAN_POINT('Ctrl Pts',(-53.7768144020947,-101.712966162168,
177.6423391512));
#32234=CARTESIAN_POINT('Ctrl Pts',(-53.7668764081149,-101.619744390164,
175.985484901707));
#32235=CARTESIAN_POINT('Ctrl Pts',(-53.756938414135,-101.526522618159,174.328630652215));
#32236=CARTESIAN_POINT('Ctrl Pts',(-54.9119720357346,-101.309107088882,
173.157057825983));
#32237=CARTESIAN_POINT('Ctrl Pts',(-56.0670056573342,-101.091691559604,
171.985484999752));
#32238=CARTESIAN_POINT('Ctrl Pts',(-57.7045862815041,-100.822833296007,
171.985485069079));
#32239=CARTESIAN_POINT('Ctrl Pts',(-59.342166905674,-100.55397503241,171.985485138407));
#32240=CARTESIAN_POINT('Ctrl Pts',(-60.4972004297817,-100.336559513526,
173.157058062683));
#32241=CARTESIAN_POINT('Ctrl Pts',(-61.6522339538895,-100.119143994642,
174.328630986959));
#32242=CARTESIAN_POINT('Ctrl Pts',(-61.6422958220353,-100.025922237336,
175.985485236451));
#32243=CARTESIAN_POINT('Ctrl Pts',(-61.6323576901811,-99.9327004800294,
177.642339485944));
#32244=CARTESIAN_POINT('Ctrl Pts',(-60.4574479427475,-99.9636724799962,
178.813912312176));
#32245=CARTESIAN_POINT('Ctrl Pts',(-59.2825381953138,-99.994644479963,179.985485138407));
#32246=CARTESIAN_POINT('Ctrl Pts',(-57.6250814453099,-100.077059214249,
179.985485069079));
#32247=CARTESIAN_POINT('Ctrl Pts',(-55.9676246953061,-100.159473948536,
179.985484999752));
#32248=CARTESIAN_POINT('Ctrl Pts',(-54.7927150453643,-100.190445938109,
178.813912075476));
#32249=CARTESIAN_POINT('Ctrl Pts',(-53.6178053954225,-100.221417927683,
177.6423391512));
#32250=CARTESIAN_POINT('Ctrl Pts',(-53.6078674014426,-100.128196155678,
175.985484901707));
#32251=CARTESIAN_POINT('Ctrl Pts',(-53.5979294074628,-100.034974383673,
174.328630652215));
#32252=CARTESIAN_POINT('Ctrl Pts',(-54.7529630290624,-99.817558854396,173.157057825983));
#32253=CARTESIAN_POINT('Ctrl Pts',(-55.907996650662,-99.6001433251185,171.985484999752));
#32254=CARTESIAN_POINT('Ctrl Pts',(-57.5455772748319,-99.3312850615215,
171.985485069079));
#32255=CARTESIAN_POINT('Ctrl Pts',(-59.1831578990017,-99.0624267979246,
171.985485138407));
#32256=CARTESIAN_POINT('Ctrl Pts',(-60.3381914231095,-98.8450112790404,
173.157058062683));
#32257=CARTESIAN_POINT('Ctrl Pts',(-61.4932249472172,-98.6275957601562,
174.328630986959));
#32258=CARTESIAN_POINT('Ctrl Pts',(-61.4832868153631,-98.53437400285,175.985485236451));
#32259=CARTESIAN_POINT('Ctrl Pts',(-61.4733486835089,-98.4411522455438,
177.642339485944));
#32260=CARTESIAN_POINT('Ctrl Pts',(-60.2984389360752,-98.4721242455106,
178.813912312176));
#32261=CARTESIAN_POINT('Ctrl Pts',(-59.1235291886416,-98.5030962454774,
179.985485138407));
#32262=CARTESIAN_POINT('Ctrl Pts',(-57.4660724386377,-98.5855109797636,
179.985485069079));
#32263=CARTESIAN_POINT('Ctrl Pts',(-55.8086156886338,-98.6679257140499,
179.985484999752));
#32264=CARTESIAN_POINT('Ctrl Pts',(-54.633706038692,-98.6988977036234,178.813912075476));
#32265=CARTESIAN_POINT('Origin',(-31.7758655563387,23.6116972707429,178.485485069079));
#32266=CARTESIAN_POINT('Origin',(-31.7758655563387,23.6116972707429,173.985485069079));
#32267=CARTESIAN_POINT('Origin',(-31.7758655563387,23.6116972707429,177.985485069079));
#32268=CARTESIAN_POINT('Ctrl Pts',(-33.7101944105682,36.1001541204655,173.485485069079));
#32269=CARTESIAN_POINT('Ctrl Pts',(-33.9682581825426,35.6003903982821,173.143998023837));
#32270=CARTESIAN_POINT('Ctrl Pts',(-33.3358320373305,35.4434146616551,173.235485069079));
#32271=CARTESIAN_POINT('Ctrl Pts',(-33.5757636385812,36.3604914102378,172.982269696584));
#32272=CARTESIAN_POINT('Ctrl Pts',(-33.8204276914646,35.8561010262747,172.645545369172));
#32273=CARTESIAN_POINT('Ctrl Pts',(-33.1880191877447,35.7136289261714,172.732268406515));
#32274=CARTESIAN_POINT('Ctrl Pts',(-33.4516565150982,36.6248074047901,172.479340629102));
#32275=CARTESIAN_POINT('Ctrl Pts',(-33.6822917663529,36.1173819195843,172.144313013639));
#32276=CARTESIAN_POINT('Ctrl Pts',(-33.0506074115036,35.9881357503632,172.229339795881));
#32277=CARTESIAN_POINT('Ctrl Pts',(-33.3378144598069,36.8927267103254,171.976487691182));
#32278=CARTESIAN_POINT('Ctrl Pts',(-33.5545758603726,36.3825939324359,171.641904135334));
#32279=CARTESIAN_POINT('Ctrl Pts',(-32.9232632882234,36.2665888893428,171.726487691182));
#32280=CARTESIAN_POINT('Origin',(-33.26592800316,35.8707475833996,173.485485069079));
#32281=CARTESIAN_POINT('Ctrl Pts',(-34.1412494001895,35.3369392868692,173.985485069079));
#32282=CARTESIAN_POINT('Ctrl Pts',(-34.1412494001895,35.3369392868692,173.485485069079));
#32283=CARTESIAN_POINT('Ctrl Pts',(-33.7154041461839,35.0749167312735,173.485485069079));
#32284=CARTESIAN_POINT('Ctrl Pts',(-34.0503675686949,35.4846425887064,173.985485046591));
#32285=CARTESIAN_POINT('Ctrl Pts',(-34.0908546515829,35.4188420329393,173.456207535552));
#32286=CARTESIAN_POINT('Ctrl Pts',(-33.6387071223109,35.1455646668778,173.485485069079));
#32287=CARTESIAN_POINT('Ctrl Pts',(-33.9619493301675,35.6363826725923,173.940377868901));
#32288=CARTESIAN_POINT('Ctrl Pts',(-34.050965142566,35.4840104825677,173.400217226376));
#32289=CARTESIAN_POINT('Ctrl Pts',(-33.5621652331424,35.2185830930478,173.462931467345));
#32290=CARTESIAN_POINT('Ctrl Pts',(-33.8135226820125,35.9025198720883,173.769060220931));
#32291=CARTESIAN_POINT('Ctrl Pts',(-33.9938812681979,35.5714820882983,173.274080148675));
#32292=CARTESIAN_POINT('Ctrl Pts',(-33.4306927660806,35.3472393598486,173.37727264665));
#32293=CARTESIAN_POINT('Ctrl Pts',(-33.7516274460001,36.0199153180548,173.640581477849));
#32294=CARTESIAN_POINT('Ctrl Pts',(-33.977283069749,35.5920962921692,173.203436824419));
#32295=CARTESIAN_POINT('Ctrl Pts',(-33.3741378393645,35.4043412967755,173.312985330162));
#32296=CARTESIAN_POINT('Ctrl Pts',(-33.7101944105682,36.1001541204655,173.485485069079));
#32297=CARTESIAN_POINT('Ctrl Pts',(-33.9682581825426,35.6003903982821,173.143998023837));
#32298=CARTESIAN_POINT('Ctrl Pts',(-33.3358320373305,35.4434146616551,173.235485069079));
#32299=CARTESIAN_POINT('Origin',(-33.7154041461839,35.0749167312736,173.985485069079));
#32300=CARTESIAN_POINT('Origin',(-44.1060283439209,41.4682670878081,173.985485069079));
#32301=CARTESIAN_POINT('Origin',(-37.1738630900728,31.4290895869696,173.985485069079));
#32302=CARTESIAN_POINT('Origin',(-31.7758655563387,23.6116972707429,173.985485069079));
#32303=CARTESIAN_POINT('Origin',(-41.1020539958444,25.42062214227,173.985485069079));
#32304=CARTESIAN_POINT('Origin',(-36.6843857876575,24.5637629925993,173.985485069079));
#32305=CARTESIAN_POINT('Origin',(-36.6843857876575,24.5637629925993,177.985485069079));
#32306=CARTESIAN_POINT('Origin',(-41.1020539958444,25.42062214227,177.985485069079));
#32307=CARTESIAN_POINT('Origin',(-31.7758655563387,23.6116972707429,177.985485069079));
#32308=CARTESIAN_POINT('Origin',(-37.1738630900728,31.4290895869696,177.985485069079));
#32309=CARTESIAN_POINT('Origin',(-44.1060283439209,41.4682670878081,177.985485069079));
#32310=CARTESIAN_POINT('Origin',(-33.7154041461839,35.0749167312736,177.985485069079));
#32311=CARTESIAN_POINT('Ctrl Pts',(-33.7101944105682,36.1001541204655,178.485485069079));
#32312=CARTESIAN_POINT('Ctrl Pts',(-33.9682581825426,35.6003903982821,178.826972114322));
#32313=CARTESIAN_POINT('Ctrl Pts',(-33.3358320373305,35.4434146616551,178.735485069079));
#32314=CARTESIAN_POINT('Ctrl Pts',(-33.7516006038855,36.0199673002257,178.330489138169));
#32315=CARTESIAN_POINT('Ctrl Pts',(-33.977279425657,35.5920996411968,178.767557313941));
#32316=CARTESIAN_POINT('Ctrl Pts',(-33.3741156308558,35.4043639502364,178.658029740133));
#32317=CARTESIAN_POINT('Ctrl Pts',(-33.8133066023579,35.9029147229749,178.202225990637));
#32318=CARTESIAN_POINT('Ctrl Pts',(-33.9938040222832,35.5715957197603,178.697100878701));
#32319=CARTESIAN_POINT('Ctrl Pts',(-33.4304994268961,35.3474306123349,178.593855528671));
#32320=CARTESIAN_POINT('Ctrl Pts',(-33.9618960455694,35.6364708201442,178.030587223347));
#32321=CARTESIAN_POINT('Ctrl Pts',(-34.0509357072909,35.484060062052,178.570779964287));
#32322=CARTESIAN_POINT('Ctrl Pts',(-33.5621199729607,35.2186253327459,178.508036147401));
#32323=CARTESIAN_POINT('Ctrl Pts',(-34.0500285364698,35.4851935918964,177.985485070059));
#32324=CARTESIAN_POINT('Ctrl Pts',(-34.0906717048824,35.4191393620078,178.514868872724));
#32325=CARTESIAN_POINT('Ctrl Pts',(-33.6384206503181,35.1458285437047,178.485485069079));
#32326=CARTESIAN_POINT('Ctrl Pts',(-34.1412494001895,35.3369392868692,177.985485069079));
#32327=CARTESIAN_POINT('Ctrl Pts',(-34.1412494001895,35.3369392868692,178.485485069079));
#32328=CARTESIAN_POINT('Ctrl Pts',(-33.7154041461839,35.0749167312735,178.485485069079));
#32329=CARTESIAN_POINT('Origin',(-33.26592800316,35.8707475833996,178.485485069079));
#32330=CARTESIAN_POINT('Ctrl Pts',(-33.3358320373305,35.4434146616551,178.735485069079));
#32331=CARTESIAN_POINT('Ctrl Pts',(-33.9682581825426,35.6003903982821,178.826972114322));
#32332=CARTESIAN_POINT('Ctrl Pts',(-33.7101944105682,36.1001541204655,178.485485069079));
#32333=CARTESIAN_POINT('Ctrl Pts',(-33.1880191877447,35.7136289261714,179.238701731644));
#32334=CARTESIAN_POINT('Ctrl Pts',(-33.8204276914644,35.8561010262749,179.325424768988));
#32335=CARTESIAN_POINT('Ctrl Pts',(-33.5757636385812,36.3604914102378,178.988700441575));
#32336=CARTESIAN_POINT('Ctrl Pts',(-33.0506074115094,35.9881357503643,179.741630342279));
#32337=CARTESIAN_POINT('Ctrl Pts',(-33.682291766366,36.1173819195807,179.826657124525));
#32338=CARTESIAN_POINT('Ctrl Pts',(-33.4516565150989,36.6248074047886,179.491629509058));
#32339=CARTESIAN_POINT('Ctrl Pts',(-32.9232632882234,36.2665888893427,180.244482446977));
#32340=CARTESIAN_POINT('Ctrl Pts',(-33.5545758603726,36.3825939324359,180.329066002825));
#32341=CARTESIAN_POINT('Ctrl Pts',(-33.3378144598069,36.8927267103254,179.994482446977));
#32342=CARTESIAN_POINT('',(0.,0.,0.));
#32343=CARTESIAN_POINT('Origin',(-54.1598171290174,-67.5719248685924,175.985485069079));
#32344=CARTESIAN_POINT('',(-58.6617595746854,-127.180557396019,173.617797875548));
#32345=CARTESIAN_POINT('',(-58.6882610756022,-127.4291487666,173.617797875548));
#32346=CARTESIAN_POINT('',(-52.327900808713,-67.7672193871761,173.617797875548));
#32347=CARTESIAN_POINT('',(-57.5665324870377,-127.548732528291,176.406000729816));
#32348=CARTESIAN_POINT('Ctrl Pts',(-58.6617595746854,-127.180557396019,
173.617797875548));
#32349=CARTESIAN_POINT('Ctrl Pts',(-58.6326690473956,-127.186500029427,
173.640795835577));
#32350=CARTESIAN_POINT('Ctrl Pts',(-58.6039904583882,-127.192422600679,
173.664361934959));
#32351=CARTESIAN_POINT('Ctrl Pts',(-58.2740033449536,-127.261332757946,
173.946159765466));
#32352=CARTESIAN_POINT('Ctrl Pts',(-58.0269221360586,-127.320492066776,
174.262621377601));
#32353=CARTESIAN_POINT('Ctrl Pts',(-57.7119058734233,-127.412252654383,
174.89391038891));
#32354=CARTESIAN_POINT('Ctrl Pts',(-57.6177265345925,-127.447299103863,
175.18881819412));
#32355=CARTESIAN_POINT('Ctrl Pts',(-57.5224623503741,-127.504840915964,
175.795216859615));
#32356=CARTESIAN_POINT('Ctrl Pts',(-57.5212432809128,-127.528630260883,
176.102947888732));
#32357=CARTESIAN_POINT('Ctrl Pts',(-57.5665324870377,-127.548732528291,
176.406000729816));
#32358=CARTESIAN_POINT('Origin',(-60.5201773959065,-127.233854248016,175.985485069079));
#32359=CARTESIAN_POINT('Origin',(-54.1598171290174,-67.5719248685924,175.985485069079));
#32360=CARTESIAN_POINT('',(-58.502750568013,-125.689009161534,173.617797875548));
#32361=CARTESIAN_POINT('',(-58.5557535702374,-126.186191906362,173.617797875548));
#32362=CARTESIAN_POINT('',(-52.327900808713,-67.7672193871761,173.617797875548));
#32363=CARTESIAN_POINT('Ctrl Pts',(-58.5027505680128,-125.689009161534,
173.617797875548));
#32364=CARTESIAN_POINT('Ctrl Pts',(-58.4595554649872,-125.697833087609,
173.651946423045));
#32365=CARTESIAN_POINT('Ctrl Pts',(-58.417273020125,-125.706611876126,173.687344073633));
#32366=CARTESIAN_POINT('Ctrl Pts',(-58.0794854284382,-125.777931854482,
173.986693413553));
#32367=CARTESIAN_POINT('Ctrl Pts',(-57.8384992972673,-125.83646832066,174.307014661379));
#32368=CARTESIAN_POINT('Ctrl Pts',(-57.5019070438409,-125.936707051767,
175.012129922775));
#32369=CARTESIAN_POINT('Ctrl Pts',(-57.4044285699384,-125.97699712051,175.387614488075));
#32370=CARTESIAN_POINT('Ctrl Pts',(-57.3552475654393,-126.043039273718,
176.170863951934));
#32371=CARTESIAN_POINT('Ctrl Pts',(-57.4100194773212,-126.070042537833,
176.571447096641));
#32372=CARTESIAN_POINT('Ctrl Pts',(-57.6678719428223,-126.10693250791,177.315038171398));
#32373=CARTESIAN_POINT('Ctrl Pts',(-57.863027119267,-126.116088231247,177.652655147584));
#32374=CARTESIAN_POINT('Ctrl Pts',(-58.3793944921056,-126.121793925087,
178.247476301394));
#32375=CARTESIAN_POINT('Ctrl Pts',(-58.7002502206311,-126.120427424016,
178.495125960072));
#32376=CARTESIAN_POINT('Ctrl Pts',(-59.4066692402747,-126.109518767417,
178.844220731714));
#32377=CARTESIAN_POINT('Ctrl Pts',(-59.7827741197176,-126.099444134848,
178.947364493277));
#32378=CARTESIAN_POINT('Ctrl Pts',(-60.5679966693245,-126.076445160719,
179.007265954424));
#32379=CARTESIAN_POINT('Ctrl Pts',(-60.970235802468,-126.066399187525,178.957633872364));
#32380=CARTESIAN_POINT('Ctrl Pts',(-61.7179203138936,-126.051111545171,
178.708683533434));
#32381=CARTESIAN_POINT('Ctrl Pts',(-62.0578100965788,-126.044955448698,
178.517184058802));
#32382=CARTESIAN_POINT('Ctrl Pts',(-62.6583156091933,-126.041607882016,
178.007011011933));
#32383=CARTESIAN_POINT('Ctrl Pts',(-62.9096366389285,-126.047647349706,
177.688832858095));
#32384=CARTESIAN_POINT('Ctrl Pts',(-63.2669005850962,-126.074000042545,
176.98660161232));
#32385=CARTESIAN_POINT('Ctrl Pts',(-63.374361600946,-126.09267780599,176.611931574081));
#32386=CARTESIAN_POINT('Ctrl Pts',(-63.4438548314579,-126.145901209017,
175.828715776295));
#32387=CARTESIAN_POINT('Ctrl Pts',(-63.3997074250098,-126.18343619045,175.427281602623));
#32388=CARTESIAN_POINT('Ctrl Pts',(-63.1620897079078,-126.273224914735,
174.680859755401));
#32389=CARTESIAN_POINT('Ctrl Pts',(-62.9762532016153,-126.323223172721,
174.341333810424));
#32390=CARTESIAN_POINT('Ctrl Pts',(-62.4777155464864,-126.436966076225,
173.741502520989));
#32391=CARTESIAN_POINT('Ctrl Pts',(-62.1656928930358,-126.503055012754,
173.490806570389));
#32392=CARTESIAN_POINT('Ctrl Pts',(-61.4754256817193,-126.641115717402,
173.135363563321));
#32393=CARTESIAN_POINT('Ctrl Pts',(-61.106392475604,-126.710694606539,173.02895052633));
#32394=CARTESIAN_POINT('Ctrl Pts',(-60.3339981872262,-126.853598092212,
172.962334470896));
#32395=CARTESIAN_POINT('Ctrl Pts',(-59.9379422145433,-126.928642280698,
173.008654345021));
#32396=CARTESIAN_POINT('Ctrl Pts',(-59.2365162427146,-127.064829731118,
173.240052707569));
#32397=CARTESIAN_POINT('Ctrl Pts',(-58.9317136446724,-127.125410988432,
173.404381568257));
#32398=CARTESIAN_POINT('Ctrl Pts',(-58.6617595746854,-127.180557396019,
173.617797875548));
#32399=CARTESIAN_POINT('',(-61.6514014972539,-127.113258201155,173.209554841928));
#32400=CARTESIAN_POINT('Origin',(-60.5201773959065,-127.233854248016,175.985485069079));
#32401=CARTESIAN_POINT('Ctrl Pts',(-61.6514014972539,-127.113258201155,
173.209554841928));
#32402=CARTESIAN_POINT('Ctrl Pts',(-61.8857214195736,-127.067339449921,
173.307037826472));
#32403=CARTESIAN_POINT('Ctrl Pts',(-62.1065768825577,-127.022596527121,
173.434691800361));
#32404=CARTESIAN_POINT('Ctrl Pts',(-62.5071713663279,-126.938362080585,
173.741517658033));
#32405=CARTESIAN_POINT('Ctrl Pts',(-62.6859638108831,-126.899124933691,
173.918611232754));
#32406=CARTESIAN_POINT('Ctrl Pts',(-63.0767849285755,-126.808742110419,
174.418572728908));
#32407=CARTESIAN_POINT('Ctrl Pts',(-63.2526273897065,-126.758947602762,
174.76445318312));
#32408=CARTESIAN_POINT('Ctrl Pts',(-63.4679041817175,-126.671297722053,
175.52011789156));
#32409=CARTESIAN_POINT('Ctrl Pts',(-63.499642584004,-126.635152404933,175.924144803172));
#32410=CARTESIAN_POINT('Ctrl Pts',(-63.4051176552899,-126.585177337171,
176.706982606558));
#32411=CARTESIAN_POINT('Ctrl Pts',(-63.285302376919,-126.566901940954,177.078928358304));
#32412=CARTESIAN_POINT('Ctrl Pts',(-62.9042041225712,-126.542829629636,
177.771200206437));
#32413=CARTESIAN_POINT('Ctrl Pts',(-62.6415548816703,-126.538068000193,
178.081915888432));
#32414=CARTESIAN_POINT('Ctrl Pts',(-62.0224310979412,-126.54401866178,178.572749615368));
#32415=CARTESIAN_POINT('Ctrl Pts',(-61.6752270239872,-126.549984453082,
178.752880269944));
#32416=CARTESIAN_POINT('Ctrl Pts',(-60.9170006011623,-126.566116529594,
178.976236545733));
#32417=CARTESIAN_POINT('Ctrl Pts',(-60.5117969159758,-126.576552154303,
179.011628322045));
#32418=CARTESIAN_POINT('Ctrl Pts',(-59.7270399804243,-126.600160402056,
178.922934828744));
#32419=CARTESIAN_POINT('Ctrl Pts',(-59.3539170563406,-126.608889340411,
178.805732529249));
#32420=CARTESIAN_POINT('Ctrl Pts',(-58.6587254122993,-126.61830149431,178.42933450653));
#32421=CARTESIAN_POINT('Ctrl Pts',(-58.3463067253257,-126.618845616172,
178.168670455854));
#32422=CARTESIAN_POINT('Ctrl Pts',(-57.8519076813661,-126.611499757347,
177.552405199745));
#32423=CARTESIAN_POINT('Ctrl Pts',(-57.6695186672383,-126.599895212944,
177.206525382876));
#32424=CARTESIAN_POINT('Ctrl Pts',(-57.4405997529608,-126.559599585113,
176.45086158733));
#32425=CARTESIAN_POINT('Ctrl Pts',(-57.4019533413936,-126.53095775106,176.046834917067));
#32426=CARTESIAN_POINT('Ctrl Pts',(-57.4838157207256,-126.462178557917,
175.263997055208));
#32427=CARTESIAN_POINT('Ctrl Pts',(-57.5970842070223,-126.419054977016,
174.892051029029));
#32428=CARTESIAN_POINT('Ctrl Pts',(-57.9645401889828,-126.315181807793,
174.19977815377));
#32429=CARTESIAN_POINT('Ctrl Pts',(-58.220281537424,-126.255156269262,173.889061697831));
#32430=CARTESIAN_POINT('Ctrl Pts',(-58.5381763977807,-126.189788457904,
173.63177570516));
#32431=CARTESIAN_POINT('Ctrl Pts',(-58.5469462268658,-126.187991076671,
173.624760655177));
#32432=CARTESIAN_POINT('Ctrl Pts',(-58.5557535702374,-126.186191906362,
173.617797875548));
#32433=CARTESIAN_POINT('Origin',(-54.1598171290174,-67.5719248685924,175.985485069079));
#32434=CARTESIAN_POINT('',(-58.3437415613406,-124.197460927048,173.617797875548));
#32435=CARTESIAN_POINT('',(-58.3967445635652,-124.694643671877,173.617797875548));
#32436=CARTESIAN_POINT('',(-52.327900808713,-67.7672193871761,173.617797875548));
#32437=CARTESIAN_POINT('Ctrl Pts',(-58.34374156134,-124.197460927048,173.617797875549));
#32438=CARTESIAN_POINT('Ctrl Pts',(-58.278717133321,-124.210744163011,173.669203928853));
#32439=CARTESIAN_POINT('Ctrl Pts',(-58.2157774981849,-124.223921711853,
173.72342734048));
#32440=CARTESIAN_POINT('Ctrl Pts',(-57.86693839971,-124.29887647475,174.05071991815));
#32441=CARTESIAN_POINT('Ctrl Pts',(-57.6354963747508,-124.356416599752,
174.3767912935));
#32442=CARTESIAN_POINT('Ctrl Pts',(-57.3185687959958,-124.454312505303,
175.089710227681));
#32443=CARTESIAN_POINT('Ctrl Pts',(-57.231181633938,-124.492963368992,175.467464387374));
#32444=CARTESIAN_POINT('Ctrl Pts',(-57.2029760494815,-124.557220016337,
176.25061306551));
#32445=CARTESIAN_POINT('Ctrl Pts',(-57.2680216060115,-124.583151041461,
176.648644116405));
#32446=CARTESIAN_POINT('Ctrl Pts',(-57.5443231429321,-124.617842409801,
177.384195000057));
#32447=CARTESIAN_POINT('Ctrl Pts',(-57.7477568818853,-124.625564489675,
177.716476460062));
#32448=CARTESIAN_POINT('Ctrl Pts',(-58.2781818661706,-124.630202209204,
178.297117940058));
#32449=CARTESIAN_POINT('Ctrl Pts',(-58.604261517692,-124.628303276316,178.536132441238));
#32450=CARTESIAN_POINT('Ctrl Pts',(-59.3177217901214,-124.616426130427,
178.867360173637));
#32451=CARTESIAN_POINT('Ctrl Pts',(-59.6958031886026,-124.605603623277,
178.961296587042));
#32452=CARTESIAN_POINT('Ctrl Pts',(-60.4810402787824,-124.583014024349,
179.002234079384));
#32453=CARTESIAN_POINT('Ctrl Pts',(-60.8810526741571,-124.573231018561,
178.943280655469));
#32454=CARTESIAN_POINT('Ctrl Pts',(-61.6215604887575,-124.558503910591,
178.677569971472));
#32455=CARTESIAN_POINT('Ctrl Pts',(-61.9566204442423,-124.552340819203,
178.47852898906));
#32456=CARTESIAN_POINT('Ctrl Pts',(-62.5445331674686,-124.550727218005,
177.955650796022));
#32457=CARTESIAN_POINT('Ctrl Pts',(-62.7881669620093,-124.557612561274,
177.632707660284));
#32458=CARTESIAN_POINT('Ctrl Pts',(-63.1294599313677,-124.585475952162,
176.924046814847));
#32459=CARTESIAN_POINT('Ctrl Pts',(-63.2286500430818,-124.604529935403,
176.547543416596));
#32460=CARTESIAN_POINT('Ctrl Pts',(-63.2812732486243,-124.659924223454,
175.764303698241));
#32461=CARTESIAN_POINT('Ctrl Pts',(-63.2288064432854,-124.698372966086,
175.364833513626));
#32462=CARTESIAN_POINT('Ctrl Pts',(-62.9762088974864,-124.789578710455,
174.624824536462));
#32463=CARTESIAN_POINT('Ctrl Pts',(-62.7836064185933,-124.839809985127,
174.289599988599));
#32464=CARTESIAN_POINT('Ctrl Pts',(-62.2737713821488,-124.955111065801,
173.701104946398));
#32465=CARTESIAN_POINT('Ctrl Pts',(-61.9574763394134,-125.021682562797,
173.457305591578));
#32466=CARTESIAN_POINT('Ctrl Pts',(-61.2614358576456,-125.160190156705,
173.11620009463));
#32467=CARTESIAN_POINT('Ctrl Pts',(-60.8907253797158,-125.229477448949,
173.017172068597));
#32468=CARTESIAN_POINT('Ctrl Pts',(-60.1183056212707,-125.372719312397,
172.965738372967));
#32469=CARTESIAN_POINT('Ctrl Pts',(-59.7239590747349,-125.447608374899,
173.019538943988));
#32470=CARTESIAN_POINT('Ctrl Pts',(-59.0449242978319,-125.579760897032,
173.257771910224));
#32471=CARTESIAN_POINT('Ctrl Pts',(-58.7581639442399,-125.636833137111,
173.41587693548));
#32472=CARTESIAN_POINT('Ctrl Pts',(-58.5027505680127,-125.689009161534,
173.617797875548));
#32473=CARTESIAN_POINT('Ctrl Pts',(-58.5557535702374,-126.186191906362,
173.617797875548));
#32474=CARTESIAN_POINT('Ctrl Pts',(-58.8468157571489,-126.12673351778,173.387694224487));
#32475=CARTESIAN_POINT('Ctrl Pts',(-59.1781285607066,-126.061010728778,
173.21487622303));
#32476=CARTESIAN_POINT('Ctrl Pts',(-59.9119867119162,-125.91900878874,172.994735293252));
#32477=CARTESIAN_POINT('Ctrl Pts',(-60.31028336115,-125.843785900072,172.959342060538));
#32478=CARTESIAN_POINT('Ctrl Pts',(-61.0823803308402,-125.701423051036,
173.048032618572));
#32479=CARTESIAN_POINT('Ctrl Pts',(-61.4489580270192,-125.631295079213,
173.165233479167));
#32480=CARTESIAN_POINT('Ctrl Pts',(-62.1305109850442,-125.493937089217,
173.541628707431));
#32481=CARTESIAN_POINT('Ctrl Pts',(-62.4360238034073,-125.42860557392,173.80229143814));
#32482=CARTESIAN_POINT('Ctrl Pts',(-62.9177650813467,-125.31719656074,174.418554513344));
#32483=CARTESIAN_POINT('Ctrl Pts',(-63.0936098866123,-125.267402024571,
174.764433477334));
#32484=CARTESIAN_POINT('Ctrl Pts',(-63.3088919467895,-125.179751635932,
175.520096051261));
#32485=CARTESIAN_POINT('Ctrl Pts',(-63.3406332741939,-125.143605987515,
175.924122398547));
#32486=CARTESIAN_POINT('Ctrl Pts',(-63.2461142301944,-125.093630152303,
176.706960338648));
#32487=CARTESIAN_POINT('Ctrl Pts',(-63.1263018689129,-125.075354683216,
177.078906732069));
#32488=CARTESIAN_POINT('Ctrl Pts',(-62.7452092371237,-125.051281830243,
177.771180981795));
#32489=CARTESIAN_POINT('Ctrl Pts',(-62.482562646969,-125.046519897283,178.081898473403));
#32490=CARTESIAN_POINT('Ctrl Pts',(-61.8634432306732,-125.052469942589,
178.572736816437));
#32491=CARTESIAN_POINT('Ctrl Pts',(-61.5162408978839,-125.058435804369,
178.752870170917));
#32492=CARTESIAN_POINT('Ctrl Pts',(-60.7580169368939,-125.074567680543,
178.976232568843));
#32493=CARTESIAN_POINT('Ctrl Pts',(-60.352813898473,-125.085003213792,179.011627750477));
#32494=CARTESIAN_POINT('Ctrl Pts',(-59.5680567885864,-125.108611318063,
178.922941120341));
#32495=CARTESIAN_POINT('Ctrl Pts',(-59.1949331554322,-125.117340607453,
178.805742185244));
#32496=CARTESIAN_POINT('Ctrl Pts',(-58.4997387559432,-125.126753121904,
178.429350696446));
#32497=CARTESIAN_POINT('Ctrl Pts',(-58.1873179848685,-125.127297441734,
178.168689732086));
#32498=CARTESIAN_POINT('Ctrl Pts',(-57.6929136127509,-125.119951976616,
177.552429575312));
#32499=CARTESIAN_POINT('Ctrl Pts',(-57.5105215242164,-125.108348056214,
177.206551752621));
#32500=CARTESIAN_POINT('Ctrl Pts',(-57.2815955753712,-125.068053250165,
176.450890813437));
#32501=CARTESIAN_POINT('Ctrl Pts',(-57.2429452440014,-125.03941180795,176.046864898358));
#32502=CARTESIAN_POINT('Ctrl Pts',(-57.3247997090401,-124.970633271046,
175.26402685357));
#32503=CARTESIAN_POINT('Ctrl Pts',(-57.4380643589416,-124.927510417756,
174.892079968718));
#32504=CARTESIAN_POINT('Ctrl Pts',(-57.8055128332414,-124.823638126178,
174.199803879735));
#32505=CARTESIAN_POINT('Ctrl Pts',(-58.0612506286147,-124.763612938422,
173.88908500224));
#32506=CARTESIAN_POINT('Ctrl Pts',(-58.3791506952548,-124.698243645248,
173.63178906037));
#32507=CARTESIAN_POINT('Ctrl Pts',(-58.3879288364918,-124.696444554813,
173.624767283041));
#32508=CARTESIAN_POINT('Ctrl Pts',(-58.3967445635651,-124.694643671877,
173.617797875548));
#32509=CARTESIAN_POINT('Origin',(-54.1598171290174,-67.5719248685924,175.985485069079));
#32510=CARTESIAN_POINT('',(-58.1847325546685,-122.705912692563,173.617797875548));
#32511=CARTESIAN_POINT('',(-58.2377355568929,-123.203095437391,173.617797875548));
#32512=CARTESIAN_POINT('',(-52.327900808713,-67.7672193871761,173.617797875548));
#32513=CARTESIAN_POINT('Ctrl Pts',(-58.1847325546681,-122.705912692563,
173.617797875548));
#32514=CARTESIAN_POINT('Ctrl Pts',(-58.0888037581628,-122.72550909469,173.693635848704));
#32515=CARTESIAN_POINT('Ctrl Pts',(-57.9974675052454,-122.744864161319,
173.775561284347));
#32516=CARTESIAN_POINT('Ctrl Pts',(-57.635193264641,-122.824746707671,174.143923073571));
#32517=CARTESIAN_POINT('Ctrl Pts',(-57.4174742924988,-122.880811110816,
174.477660857283));
#32518=CARTESIAN_POINT('Ctrl Pts',(-57.1284820778,-122.975343264355,175.201169564384));
#32519=CARTESIAN_POINT('Ctrl Pts',(-57.0554958265115,-123.011890461818,
175.58217845336));
#32520=CARTESIAN_POINT('Ctrl Pts',(-57.0572909473777,-123.073553655012,
176.364680651823));
#32521=CARTESIAN_POINT('Ctrl Pts',(-57.1369028743213,-123.097925409945,
176.75859945057));
#32522=CARTESIAN_POINT('Ctrl Pts',(-57.4394283465603,-123.129454707669,
177.482254367609));
#32523=CARTESIAN_POINT('Ctrl Pts',(-57.6548410632274,-123.135320137726,
177.806852553459));
#32524=CARTESIAN_POINT('Ctrl Pts',(-58.2053009099689,-123.138409294449,
178.366627513958));
#32525=CARTESIAN_POINT('Ctrl Pts',(-58.5385649216933,-123.135743765666,
178.592913316506));
#32526=CARTESIAN_POINT('Ctrl Pts',(-59.2618597324605,-123.122470579587,
178.898109819127));
#32527=CARTESIAN_POINT('Ctrl Pts',(-59.6428651617749,-123.110749483957,
178.978602970774));
#32528=CARTESIAN_POINT('Ctrl Pts',(-60.4276995799954,-123.088771782396,
178.991737724848));
#32529=CARTESIAN_POINT('Ctrl Pts',(-60.8240557545849,-123.079382925796,
178.91922063596));
#32530=CARTESIAN_POINT('Ctrl Pts',(-61.5537076523256,-123.065483845327,
178.62907684617));
#32531=CARTESIAN_POINT('Ctrl Pts',(-61.8816641007378,-123.059487581138,
178.41888613984));
#32532=CARTESIAN_POINT('Ctrl Pts',(-62.4506266599793,-123.06044421288,177.877438877806));
#32533=CARTESIAN_POINT('Ctrl Pts',(-62.6826700572172,-123.068573995083,
177.547746392789));
#32534=CARTESIAN_POINT('Ctrl Pts',(-63.0001500560096,-123.098664511368,
176.829855484596));
#32535=CARTESIAN_POINT('Ctrl Pts',(-63.0870062275806,-123.118442728469,
176.450600259355));
#32536=CARTESIAN_POINT('Ctrl Pts',(-63.1143318720006,-123.177064485505,
175.667676176508));
#32537=CARTESIAN_POINT('Ctrl Pts',(-63.0494694161852,-123.216847380813,
175.271476563352));
#32538=CARTESIAN_POINT('Ctrl Pts',(-62.7745240797572,-123.310141261318,
174.541360502104));
#32539=CARTESIAN_POINT('Ctrl Pts',(-62.5717178576519,-123.360872587181,
174.212618504973));
#32540=CARTESIAN_POINT('Ctrl Pts',(-62.0449874310108,-123.4784856219,173.641525042349));
#32541=CARTESIAN_POINT('Ctrl Pts',(-61.7224759660809,-123.545735839993,
173.408333024239));
#32542=CARTESIAN_POINT('Ctrl Pts',(-61.0179373514153,-123.684871698295,
173.089054639054));
#32543=CARTESIAN_POINT('Ctrl Pts',(-60.644673418105,-123.753849182772,173.001283842222));
#32544=CARTESIAN_POINT('Ctrl Pts',(-59.8724994791847,-123.897555628781,
172.973083438963));
#32545=CARTESIAN_POINT('Ctrl Pts',(-59.4810335737413,-123.972156402458,
173.038266935018));
#32546=CARTESIAN_POINT('Ctrl Pts',(-58.8363428602948,-124.098087770071,
173.28551300444));
#32547=CARTESIAN_POINT('Ctrl Pts',(-58.5768781736677,-124.149835615648,
173.43348817094));
#32548=CARTESIAN_POINT('Ctrl Pts',(-58.34374156134,-124.197460927048,173.617797875549));
#32549=CARTESIAN_POINT('Ctrl Pts',(-58.3967445635652,-124.694643671877,
173.617797875548));
#32550=CARTESIAN_POINT('Ctrl Pts',(-58.6877979782988,-124.635187075281,
173.387701159466));
#32551=CARTESIAN_POINT('Ctrl Pts',(-59.0190996859056,-124.569466434783,
173.214886551717));
#32552=CARTESIAN_POINT('Ctrl Pts',(-59.7529443816364,-124.427466899675,
172.994740615175));
#32553=CARTESIAN_POINT('Ctrl Pts',(-60.1512401590161,-124.35224407383,172.959342825569));
#32554=CARTESIAN_POINT('Ctrl Pts',(-60.9233373162518,-124.20988098793,173.048024199532));
#32555=CARTESIAN_POINT('Ctrl Pts',(-61.2899160389894,-124.139753275246,
173.165220558003));
#32556=CARTESIAN_POINT('Ctrl Pts',(-61.9714727030833,-124.002394979554,
173.541607042789));
#32557=CARTESIAN_POINT('Ctrl Pts',(-62.2769883034669,-123.937063135279,
173.802265643482));
#32558=CARTESIAN_POINT('Ctrl Pts',(-62.75873666217,-123.82565313399,174.418521894913));
#32559=CARTESIAN_POINT('Ctrl Pts',(-62.9345856650678,-123.775858546739,
174.764398190367));
#32560=CARTESIAN_POINT('Ctrl Pts',(-63.1498771588972,-123.688207248561,
175.520056941991));
#32561=CARTESIAN_POINT('Ctrl Pts',(-63.1816237242831,-123.652061006897,
175.924082278689));
#32562=CARTESIAN_POINT('Ctrl Pts',(-63.0871152180042,-123.602083797421,
176.706920463546));
#32563=CARTESIAN_POINT('Ctrl Pts',(-62.9673080803201,-123.58380819782,177.078868006009));
#32564=CARTESIAN_POINT('Ctrl Pts',(-62.5862255167875,-123.559734374918,
177.77114655618));
#32565=CARTESIAN_POINT('Ctrl Pts',(-62.3235836733225,-123.554971898455,
178.081867288186));
#32566=CARTESIAN_POINT('Ctrl Pts',(-61.7044720777724,-123.560920840194,
178.572713897156));
#32567=CARTESIAN_POINT('Ctrl Pts',(-61.357272862849,-123.566886828148,178.7528520863));
#32568=CARTESIAN_POINT('Ctrl Pts',(-60.5990533102727,-123.583018345583,
178.976225446972));
#32569=CARTESIAN_POINT('Ctrl Pts',(-60.1938514300712,-123.593453715054,
179.011626726427));
#32570=CARTESIAN_POINT('Ctrl Pts',(-59.4090940080818,-123.617061562393,
178.922952386006));
#32571=CARTESIAN_POINT('Ctrl Pts',(-59.0359691052097,-123.625791480335,
178.805759475439));
#32572=CARTESIAN_POINT('Ctrl Pts',(-58.3407697716994,-123.635204640415,
178.429379686755));
#32573=CARTESIAN_POINT('Ctrl Pts',(-58.0283452687598,-123.63574931474,178.16872424901));
#32574=CARTESIAN_POINT('Ctrl Pts',(-57.5339313557417,-123.628404554622,
177.552473223514));
#32575=CARTESIAN_POINT('Ctrl Pts',(-57.3515337619774,-123.616801751553,
177.20659897172));
#32576=CARTESIAN_POINT('Ctrl Pts',(-57.122595216661,-123.57650841704,176.450943147388));
#32577=CARTESIAN_POINT('Ctrl Pts',(-57.083937866281,-123.547867676478,176.046918584679));
#32578=CARTESIAN_POINT('Ctrl Pts',(-57.1657781595267,-123.479090314682,
175.264080212427));
#32579=CARTESIAN_POINT('Ctrl Pts',(-57.2790359397733,-123.435968764243,
174.89213178999));
#32580=CARTESIAN_POINT('Ctrl Pts',(-57.6464709704613,-123.332098044232,
174.199849946451));
#32581=CARTESIAN_POINT('Ctrl Pts',(-57.9022024034783,-123.272073484604,
173.889126732894));
#32582=CARTESIAN_POINT('Ctrl Pts',(-58.2201117923249,-123.206701538053,
173.631812975112));
#32583=CARTESIAN_POINT('Ctrl Pts',(-58.2289048175451,-123.204899387046,
173.624779151223));
#32584=CARTESIAN_POINT('Ctrl Pts',(-58.237735556893,-123.203095437391,173.617797875548));
#32585=CARTESIAN_POINT('Origin',(-54.1598171290174,-67.5719248685924,175.985485069079));
#32586=CARTESIAN_POINT('',(-58.0257235479966,-121.214364458077,173.617797875548));
#32587=CARTESIAN_POINT('',(-58.0787265502207,-121.711547202905,173.617797875548));
#32588=CARTESIAN_POINT('',(-52.327900808713,-67.7672193871761,173.617797875548));
#32589=CARTESIAN_POINT('Ctrl Pts',(-58.0257235479965,-121.214364458077,
173.617797875548));
#32590=CARTESIAN_POINT('Ctrl Pts',(-57.8910902662336,-121.241867439718,
173.724234269834));
#32591=CARTESIAN_POINT('Ctrl Pts',(-57.7656471951412,-121.268865446389,
173.842545061126));
#32592=CARTESIAN_POINT('Ctrl Pts',(-57.3903884722706,-121.354511789475,
174.264562857379));
#32593=CARTESIAN_POINT('Ctrl Pts',(-57.1901588288744,-121.408625641651,
174.607097380125));
#32594=CARTESIAN_POINT('Ctrl Pts',(-56.9363076872888,-121.498868093884,
175.343114408043));
#32595=CARTESIAN_POINT('Ctrl Pts',(-56.8815900839742,-121.533146279122,
175.728280734596));
#32596=CARTESIAN_POINT('Ctrl Pts',(-56.9214577980342,-121.591449874668,
176.509097195586));
#32597=CARTESIAN_POINT('Ctrl Pts',(-57.0192951420369,-121.613803657037,
176.89702240998));
#32598=CARTESIAN_POINT('Ctrl Pts',(-57.3548253195761,-121.641290023581,
177.604904883751));
#32599=CARTESIAN_POINT('Ctrl Pts',(-57.5857160543015,-121.645137650408,
177.919643118704));
#32600=CARTESIAN_POINT('Ctrl Pts',(-58.1614516226242,-121.646225356556,
178.451906240832));
#32601=CARTESIAN_POINT('Ctrl Pts',(-58.503295822017,-121.642580716861,178.661411828903));
#32602=CARTESIAN_POINT('Ctrl Pts',(-59.2386444508246,-121.627517586945,
178.932744590103));
#32603=CARTESIAN_POINT('Ctrl Pts',(-59.6235445743797,-121.614971454751,
178.995662154724));
#32604=CARTESIAN_POINT('Ctrl Pts',(-60.4070754139044,-121.593817885247,
178.972324662672));
#32605=CARTESIAN_POINT('Ctrl Pts',(-60.7979355978628,-121.584960646956,
178.882235457376));
#32606=CARTESIAN_POINT('Ctrl Pts',(-61.5127413959487,-121.57215913929,178.560288614066));
#32607=CARTESIAN_POINT('Ctrl Pts',(-61.8313235414465,-121.566714699417,
178.335269783198));
#32608=CARTESIAN_POINT('Ctrl Pts',(-62.3745155498307,-121.57109409288,177.769590456732));
#32609=CARTESIAN_POINT('Ctrl Pts',(-62.5907877898474,-121.580860453187,
177.431512229467));
#32610=CARTESIAN_POINT('Ctrl Pts',(-62.8762946514684,-121.613894393029,
176.701887873391));
#32611=CARTESIAN_POINT('Ctrl Pts',(-62.9465577724403,-121.634960807152,
176.318893024691));
#32612=CARTESIAN_POINT('Ctrl Pts',(-62.9396479590941,-121.697896378297,
175.537075933605));
#32613=CARTESIAN_POINT('Ctrl Pts',(-62.8581926713311,-121.73941240673,175.145919171686));
#32614=CARTESIAN_POINT('Ctrl Pts',(-62.553222792541,-121.835462033537,174.429720497847));
#32615=CARTESIAN_POINT('Ctrl Pts',(-62.3364713059894,-121.887170647192,
174.109825587998));
#32616=CARTESIAN_POINT('Ctrl Pts',(-61.7869816303679,-122.007861169625,
173.563074998768));
#32617=CARTESIAN_POINT('Ctrl Pts',(-61.4564544944988,-122.075938466264,
173.344736476158));
#32618=CARTESIAN_POINT('Ctrl Pts',(-60.7407356703104,-122.215841139421,
173.055634861287));
#32619=CARTESIAN_POINT('Ctrl Pts',(-60.3639329205162,-122.284662414731,
172.983479930204));
#32620=CARTESIAN_POINT('Ctrl Pts',(-59.592681777914,-122.428907413695,172.987637390073));
#32621=CARTESIAN_POINT('Ctrl Pts',(-59.2057579301147,-122.50300420502,173.068519815426));
#32622=CARTESIAN_POINT('Ctrl Pts',(-58.6089227159464,-122.620202316533,
173.325384475355));
#32623=CARTESIAN_POINT('Ctrl Pts',(-58.3868146007374,-122.664631229834,
173.458038831931));
#32624=CARTESIAN_POINT('Ctrl Pts',(-58.1847325546681,-122.705912692563,
173.617797875548));
#32625=CARTESIAN_POINT('Ctrl Pts',(-58.237735556893,-123.203095437391,173.617797875548));
#32626=CARTESIAN_POINT('Ctrl Pts',(-58.5287732638245,-123.143642049596,
173.387713577509));
#32627=CARTESIAN_POINT('Ctrl Pts',(-58.8600551027551,-123.077925256269,
173.214905046944));
#32628=CARTESIAN_POINT('Ctrl Pts',(-59.5938757045305,-122.935930027545,
172.994750145778));
#32629=CARTESIAN_POINT('Ctrl Pts',(-59.9921699206112,-122.86070731422,172.959344196458));
#32630=CARTESIAN_POINT('Ctrl Pts',(-60.7642674135403,-122.718343804205,
173.04800912509));
#32631=CARTESIAN_POINT('Ctrl Pts',(-61.1308479744597,-122.64821655548,173.165197421926));
#32632=CARTESIAN_POINT('Ctrl Pts',(-61.8124112746046,-122.510857712428,
173.541568250379));
#32633=CARTESIAN_POINT('Ctrl Pts',(-62.1179318564219,-122.445525279102,
173.802219455678));
#32634=CARTESIAN_POINT('Ctrl Pts',(-62.5996928940023,-122.334113508502,
174.418463488186));
#32635=CARTESIAN_POINT('Ctrl Pts',(-62.7755494132449,-122.284318829716,
174.764335005319));
#32636=CARTESIAN_POINT('Ctrl Pts',(-62.9908577990156,-122.196665902924,
175.519986912537));
#32637=CARTESIAN_POINT('Ctrl Pts',(-63.0226137435619,-122.160518599003,
175.924010439495));
#32638=CARTESIAN_POINT('Ctrl Pts',(-62.9281241062413,-122.110538928769,
176.706849062437));
#32639=CARTESIAN_POINT('Ctrl Pts',(-62.8083263219376,-122.092263095387,
177.078798662381));
#32640=CARTESIAN_POINT('Ctrl Pts',(-62.4272617866629,-122.06818753574,177.771084912746));
#32641=CARTESIAN_POINT('Ctrl Pts',(-62.164628442723,-122.063424086087,178.081811446834));
#32642=CARTESIAN_POINT('Ctrl Pts',(-61.5455308511229,-122.069371051784,
178.572672856614));
#32643=CARTESIAN_POINT('Ctrl Pts',(-61.1983372190016,-122.075337265567,
178.752819702656));
#32644=CARTESIAN_POINT('Ctrl Pts',(-60.440125560244,-122.091468140645,178.976212692936));
#32645=CARTESIAN_POINT('Ctrl Pts',(-60.0349257541581,-122.101903216854,
179.011624891001));
#32646=CARTESIAN_POINT('Ctrl Pts',(-59.2501677735642,-122.12551060413,178.922972556315));
#32647=CARTESIAN_POINT('Ctrl Pts',(-58.8770405971546,-122.134241647429,
178.805790433108));
#32648=CARTESIAN_POINT('Ctrl Pts',(-58.1818324291849,-122.143655963546,
178.429431594332));
#32649=CARTESIAN_POINT('Ctrl Pts',(-57.8694012443158,-122.144201272616,
178.168786052508));
#32650=CARTESIAN_POINT('Ctrl Pts',(-57.3749702478911,-122.136857774846,
177.552551377356));
#32651=CARTESIAN_POINT('Ctrl Pts',(-57.1925627966907,-122.125256972299,
177.206683519448));
#32652=CARTESIAN_POINT('Ctrl Pts',(-56.9636016969033,-122.084966272651,
176.451036853763));
#32653=CARTESIAN_POINT('Ctrl Pts',(-56.9249317787034,-122.056326788452,
176.047014712842));
#32654=CARTESIAN_POINT('Ctrl Pts',(-57.0067466966813,-121.987551530768,
175.264175754574));
#32655=CARTESIAN_POINT('Ctrl Pts',(-57.1199921765401,-121.944432312985,
174.892224579027));
#32656=CARTESIAN_POINT('Ctrl Pts',(-57.4874031359341,-121.840564406947,
174.199932432095));
#32657=CARTESIAN_POINT('Ctrl Pts',(-57.7431231767648,-121.780540972055,
173.889201454985));
#32658=CARTESIAN_POINT('Ctrl Pts',(-58.061049255969,-121.715164274657,173.631855795998));
#32659=CARTESIAN_POINT('Ctrl Pts',(-58.0698689309023,-121.71335664362,173.624800401594));
#32660=CARTESIAN_POINT('Ctrl Pts',(-58.0787265502207,-121.711547202905,
173.617797875548));
#32661=CARTESIAN_POINT('Origin',(-54.1598171290174,-67.5719248685924,175.985485069079));
#32662=CARTESIAN_POINT('',(-57.8667145413245,-119.722816223591,173.617797875548));
#32663=CARTESIAN_POINT('',(-57.9197175435485,-120.21999896842,173.617797875548));
#32664=CARTESIAN_POINT('',(-52.327900808713,-67.7672193871761,173.617797875548));
#32665=CARTESIAN_POINT('Ctrl Pts',(-57.8667145413246,-119.722816223591,
173.617797875548));
#32666=CARTESIAN_POINT('Ctrl Pts',(-57.6914471639414,-119.758619966911,
173.756358173866));
#32667=CARTESIAN_POINT('Ctrl Pts',(-57.532019262434,-119.793513567425,173.914828966194));
#32668=CARTESIAN_POINT('Ctrl Pts',(-57.1465332178751,-119.884996020418,
174.397186504441));
#32669=CARTESIAN_POINT('Ctrl Pts',(-56.9642747443631,-119.937213881699,
174.750270474763));
#32670=CARTESIAN_POINT('Ctrl Pts',(-56.7491012600445,-120.022682791733,
175.499327684857));
#32671=CARTESIAN_POINT('Ctrl Pts',(-56.7145927550832,-120.054810410505,
175.886962757056));
#32672=CARTESIAN_POINT('Ctrl Pts',(-56.7952337262314,-120.10941431512,176.664685479809));
#32673=CARTESIAN_POINT('Ctrl Pts',(-56.9130994766506,-120.129621476025,
177.046922740441));
#32674=CARTESIAN_POINT('Ctrl Pts',(-57.2850225644234,-120.152590512418,
177.736662194168));
#32675=CARTESIAN_POINT('Ctrl Pts',(-57.5322239088185,-120.154674458871,
178.039183324876));
#32676=CARTESIAN_POINT('Ctrl Pts',(-58.1347931906971,-120.153559985664,
178.540318042894));
#32677=CARTESIAN_POINT('Ctrl Pts',(-58.4864450863061,-120.148827001235,
178.731408524917));
#32678=CARTESIAN_POINT('Ctrl Pts',(-59.2347724041748,-120.13175680159,178.964298242534));
#32679=CARTESIAN_POINT('Ctrl Pts',(-59.623093824967,-120.11879287224,179.007120014528));
#32680=CARTESIAN_POINT('Ctrl Pts',(-60.403856401275,-120.098602649356,178.942741236308));
#32681=CARTESIAN_POINT('Ctrl Pts',(-60.7883583544615,-120.09034912906,178.832846215453));
#32682=CARTESIAN_POINT('Ctrl Pts',(-61.4855725740688,-120.078815064133,
178.474746987524));
#32683=CARTESIAN_POINT('Ctrl Pts',(-61.7929159484235,-120.074488583628,
178.232888600283));
#32684=CARTESIAN_POINT('Ctrl Pts',(-62.3054851758825,-120.082808761327,
177.640193174294));
#32685=CARTESIAN_POINT('Ctrl Pts',(-62.5032680503643,-120.094440744594,
177.293029773678));
#32686=CARTESIAN_POINT('Ctrl Pts',(-62.7514324671375,-120.130869850592,
176.550300113879));
#32687=CARTESIAN_POINT('Ctrl Pts',(-62.8021576249081,-120.153918370995,
176.162849262917));
#32688=CARTESIAN_POINT('Ctrl Pts',(-62.7547694302776,-120.221872828282,
175.383368750423));
#32689=CARTESIAN_POINT('Ctrl Pts',(-62.6540228035417,-120.265324439071,
174.999075580255));
#32690=CARTESIAN_POINT('Ctrl Pts',(-62.3138754992907,-120.364527975419,
174.300125140517));
#32691=CARTESIAN_POINT('Ctrl Pts',(-62.0803823928511,-120.417860930305,
173.990833581451));
#32692=CARTESIAN_POINT('Ctrl Pts',(-61.5041786598013,-120.542104915372,
173.474093635012));
#32693=CARTESIAN_POINT('Ctrl Pts',(-61.1648286858917,-120.611013630438,
173.274035009477));
#32694=CARTESIAN_POINT('Ctrl Pts',(-60.4364022663505,-120.751691527133,
173.021589071245));
#32695=CARTESIAN_POINT('Ctrl Pts',(-60.0552761315911,-120.820756285235,
172.968535643119));
#32696=CARTESIAN_POINT('Ctrl Pts',(-59.2860945509954,-120.965486127467,
173.012361011038));
#32697=CARTESIAN_POINT('Ctrl Pts',(-58.9055699766426,-121.0388032346,173.112192942474));
#32698=CARTESIAN_POINT('Ctrl Pts',(-58.3671317600356,-121.145242801056,
173.376173693532));
#32699=CARTESIAN_POINT('Ctrl Pts',(-58.1897246329056,-121.18086220092,173.488144316575));
#32700=CARTESIAN_POINT('Ctrl Pts',(-58.0257235479965,-121.214364458077,
173.617797875548));
#32701=CARTESIAN_POINT('Ctrl Pts',(-58.0787265502207,-121.711547202905,
173.617797875548));
#32702=CARTESIAN_POINT('Ctrl Pts',(-58.3697361321289,-121.65209956051,173.387735812175));
#32703=CARTESIAN_POINT('Ctrl Pts',(-58.7009823964628,-121.586389655514,
173.214938163782));
#32704=CARTESIAN_POINT('Ctrl Pts',(-59.4347598575272,-121.444402137507,
172.994767213526));
#32705=CARTESIAN_POINT('Ctrl Pts',(-59.833051277686,-121.369179625724,172.959346654237));
#32706=CARTESIAN_POINT('Ctrl Pts',(-60.6051493712523,-121.22681535641,173.047982137366));
#32707=CARTESIAN_POINT('Ctrl Pts',(-60.9717332234154,-121.156688938203,
173.165155999873));
#32708=CARTESIAN_POINT('Ctrl Pts',(-61.6533084049214,-121.019329115187,
173.541498795707));
#32709=CARTESIAN_POINT('Ctrl Pts',(-61.9588379055462,-120.953995627252,
173.802136759374));
#32710=CARTESIAN_POINT('Ctrl Pts',(-62.4406216441401,-120.842580688804,
174.418358913714));
#32711=CARTESIAN_POINT('Ctrl Pts',(-62.6164916211797,-120.792785845895,
174.764221875393));
#32712=CARTESIAN_POINT('Ctrl Pts',(-62.831830251157,-120.705130003192,175.519861527492));
#32713=CARTESIAN_POINT('Ctrl Pts',(-62.8636029886591,-120.668980797393,
175.923881813629));
#32714=CARTESIAN_POINT('Ctrl Pts',(-62.7691471355156,-120.618996721308,
176.706721220368));
#32715=CARTESIAN_POINT('Ctrl Pts',(-62.6493660979336,-120.60072046909,177.078674504138));
#32716=CARTESIAN_POINT('Ctrl Pts',(-62.2683338413584,-120.576641799933,
177.770974540679));
#32717=CARTESIAN_POINT('Ctrl Pts',(-62.0057157156663,-120.571876607854,
178.081711462514));
#32718=CARTESIAN_POINT('Ctrl Pts',(-61.386643197741,-120.577820035574,178.572599371752));
#32719=CARTESIAN_POINT('Ctrl Pts',(-61.0394595611544,-120.583786653381,
178.752761717307));
#32720=CARTESIAN_POINT('Ctrl Pts',(-60.2812620362002,-120.599916378367,
178.976189852383));
#32721=CARTESIAN_POINT('Ctrl Pts',(-59.8760659443662,-120.610350929496,
179.011621599123));
#32722=CARTESIAN_POINT('Ctrl Pts',(-59.0913069644141,-120.633957493048,
178.923008663735));
#32723=CARTESIAN_POINT('Ctrl Pts',(-58.7181757174253,-120.642690550831,
178.805845854155));
#32724=CARTESIAN_POINT('Ctrl Pts',(-58.0229517331321,-120.65210693668,178.429524524002));
#32725=CARTESIAN_POINT('Ctrl Pts',(-57.710508585761,-120.65265338218,178.168896700149));
#32726=CARTESIAN_POINT('Ctrl Pts',(-57.2160470041594,-120.645312144498,
177.552691298977));
#32727=CARTESIAN_POINT('Ctrl Pts',(-57.0336219045084,-120.633714923204,
177.206834888442));
#32728=CARTESIAN_POINT('Ctrl Pts',(-56.8046204246826,-120.593428940922,
176.451204620774));
#32729=CARTESIAN_POINT('Ctrl Pts',(-56.7659280058564,-120.564791706116,
176.047186816681));
#32730=CARTESIAN_POINT('Ctrl Pts',(-56.8476974932369,-120.496020215608,
175.26434681027));
#32731=CARTESIAN_POINT('Ctrl Pts',(-56.9609209512799,-120.452905173578,
174.892390705729));
#32732=CARTESIAN_POINT('Ctrl Pts',(-57.3282888150645,-120.34904230557,174.200080113435));
#32733=CARTESIAN_POINT('Ctrl Pts',(-57.5839884596258,-120.289020884472,
173.889335238043));
#32734=CARTESIAN_POINT('Ctrl Pts',(-57.9019444156091,-120.223635681883,
173.631932461655));
#32735=CARTESIAN_POINT('Ctrl Pts',(-57.9108118003911,-120.221818239906,
173.624838446629));
#32736=CARTESIAN_POINT('Ctrl Pts',(-57.9197175435485,-120.21999896842,173.617797875548));
#32737=CARTESIAN_POINT('Origin',(-54.1598171290174,-67.5719248685924,175.985485069079));
#32738=CARTESIAN_POINT('',(-57.7077055346527,-118.231267989106,173.617797875547));
#32739=CARTESIAN_POINT('',(-57.7607085368763,-118.728450733934,173.617797875548));
#32740=CARTESIAN_POINT('',(-52.327900808713,-67.7672193871761,173.617797875548));
#32741=CARTESIAN_POINT('Ctrl Pts',(-57.7077055346532,-118.231267989105,
173.617797875547));
#32742=CARTESIAN_POINT('Ctrl Pts',(-57.4959621896365,-118.274523068789,
173.785194806399));
#32743=CARTESIAN_POINT('Ctrl Pts',(-57.3076732924635,-118.316380953857,
173.981384137499));
#32744=CARTESIAN_POINT('Ctrl Pts',(-56.9166317085334,-118.412777038229,
174.520832622239));
#32745=CARTESIAN_POINT('Ctrl Pts',(-56.750514647398,-118.463346246606,174.884149145073));
#32746=CARTESIAN_POINT('Ctrl Pts',(-56.5714891759017,-118.544263785547,
175.644138037827));
#32747=CARTESIAN_POINT('Ctrl Pts',(-56.5556667163322,-118.574733608663,
176.032265300035));
#32748=CARTESIAN_POINT('Ctrl Pts',(-56.6733470037069,-118.625927257235,
176.806552565876));
#32749=CARTESIAN_POINT('Ctrl Pts',(-56.810230408708,-118.644190079599,177.184578227962));
#32750=CARTESIAN_POINT('Ctrl Pts',(-57.2161301513622,-118.662834557244,
177.856022857159));
#32751=CARTESIAN_POINT('Ctrl Pts',(-57.4771708165094,-118.663728203223,
178.145359811132));
#32752=CARTESIAN_POINT('Ctrl Pts',(-58.1040538177718,-118.660578695295,
178.617304601394));
#32753=CARTESIAN_POINT('Ctrl Pts',(-58.4664849731559,-118.65479096,178.791666699017));
#32754=CARTESIAN_POINT('Ctrl Pts',(-59.2262807590043,-118.635793046171,
178.98675832149));
#32755=CARTESIAN_POINT('Ctrl Pts',(-59.6151252160864,-118.623005534561,
179.010088454037));
#32756=CARTESIAN_POINT('Ctrl Pts',(-60.3926306750729,-118.603737382819,
178.907203912237));
#32757=CARTESIAN_POINT('Ctrl Pts',(-60.7730525089593,-118.596024833953,
178.777492732011));
#32758=CARTESIAN_POINT('Ctrl Pts',(-61.4515994433801,-118.585775083933,
178.383836348125));
#32759=CARTESIAN_POINT('Ctrl Pts',(-61.7453936668036,-118.583069027208,
178.127620143533));
#32760=CARTESIAN_POINT('Ctrl Pts',(-62.2282783918895,-118.595145616927,
177.509631408275));
#32761=CARTESIAN_POINT('Ctrl Pts',(-62.4090968626334,-118.608703934463,
177.151113681912));
#32762=CARTESIAN_POINT('Ctrl Pts',(-62.6185406180347,-118.648551184006,
176.39623447214));
#32763=CARTESIAN_POINT('Ctrl Pts',(-62.6493280119049,-118.673837331507,
176.008347577506));
#32764=CARTESIAN_POINT('Ctrl Pts',(-62.5628115219606,-118.746549626409,
175.232305764503));
#32765=CARTESIAN_POINT('Ctrl Pts',(-62.4419634897019,-118.792258059477,
174.8521407814));
#32766=CARTESIAN_POINT('Ctrl Pts',(-62.0654492724426,-118.894660541694,
174.171798112607));
#32767=CARTESIAN_POINT('Ctrl Pts',(-61.8170828921811,-118.949666263393,
173.876129109712));
#32768=CARTESIAN_POINT('Ctrl Pts',(-61.2152216894388,-119.077249068476,
173.390024925554));
#32769=CARTESIAN_POINT('Ctrl Pts',(-60.8648129210778,-119.147419241121,
173.207514866718));
#32770=CARTESIAN_POINT('Ctrl Pts',(-60.1235724595637,-119.288792655129,
172.994139736444));
#32771=CARTESIAN_POINT('Ctrl Pts',(-59.7409990374732,-119.358072166465,
172.9613972216));
#32772=CARTESIAN_POINT('Ctrl Pts',(-58.975156012803,-119.503065519046,173.045611951922));
#32773=CARTESIAN_POINT('Ctrl Pts',(-58.5995443177483,-119.575910058344,
173.165726609417));
#32774=CARTESIAN_POINT('Ctrl Pts',(-58.1205711238936,-119.671308320629,
173.433040081355));
#32775=CARTESIAN_POINT('Ctrl Pts',(-57.9898008994096,-119.697672055653,
173.520490077886));
#32776=CARTESIAN_POINT('Ctrl Pts',(-57.8667145413246,-119.722816223591,
173.617797875548));
#32777=CARTESIAN_POINT('Ctrl Pts',(-57.9197175435485,-120.21999896842,173.617797875548));
#32778=CARTESIAN_POINT('Ctrl Pts',(-58.2106767735707,-120.160561611943,
173.387775618626));
#32779=CARTESIAN_POINT('Ctrl Pts',(-58.5418593508223,-120.09486403879,173.214997455317));
#32780=CARTESIAN_POINT('Ctrl Pts',(-59.2755595770514,-119.952890325441,
172.99479777958));
#32781=CARTESIAN_POINT('Ctrl Pts',(-59.6738459904375,-119.877668174723,
172.959351064575));
#32782=CARTESIAN_POINT('Ctrl Pts',(-60.4459451579516,-119.735302546304,
173.047933832021));
#32783=CARTESIAN_POINT('Ctrl Pts',(-60.8125349022444,-119.665177614304,
173.165081853359));
#32784=CARTESIAN_POINT('Ctrl Pts',(-61.494131352967,-119.527816037166,173.54137446353));
#32785=CARTESIAN_POINT('Ctrl Pts',(-61.7996768191756,-119.462480661484,
173.801988720596));
#32786=CARTESIAN_POINT('Ctrl Pts',(-62.2815011969325,-119.35106005207,174.418171706624));
#32787=CARTESIAN_POINT('Ctrl Pts',(-62.4573952662902,-119.30126491461,174.764019352204));
#32788=CARTESIAN_POINT('Ctrl Pts',(-62.6727880387899,-119.213603852045,
175.519637063711));
#32789=CARTESIAN_POINT('Ctrl Pts',(-62.7045908387443,-119.177451241683,
175.923651546385));
#32790=CARTESIAN_POINT('Ctrl Pts',(-62.6101954659949,-119.127459278395,
176.706492354431));
#32791=CARTESIAN_POINT('Ctrl Pts',(-62.490444407855,-119.109182275538,177.078452232915));
#32792=CARTESIAN_POINT('Ctrl Pts',(-62.1094699358185,-119.085098039957,
177.770776947088));
#32793=CARTESIAN_POINT('Ctrl Pts',(-61.8468790543294,-119.08032972871,178.081532462913));
#32794=CARTESIAN_POINT('Ctrl Pts',(-61.2278514236408,-119.086266822916,
178.572467808727));
#32795=CARTESIAN_POINT('Ctrl Pts',(-60.8806856801912,-119.092234162999,
178.752657900388));
#32796=CARTESIAN_POINT('Ctrl Pts',(-60.1225134582295,-119.108361829161,
178.976148947484));
#32797=CARTESIAN_POINT('Ctrl Pts',(-59.717324017646,-119.118795440289,179.011615688008));
#32798=CARTESIAN_POINT('Ctrl Pts',(-58.9325632512169,-119.14240052922,178.92307328148));
#32799=CARTESIAN_POINT('Ctrl Pts',(-58.5594247174237,-119.151137191948,
178.805945044747));
#32800=CARTESIAN_POINT('Ctrl Pts',(-57.8641724234153,-119.160557282684,
178.429690857934));
#32801=CARTESIAN_POINT('Ctrl Pts',(-57.5517078647856,-119.161105762437,
178.169094751776));
#32802=CARTESIAN_POINT('Ctrl Pts',(-57.0571915361592,-119.15376857044,177.552941754575));
#32803=CARTESIAN_POINT('Ctrl Pts',(-56.8747348452426,-119.142177758356,
177.20710583504));
#32804=CARTESIAN_POINT('Ctrl Pts',(-56.6456610864564,-119.101900220253,
176.451504922429));
#32805=CARTESIAN_POINT('Ctrl Pts',(-56.6069283921423,-119.073267012053,
176.047494884375));
#32806=CARTESIAN_POINT('Ctrl Pts',(-56.6886165589738,-119.004502265035,
175.264653005099));
#32807=CARTESIAN_POINT('Ctrl Pts',(-56.8018005986401,-118.961394695927,
174.892688077791));
#32808=CARTESIAN_POINT('Ctrl Pts',(-57.1690913228373,-118.857540846071,
174.200344472601));
#32809=CARTESIAN_POINT('Ctrl Pts',(-57.4247544572965,-118.797523030058,
173.88957472317));
#32810=CARTESIAN_POINT('Ctrl Pts',(-57.7427638772072,-118.732122604775,
173.632069696993));
#32811=CARTESIAN_POINT('Ctrl Pts',(-57.7517166545312,-118.730287601994,
173.624906545277));
#32812=CARTESIAN_POINT('Ctrl Pts',(-57.7607085368763,-118.728450733934,
173.617797875548));
#32813=CARTESIAN_POINT('Origin',(-54.1598171290174,-67.5719248685924,175.985485069079));
#32814=CARTESIAN_POINT('',(-57.5486965279805,-116.73971975462,173.617797875547));
#32815=CARTESIAN_POINT('',(-57.601699530204,-117.236902499449,173.617797875548));
#32816=CARTESIAN_POINT('',(-52.327900808713,-67.7672193871761,173.617797875548));
#32817=CARTESIAN_POINT('Ctrl Pts',(-57.548696527981,-116.73971975462,173.617797875547));
#32818=CARTESIAN_POINT('Ctrl Pts',(-57.3083599148635,-116.788815887254,
173.807799650592));
#32819=CARTESIAN_POINT('Ctrl Pts',(-57.0985524074229,-116.836048388882,
174.034651071404));
#32820=CARTESIAN_POINT('Ctrl Pts',(-56.7063045242392,-116.935899466992,
174.619800438034));
#32821=CARTESIAN_POINT('Ctrl Pts',(-56.5531790359681,-116.985088492272,
174.990610114756));
#32822=CARTESIAN_POINT('Ctrl Pts',(-56.4026615921244,-117.062366679206,
175.758523970475));
#32823=CARTESIAN_POINT('Ctrl Pts',(-56.4015627571165,-117.091838693313,
176.147067054867));
#32824=CARTESIAN_POINT('Ctrl Pts',(-56.5486985717973,-117.140272647945,
176.91801861918));
#32825=CARTESIAN_POINT('Ctrl Pts',(-56.7006082724247,-117.156944551056,
177.292024778325));
#32826=CARTESIAN_POINT('Ctrl Pts',(-57.133243173484,-117.172121812282,177.948259104063));
#32827=CARTESIAN_POINT('Ctrl Pts',(-57.4054042916933,-117.172387581818,
178.227077251624));
#32828=CARTESIAN_POINT('Ctrl Pts',(-58.0515087032864,-117.167588897825,
178.674943552142));
#32829=CARTESIAN_POINT('Ctrl Pts',(-58.4220892300848,-117.160950207667,
178.835329306316));
#32830=CARTESIAN_POINT('Ctrl Pts',(-59.1904533167627,-117.140405969468,
178.99954710651));
#32831=CARTESIAN_POINT('Ctrl Pts',(-59.5797920359974,-117.128104936031,
179.007024670633));
#32832=CARTESIAN_POINT('Ctrl Pts',(-60.3539318250452,-117.109615318493,
178.872415935096));
#32833=CARTESIAN_POINT('Ctrl Pts',(-60.7302326391108,-117.102367420638,
178.726472928545));
#32834=CARTESIAN_POINT('Ctrl Pts',(-61.3926513698913,-117.093189541362,
178.303843026263));
#32835=CARTESIAN_POINT('Ctrl Pts',(-61.6752938263682,-117.092188612567,
178.035719473275));
#32836=CARTESIAN_POINT('Ctrl Pts',(-62.1327621306332,-117.107414460568,
177.397017325779));
#32837=CARTESIAN_POINT('Ctrl Pts',(-62.2988430834852,-117.122577373761,
177.029604538182));
#32838=CARTESIAN_POINT('Ctrl Pts',(-62.4754944817019,-117.165259733133,
176.265275719895));
#32839=CARTESIAN_POINT('Ctrl Pts',(-62.4895199837143,-117.192821668892,
175.876927760014));
#32840=CARTESIAN_POINT('Ctrl Pts',(-62.3694967178749,-117.269565760154,
175.10436597572));
#32841=CARTESIAN_POINT('Ctrl Pts',(-62.2314564271143,-117.317149273094,
174.728426354695));
#32842=CARTESIAN_POINT('Ctrl Pts',(-61.8241467766779,-117.422162195221,
174.065080856857));
#32843=CARTESIAN_POINT('Ctrl Pts',(-61.5632570996869,-117.478959868437,
173.781389383671));
#32844=CARTESIAN_POINT('Ctrl Pts',(-60.9395057722688,-117.609356080022,
173.322282674548));
#32845=CARTESIAN_POINT('Ctrl Pts',(-60.5795755617375,-117.680592973706,
173.155355436889));
#32846=CARTESIAN_POINT('Ctrl Pts',(-59.8281154054219,-117.822373149151,
172.97675877957));
#32847=CARTESIAN_POINT('Ctrl Pts',(-59.4451103376711,-117.892119058604,
172.961902562141));
#32848=CARTESIAN_POINT('Ctrl Pts',(-58.6827834569909,-118.037237208823,
173.081704619415));
#32849=CARTESIAN_POINT('Ctrl Pts',(-58.3114025141392,-118.109692363721,
173.220085431791));
#32850=CARTESIAN_POINT('Ctrl Pts',(-57.8840410361413,-118.195417984603,
173.486217673092));
#32851=CARTESIAN_POINT('Ctrl Pts',(-57.7939584776156,-118.213648177156,
173.549609295983));
#32852=CARTESIAN_POINT('Ctrl Pts',(-57.7077055346532,-118.231267989105,
173.617797875547));
#32853=CARTESIAN_POINT('Ctrl Pts',(-57.7607085368762,-118.728450733934,
173.617797875548));
#32854=CARTESIAN_POINT('Ctrl Pts',(-58.0515776428276,-118.669031788066,
173.387846867585));
#32855=CARTESIAN_POINT('Ctrl Pts',(-58.3826462329409,-118.603356286683,
173.215103589513));
#32856=CARTESIAN_POINT('Ctrl Pts',(-59.1162082159644,-118.461407282903,
172.994852520928));
#32857=CARTESIAN_POINT('Ctrl Pts',(-59.5144856637423,-118.38618577923,172.959358991275));
#32858=CARTESIAN_POINT('Ctrl Pts',(-60.2865867491216,-118.243817719005,
173.047847404498));
#32859=CARTESIAN_POINT('Ctrl Pts',(-60.653187039188,-118.173695445026,173.164949174507));
#32860=CARTESIAN_POINT('Ctrl Pts',(-61.3348215534645,-118.036330729164,
173.541151960673));
#32861=CARTESIAN_POINT('Ctrl Pts',(-61.640395590947,-117.970991975614,173.801723784791));
#32862=CARTESIAN_POINT('Ctrl Pts',(-62.1222927011249,-117.859561217089,
174.417836663756));
#32863=CARTESIAN_POINT('Ctrl Pts',(-62.2982298897146,-117.809765550101,
174.763656897282));
#32864=CARTESIAN_POINT('Ctrl Pts',(-62.5137195604792,-117.72209514605,175.519235336379));
#32865=CARTESIAN_POINT('Ctrl Pts',(-62.5455761630827,-117.685936443013,
175.923239426838));
#32866=CARTESIAN_POINT('Ctrl Pts',(-62.4512890336388,-117.635930364266,
176.706082736919));
#32867=CARTESIAN_POINT('Ctrl Pts',(-62.3315916288074,-117.617652015292,
177.078054417928));
#32868=CARTESIAN_POINT('Ctrl Pts',(-61.9507205728282,-117.593557818036,
177.770423290715));
#32869=CARTESIAN_POINT('Ctrl Pts',(-61.6881784526301,-117.588783924713,
178.081212077816));
#32870=CARTESIAN_POINT('Ctrl Pts',(-61.0692311589717,-117.594709684208,
178.572232313359));
#32871=CARTESIAN_POINT('Ctrl Pts',(-60.7220974365814,-117.600678313742,
178.752472059403));
#32872=CARTESIAN_POINT('Ctrl Pts',(-59.9639705021903,-117.616802295402,
178.976075688442));
#32873=CARTESIAN_POINT('Ctrl Pts',(-59.5587929719279,-117.627234224161,
179.011605051095));
#32874=CARTESIAN_POINT('Ctrl Pts',(-58.7740290164334,-117.650836673956,
178.923188859954));
#32875=CARTESIAN_POINT('Ctrl Pts',(-58.4008774423528,-117.659579784133,
178.806122491485));
#32876=CARTESIAN_POINT('Ctrl Pts',(-57.7055744966176,-117.669006504483,
178.429988458243));
#32877=CARTESIAN_POINT('Ctrl Pts',(-57.3930716305156,-117.669558624411,
178.16944911486));
#32878=CARTESIAN_POINT('Ctrl Pts',(-56.8984573406303,-117.662228672049,
177.553389899095));
#32879=CARTESIAN_POINT('Ctrl Pts',(-56.7159441195295,-117.650649324458,
177.207590646192));
#32880=CARTESIAN_POINT('Ctrl Pts',(-56.486741031144,-117.610386896422,176.452042268985));
#32881=CARTESIAN_POINT('Ctrl Pts',(-56.4479362711177,-117.581760893924,
176.048046137231));
#32882=CARTESIAN_POINT('Ctrl Pts',(-56.5294789261214,-117.513008214282,
175.265200917308));
#32883=CARTESIAN_POINT('Ctrl Pts',(-56.6425924338899,-117.469914011628,
174.893220203229));
#32884=CARTESIAN_POINT('Ctrl Pts',(-57.0097451318139,-117.366076298834,
174.200817539525));
#32885=CARTESIAN_POINT('Ctrl Pts',(-57.2653429337035,-117.306064934913,
173.890003293683));
#32886=CARTESIAN_POINT('Ctrl Pts',(-57.58344797069,-117.240637275718,173.63231527396));
#32887=CARTESIAN_POINT('Ctrl Pts',(-57.5925535209534,-117.238770852661,
173.625028392653));
#32888=CARTESIAN_POINT('Ctrl Pts',(-57.601699530204,-117.236902499449,173.617797875548));
#32889=CARTESIAN_POINT('Origin',(-54.1598171290174,-67.5719248685924,175.985485069079));
#32890=CARTESIAN_POINT('',(-57.389687521308,-115.248171520134,173.617797875548));
#32891=CARTESIAN_POINT('',(-57.4426905235318,-115.745354264963,173.617797875548));
#32892=CARTESIAN_POINT('',(-52.327900808713,-67.7672193871761,173.617797875548));
#32893=CARTESIAN_POINT('Ctrl Pts',(-57.3896875213082,-115.248171520134,
173.617797875547));
#32894=CARTESIAN_POINT('Ctrl Pts',(-57.1294513039164,-115.301332757948,
173.823531586255));
#32895=CARTESIAN_POINT('Ctrl Pts',(-56.9052436706449,-115.352261519648,
174.072290913891));
#32896=CARTESIAN_POINT('Ctrl Pts',(-56.5138092385919,-115.454302586941,
174.689656594133));
#32897=CARTESIAN_POINT('Ctrl Pts',(-56.3698913538831,-115.502486587136,
175.065402645794));
#32898=CARTESIAN_POINT('Ctrl Pts',(-56.2393156442174,-115.577193603871,
175.838505933654));
#32899=CARTESIAN_POINT('Ctrl Pts',(-56.2485300800921,-115.606126432242,
176.227354066961));
#32900=CARTESIAN_POINT('Ctrl Pts',(-56.4164065131603,-115.652591749473,
176.99563475266));
#32901=CARTESIAN_POINT('Ctrl Pts',(-56.5788247100044,-115.668121707705,
177.366458368768));
#32902=CARTESIAN_POINT('Ctrl Pts',(-57.0301337226059,-115.680842882183,
178.011634487482));
#32903=CARTESIAN_POINT('Ctrl Pts',(-57.31020217626,-115.680836901443,178.283012481517));
#32904=CARTESIAN_POINT('Ctrl Pts',(-57.9697747695641,-115.674859991022,
178.713444416283));
#32905=CARTESIAN_POINT('Ctrl Pts',(-58.3458441823813,-115.667616675278,
178.863635062624));
#32906=CARTESIAN_POINT('Ctrl Pts',(-59.1199365044752,-115.645976364494,
179.00566581141));
#32907=CARTESIAN_POINT('Ctrl Pts',(-59.5096679381343,-115.634213519229,
179.001762009582));
#32908=CARTESIAN_POINT('Ctrl Pts',(-60.2809866109783,-115.616298003549,
178.844193354825));
#32909=CARTESIAN_POINT('Ctrl Pts',(-60.653881599363,-115.609396381106,178.686581914147));
#32910=CARTESIAN_POINT('Ctrl Pts',(-61.3042109045463,-115.601001870185,
178.243163587925));
#32911=CARTESIAN_POINT('Ctrl Pts',(-61.5787705876214,-115.601449085696,
177.9663575889));
#32912=CARTESIAN_POINT('Ctrl Pts',(-62.0172788459717,-115.618985978262,
177.312741458275));
#32913=CARTESIAN_POINT('Ctrl Pts',(-62.1722693180302,-115.635317575529,
176.93918102279));
#32914=CARTESIAN_POINT('Ctrl Pts',(-62.3246579353953,-115.680061206192,
176.168372574323));
#32915=CARTESIAN_POINT('Ctrl Pts',(-62.3263274665632,-115.709530529282,
175.779662774806));
#32916=CARTESIAN_POINT('Ctrl Pts',(-62.1813255083139,-115.789244339945,
175.010147786758));
#32917=CARTESIAN_POINT('Ctrl Pts',(-62.0305522343798,-115.838175355501,
174.637857013707));
#32918=CARTESIAN_POINT('Ctrl Pts',(-61.6004962439435,-115.945068340475,
173.987671895184));
#32919=CARTESIAN_POINT('Ctrl Pts',(-61.3302278998166,-116.003456669163,
173.71294337057));
#32920=CARTESIAN_POINT('Ctrl Pts',(-60.6902452992533,-116.135907704359,
173.27462006307));
#32921=CARTESIAN_POINT('Ctrl Pts',(-60.3235454023058,-116.207860667075,
173.119808132163));
#32922=CARTESIAN_POINT('Ctrl Pts',(-59.5648797333026,-116.349845053487,
172.967752007192));
#32923=CARTESIAN_POINT('Ctrl Pts',(-59.1815493155087,-116.420213825367,
172.966512880429));
#32924=CARTESIAN_POINT('Ctrl Pts',(-58.4224463099306,-116.565330938028,
173.113689703508));
#32925=CARTESIAN_POINT('Ctrl Pts',(-58.0548941280946,-116.637377196498,
173.26602941121));
#32926=CARTESIAN_POINT('Ctrl Pts',(-57.6663208572241,-116.715768960606,
173.528339014525));
#32927=CARTESIAN_POINT('Ctrl Pts',(-57.6066355545438,-116.727883929458,
173.571993294428));
#32928=CARTESIAN_POINT('Ctrl Pts',(-57.548696527981,-116.73971975462,173.617797875547));
#32929=CARTESIAN_POINT('Ctrl Pts',(-57.601699530204,-117.236902499449,173.617797875548));
#32930=CARTESIAN_POINT('Ctrl Pts',(-57.8924073894534,-117.177516493171,
173.387974343625));
#32931=CARTESIAN_POINT('Ctrl Pts',(-58.2232720552108,-117.111880479211,
173.215293510345));
#32932=CARTESIAN_POINT('Ctrl Pts',(-58.9565866929256,-116.969975687516,
172.994950563429));
#32933=CARTESIAN_POINT('Ctrl Pts',(-59.3548480867578,-116.894755344021,
172.959373278143));
#32934=CARTESIAN_POINT('Ctrl Pts',(-60.1269525894985,-116.752382935572,
173.047692878696));
#32935=CARTESIAN_POINT('Ctrl Pts',(-60.4935717462103,-116.682265410449,
173.164711901945));
#32936=CARTESIAN_POINT('Ctrl Pts',(-61.1752743435507,-116.544895081938,
173.540753986414));
#32937=CARTESIAN_POINT('Ctrl Pts',(-61.4808994828104,-116.479550287966,
173.801249888292));
#32938=CARTESIAN_POINT('Ctrl Pts',(-61.9629267007928,-116.368101375068,
174.41723733329));
#32939=CARTESIAN_POINT('Ctrl Pts',(-62.1389410263743,-116.318304753252,
174.763008528566));
#32940=CARTESIAN_POINT('Ctrl Pts',(-62.3546040300313,-116.230617640446,
175.518516698796));
#32941=CARTESIAN_POINT('Ctrl Pts',(-62.3865568762075,-116.194448040141,
175.922502180891));
#32942=CARTESIAN_POINT('Ctrl Pts',(-62.292463380927,-116.144416712053,176.705349947868));
#32943=CARTESIAN_POINT('Ctrl Pts',(-62.1728619500436,-116.126135946456,
177.077342741514));
#32944=CARTESIAN_POINT('Ctrl Pts',(-61.7921758851629,-116.102023931203,
177.769790584473));
#32945=CARTESIAN_POINT('Ctrl Pts',(-61.5297209982687,-116.097240053436,
178.080638867891));
#32946=CARTESIAN_POINT('Ctrl Pts',(-60.9109174216561,-116.103145538237,
178.571810932972));
#32947=CARTESIAN_POINT('Ctrl Pts',(-60.5638409722789,-116.10911646412,178.752139493388));
#32948=CARTESIAN_POINT('Ctrl Pts',(-59.8057950587711,-116.125233855381,
178.97594447532));
#32949=CARTESIAN_POINT('Ctrl Pts',(-59.4006388551323,-116.135662774514,
179.011585838522));
#32950=CARTESIAN_POINT('Ctrl Pts',(-58.6158692211454,-116.159260503308,
178.923395393299));
#32951=CARTESIAN_POINT('Ctrl Pts',(-58.242694323062,-116.168015133066,178.806439675221));
#32952=CARTESIAN_POINT('Ctrl Pts',(-57.5473008151624,-116.177453709431,
178.430520535517));
#32953=CARTESIAN_POINT('Ctrl Pts',(-57.2347294625985,-116.178012339331,
178.170082723635));
#32954=CARTESIAN_POINT('Ctrl Pts',(-56.7399399987164,-116.170695334496,
177.554191248178));
#32955=CARTESIAN_POINT('Ctrl Pts',(-56.5573256823801,-116.159136475564,
177.208457566208));
#32956=CARTESIAN_POINT('Ctrl Pts',(-56.3278913346571,-116.118901068969,
176.453003161774));
#32957=CARTESIAN_POINT('Ctrl Pts',(-56.2889577101339,-116.090287953991,
176.049031929797));
#32958=CARTESIAN_POINT('Ctrl Pts',(-56.3702401569045,-116.021556856233,
175.266180769898));
#32959=CARTESIAN_POINT('Ctrl Pts',(-56.483227543392,-115.978486538889,174.894171826583));
#32960=CARTESIAN_POINT('Ctrl Pts',(-56.8501334327227,-115.874677683887,
174.20166359593));
#32961=CARTESIAN_POINT('Ctrl Pts',(-57.1056143961393,-115.814677861905,
173.890769819493));
#32962=CARTESIAN_POINT('Ctrl Pts',(-57.423890260819,-115.749201518234,173.632754464228));
#32963=CARTESIAN_POINT('Ctrl Pts',(-57.4332689233803,-115.747278916079,
173.625246265243));
#32964=CARTESIAN_POINT('Ctrl Pts',(-57.4426905235318,-115.745354264963,
173.617797875548));
#32965=CARTESIAN_POINT('Origin',(-54.1598171290174,-67.5719248685924,175.985485069079));
#32966=CARTESIAN_POINT('',(-57.2306785146355,-113.756623285649,173.617797875548));
#32967=CARTESIAN_POINT('',(-57.2836815168596,-114.253806030477,173.617797875548));
#32968=CARTESIAN_POINT('',(-52.327900808713,-67.7672193871761,173.617797875548));
#32969=CARTESIAN_POINT('Ctrl Pts',(-57.230686260479,-113.756621703323,173.617791751974));
#32970=CARTESIAN_POINT('Ctrl Pts',(-56.9391520032908,-113.816176526754,
173.848268605392));
#32971=CARTESIAN_POINT('Ctrl Pts',(-56.6932758300137,-113.872841127714,
174.132419081623));
#32972=CARTESIAN_POINT('Ctrl Pts',(-56.3182567509192,-113.974598128388,
174.779611919365));
#32973=CARTESIAN_POINT('Ctrl Pts',(-56.1928240859027,-114.018738792552,
175.137018307616));
#32974=CARTESIAN_POINT('Ctrl Pts',(-56.0786149232731,-114.089571808378,
175.889782503794));
#32975=CARTESIAN_POINT('Ctrl Pts',(-56.0944605876305,-114.118226185,176.278831751245));
#32976=CARTESIAN_POINT('Ctrl Pts',(-56.2757092205817,-114.163411034205,
177.045248412219));
#32977=CARTESIAN_POINT('Ctrl Pts',(-56.4448647956619,-114.178195885927,
177.413867474309));
#32978=CARTESIAN_POINT('Ctrl Pts',(-56.9081477547668,-114.189327126592,
178.051762152112));
#32979=CARTESIAN_POINT('Ctrl Pts',(-57.1933528069892,-114.189220667881,
178.318322809599));
#32980=CARTESIAN_POINT('Ctrl Pts',(-57.8615774554013,-114.182476464193,
178.737296757641));
#32981=CARTESIAN_POINT('Ctrl Pts',(-58.24106860038,-114.17484128849,178.880760888487));
#32982=CARTESIAN_POINT('Ctrl Pts',(-59.0187163975137,-114.152491052106,
179.00828533427));
#32983=CARTESIAN_POINT('Ctrl Pts',(-59.4087205826764,-114.141164658589,
178.996936233929));
#32984=CARTESIAN_POINT('Ctrl Pts',(-60.1780082358599,-114.123631305916,
178.824279651137));
#32985=CARTESIAN_POINT('Ctrl Pts',(-60.5484738132297,-114.116961555137,
178.659045201321));
#32986=CARTESIAN_POINT('Ctrl Pts',(-61.1906692006231,-114.10908528641,178.202048242943));
#32987=CARTESIAN_POINT('Ctrl Pts',(-61.4599045154499,-114.110583658141,
177.919500596901));
#32988=CARTESIAN_POINT('Ctrl Pts',(-61.8856854300552,-114.129654195603,
177.256122027241));
#32989=CARTESIAN_POINT('Ctrl Pts',(-62.0331959862368,-114.146756256848,
176.878665009532));
#32990=CARTESIAN_POINT('Ctrl Pts',(-62.1693912717361,-114.192858816441,
176.10376818939));
#32991=CARTESIAN_POINT('Ctrl Pts',(-62.162823924056,-114.223707214386,175.714807996739));
#32992=CARTESIAN_POINT('Ctrl Pts',(-62.0010577572282,-114.305396839896,
174.947555617494));
#32993=CARTESIAN_POINT('Ctrl Pts',(-61.8417904801587,-114.355206848899,
174.577949784827));
#32994=CARTESIAN_POINT('Ctrl Pts',(-61.3965692401005,-114.46333021106,173.936829693498));
#32995=CARTESIAN_POINT('Ctrl Pts',(-61.1199773222918,-114.522910269248,
173.668142587039));
#32996=CARTESIAN_POINT('Ctrl Pts',(-60.4691467286856,-114.656718870453,
173.244094882701));
#32997=CARTESIAN_POINT('Ctrl Pts',(-60.0980748242194,-114.729112095771,
173.097649947013));
#32998=CARTESIAN_POINT('Ctrl Pts',(-59.3347779164793,-114.871184521411,
172.963709202852));
#32999=CARTESIAN_POINT('Ctrl Pts',(-58.9512280542984,-114.94210987731,172.971764400139));
#33000=CARTESIAN_POINT('Ctrl Pts',(-58.1946015258564,-115.087177195723,
173.137739855785));
#33001=CARTESIAN_POINT('Ctrl Pts',(-57.8299643801731,-115.15888788711,173.29960349534));
#33002=CARTESIAN_POINT('Ctrl Pts',(-57.4674731119605,-115.232315692349,
173.557862745655));
#33003=CARTESIAN_POINT('Ctrl Pts',(-57.4281921345336,-115.24030577062,173.587357466301));
#33004=CARTESIAN_POINT('Ctrl Pts',(-57.3896875213082,-115.248171520134,
173.617797875547));
#33005=CARTESIAN_POINT('Ctrl Pts',(-57.4426905235318,-115.745354264963,
173.617797875548));
#33006=CARTESIAN_POINT('Ctrl Pts',(-57.7331100939653,-115.686027150527,
173.388202254745));
#33007=CARTESIAN_POINT('Ctrl Pts',(-58.0636102238676,-115.620461726853,
173.215633158892));
#33008=CARTESIAN_POINT('Ctrl Pts',(-58.7964826214188,-115.478635989196,
172.995126174909));
#33009=CARTESIAN_POINT('Ctrl Pts',(-59.1947152712333,-115.403417727966,
172.959399156046));
#33010=CARTESIAN_POINT('Ctrl Pts',(-59.966825838982,-115.261037553985,173.04741694866));
#33011=CARTESIAN_POINT('Ctrl Pts',(-60.3334787221989,-115.19092849755,173.164288045249));
#33012=CARTESIAN_POINT('Ctrl Pts',(-61.0153029832218,-115.053548144051,
173.540042841311));
#33013=CARTESIAN_POINT('Ctrl Pts',(-61.3210194319925,-114.988192560594,
173.800402994964));
#33014=CARTESIAN_POINT('Ctrl Pts',(-61.8032791948,-114.876711202894,174.416166176717));
#33015=CARTESIAN_POINT('Ctrl Pts',(-61.9794313985134,-114.826912850261,
174.761849718203));
#33016=CARTESIAN_POINT('Ctrl Pts',(-62.1954041910925,-114.73919587929,175.51723224345));
#33017=CARTESIAN_POINT('Ctrl Pts',(-62.2275290505995,-114.703006807309,
175.921184408229));
#33018=CARTESIAN_POINT('Ctrl Pts',(-62.1337816503851,-114.652930354216,
176.70404008077));
#33019=CARTESIAN_POINT('Ctrl Pts',(-62.0143517430599,-114.634645241808,
177.076070608353));
#33020=CARTESIAN_POINT('Ctrl Pts',(-61.6339963003143,-114.610501386406,
177.768659522463));
#33021=CARTESIAN_POINT('Ctrl Pts',(-61.3716973480183,-114.605699666669,
178.07961407736));
#33022=CARTESIAN_POINT('Ctrl Pts',(-60.7531506585592,-114.611568918709,
178.571057428201));
#33023=CARTESIAN_POINT('Ctrl Pts',(-60.4061765489483,-114.617543916026,
178.751544696308));
#33024=CARTESIAN_POINT('Ctrl Pts',(-59.6482754714225,-114.633649530162,
178.97570943353));
#33025=CARTESIAN_POINT('Ctrl Pts',(-59.243157451725,-114.644073069761,179.011550909639));
#33026=CARTESIAN_POINT('Ctrl Pts',(-58.458377752376,-114.667662360705,178.92376383316));
#33027=CARTESIAN_POINT('Ctrl Pts',(-58.0851611769012,-114.676437535059,
178.807005809767));
#33028=CARTESIAN_POINT('Ctrl Pts',(-57.389605953392,-114.685897291084,178.431470614418));
#33029=CARTESIAN_POINT('Ctrl Pts',(-57.0769123212988,-114.686467550742,
178.171214243736));
#33030=CARTESIAN_POINT('Ctrl Pts',(-56.5818099708201,-114.679173677331,
177.555622507053));
#33031=CARTESIAN_POINT('Ctrl Pts',(-56.3990150574061,-114.667651375495,
177.210005956547));
#33032=CARTESIAN_POINT('Ctrl Pts',(-56.1691676700437,-114.627464238523,
176.454719494352));
#33033=CARTESIAN_POINT('Ctrl Pts',(-56.130003884674,-114.598874149911,176.050792841041));
#33034=CARTESIAN_POINT('Ctrl Pts',(-56.2108215468567,-114.530181610307,
175.267931179225));
#33035=CARTESIAN_POINT('Ctrl Pts',(-56.3235836736219,-114.487153902853,
174.895871816253));
#33036=CARTESIAN_POINT('Ctrl Pts',(-56.6900487567697,-114.38339659709,174.203175159166));
#33037=CARTESIAN_POINT('Ctrl Pts',(-56.9453209944096,-114.323417404517,
173.892139449795));
#33038=CARTESIAN_POINT('Ctrl Pts',(-57.2639014894801,-114.257854151479,
173.633539083492));
#33039=CARTESIAN_POINT('Ctrl Pts',(-57.2737677291267,-114.255831226019,
173.625635371642));
#33040=CARTESIAN_POINT('Ctrl Pts',(-57.2836815168596,-114.253806030477,
173.617797875548));
#33041=CARTESIAN_POINT('Origin',(-54.1598171290174,-67.5719248685924,175.985485069079));
#33042=CARTESIAN_POINT('',(-57.0716695079633,-112.265075051163,173.617797875548));
#33043=CARTESIAN_POINT('',(-57.1246725101874,-112.762257795992,173.617797875548));
#33044=CARTESIAN_POINT('',(-52.327900808713,-67.7672193871761,173.617797875548));
#33045=CARTESIAN_POINT('Ctrl Pts',(-57.0716695079633,-112.265075051163,
173.617797875548));
#33046=CARTESIAN_POINT('Ctrl Pts',(-57.0627343906797,-112.266900323216,
173.624861668792));
#33047=CARTESIAN_POINT('Ctrl Pts',(-57.0538378855726,-112.268723753602,
173.631979258842));
#33048=CARTESIAN_POINT('Ctrl Pts',(-56.7358636959649,-112.334114147414,
173.88941690138));
#33049=CARTESIAN_POINT('Ctrl Pts',(-56.4801765013653,-112.394134339222,
174.200170259468));
#33050=CARTESIAN_POINT('Ctrl Pts',(-56.112834942677,-112.497994132019,174.892492109895));
#33051=CARTESIAN_POINT('Ctrl Pts',(-55.9996249265372,-112.541106625516,
175.26445122305));
#33052=CARTESIAN_POINT('Ctrl Pts',(-55.9178831697836,-112.609875816504,
176.047291868592));
#33053=CARTESIAN_POINT('Ctrl Pts',(-55.956589322785,-112.638511678251,176.451307024888));
#33054=CARTESIAN_POINT('Ctrl Pts',(-56.1856154501808,-112.678794781052,
177.206927282754));
#33055=CARTESIAN_POINT('Ctrl Pts',(-56.3680513224875,-112.690389816605,
177.552776705815));
#33056=CARTESIAN_POINT('Ctrl Pts',(-56.8625315730818,-112.697729674712,
178.168964237558));
#33057=CARTESIAN_POINT('Ctrl Pts',(-57.1749820220013,-112.697182535531,
178.429581245929));
#33058=CARTESIAN_POINT('Ctrl Pts',(-57.8702156602254,-112.687764886311,
178.805879680385));
#33059=CARTESIAN_POINT('Ctrl Pts',(-58.2433493919726,-112.679030599089,
178.923030700711));
#33060=CARTESIAN_POINT('Ctrl Pts',(-59.0281089814614,-112.655424538366,
179.011619586101));
#33061=CARTESIAN_POINT('Ctrl Pts',(-59.4333028055902,-112.644990307764,
178.976175906596));
#33062=CARTESIAN_POINT('Ctrl Pts',(-60.1914917026374,-112.628861284821,
178.752726318707));
#33063=CARTESIAN_POINT('Ctrl Pts',(-60.5386692377639,-112.622894420582,
178.572554511917));
#33064=CARTESIAN_POINT('Ctrl Pts',(-61.1577264497552,-112.616953152536,
178.081650427006));
#33065=CARTESIAN_POINT('Ctrl Pts',(-61.420335285588,-112.621719408229,177.770907164543));
#33066=CARTESIAN_POINT('Ctrl Pts',(-61.801347838248,-112.645799975499,177.078598712896));
#33067=CARTESIAN_POINT('Ctrl Pts',(-61.9211186531393,-112.664076483555,
176.706643180403));
#33068=CARTESIAN_POINT('Ctrl Pts',(-62.0155538832229,-112.714063249099,
175.923803295569));
#33069=CARTESIAN_POINT('Ctrl Pts',(-61.9837708947597,-112.750213615836,
175.519784988088));
#33070=CARTESIAN_POINT('Ctrl Pts',(-61.7684138027681,-112.837871238476,
174.764152817242));
#33071=CARTESIAN_POINT('Ctrl Pts',(-61.5925356105753,-112.887666181717,
174.418295078142));
#33072=CARTESIAN_POINT('Ctrl Pts',(-61.1107380145101,-112.99908305391,173.802086279413));
#33073=CARTESIAN_POINT('Ctrl Pts',(-60.8052030696972,-113.064417185573,
173.541456399193));
#33074=CARTESIAN_POINT('Ctrl Pts',(-60.1236206355408,-113.201777606753,
173.165130715799));
#33075=CARTESIAN_POINT('Ctrl Pts',(-59.7570347742566,-113.271903518097,
173.047965664686));
#33076=CARTESIAN_POINT('Ctrl Pts',(-58.9978043319857,-113.411895558799,
172.960825081789));
#33077=CARTESIAN_POINT('Ctrl Pts',(-58.6125648708664,-113.484596976178,
172.992533613084));
#33078=CARTESIAN_POINT('Ctrl Pts',(-57.876087918505,-113.626875740639,173.20299707846));
#33079=CARTESIAN_POINT('Ctrl Pts',(-57.5318946593438,-113.695090639415,
173.379666858286));
#33080=CARTESIAN_POINT('Ctrl Pts',(-57.2306785146356,-113.756623285649,
173.617797875548));
#33081=CARTESIAN_POINT('Ctrl Pts',(-57.2836815168596,-114.253806030477,
173.617797875548));
#33082=CARTESIAN_POINT('Ctrl Pts',(-57.5735863268685,-114.194584071664,
173.38860920645));
#33083=CARTESIAN_POINT('Ctrl Pts',(-57.9034357279494,-114.129144665683,
173.216239925632));
#33084=CARTESIAN_POINT('Ctrl Pts',(-58.6355184171523,-113.987460111408,
172.995440774764));
#33085=CARTESIAN_POINT('Ctrl Pts',(-59.0336996098216,-113.912245593771,
172.959446430816));
#33086=CARTESIAN_POINT('Ctrl Pts',(-59.805820864167,-113.769851581135,173.046925348647));
#33087=CARTESIAN_POINT('Ctrl Pts',(-60.1725339536146,-113.699757577027,
173.163532356499));
#33088=CARTESIAN_POINT('Ctrl Pts',(-60.8545752618224,-113.562359354176,
173.538774261281));
#33089=CARTESIAN_POINT('Ctrl Pts',(-61.1604545779857,-113.496984537301,
173.798891998665));
#33090=CARTESIAN_POINT('Ctrl Pts',(-61.6431293382452,-113.38544528829,174.414254732326));
#33091=CARTESIAN_POINT('Ctrl Pts',(-61.8195276279145,-113.335643769574,
174.759781826746));
#33092=CARTESIAN_POINT('Ctrl Pts',(-62.0360532252756,-113.247873532447,
175.514939962153));
#33093=CARTESIAN_POINT('Ctrl Pts',(-62.0684850418152,-113.211649728303,
175.918832483867));
#33094=CARTESIAN_POINT('Ctrl Pts',(-61.9753553055497,-113.161492757481,
176.701702072252));
#33095=CARTESIAN_POINT('Ctrl Pts',(-61.8562314564137,-113.143199800051,
177.073799935792));
#33096=CARTESIAN_POINT('Ctrl Pts',(-61.476465985183,-113.118999143335,177.76664036815));
#33097=CARTESIAN_POINT('Ctrl Pts',(-61.214445377309,-113.114165594034,178.077784358413));
#33098=CARTESIAN_POINT('Ctrl Pts',(-60.5963571844697,-113.119970200329,
178.569711579633));
#33099=CARTESIAN_POINT('Ctrl Pts',(-60.2495656278064,-113.125952358746,
178.750481973186));
#33100=CARTESIAN_POINT('Ctrl Pts',(-59.491923104094,-113.142036962072,178.975288320393));
#33101=CARTESIAN_POINT('Ctrl Pts',(-59.0868734382955,-113.152450900272,
179.01148669837));
#33102=CARTESIAN_POINT('Ctrl Pts',(-58.3020760435979,-113.176025133447,
178.924419112465));
#33103=CARTESIAN_POINT('Ctrl Pts',(-57.9287851232326,-113.184836829471,
178.808013659741));
#33104=CARTESIAN_POINT('Ctrl Pts',(-57.2329417753444,-113.194334347895,
178.433163202329));
#33105=CARTESIAN_POINT('Ctrl Pts',(-56.9200303315871,-113.194925343858,
178.173230539031));
#33106=CARTESIAN_POINT('Ctrl Pts',(-56.42437026228,-113.18767271874,177.558173498531));
#33107=CARTESIAN_POINT('Ctrl Pts',(-56.2412533521598,-113.176215456699,
177.212765772886));
#33108=CARTESIAN_POINT('Ctrl Pts',(-56.0106697986407,-113.136114377111,
176.457778962724));
#33109=CARTESIAN_POINT('Ctrl Pts',(-55.9710957851752,-113.107565356253,
176.053932101379));
#33110=CARTESIAN_POINT('Ctrl Pts',(-56.0510849253777,-113.03894157732,175.271052062676));
#33111=CARTESIAN_POINT('Ctrl Pts',(-56.1634455638887,-112.995989653942,
174.898902832797));
#33112=CARTESIAN_POINT('Ctrl Pts',(-56.5291250084888,-112.892324250224,
174.205870724865));
#33113=CARTESIAN_POINT('Ctrl Pts',(-56.7840250823298,-112.832381873329,
173.894582403637));
#33114=CARTESIAN_POINT('Ctrl Pts',(-57.1031470110203,-112.76666385856,173.634938174122));
#33115=CARTESIAN_POINT('Ctrl Pts',(-57.113881585975,-112.764462173592,173.626328805264));
#33116=CARTESIAN_POINT('Ctrl Pts',(-57.1246725101874,-112.762257795992,
173.617797875548));
#33117=CARTESIAN_POINT('Origin',(-54.1598171290174,-67.5719248685924,175.985485069079));
#33118=CARTESIAN_POINT('',(-56.9126605012911,-110.773526816678,173.617797875548));
#33119=CARTESIAN_POINT('',(-56.9656635035151,-111.270709561506,173.617797875548));
#33120=CARTESIAN_POINT('',(-52.327900808713,-67.7672193871761,173.617797875548));
#33121=CARTESIAN_POINT('Ctrl Pts',(-56.912660501291,-110.773526816678,173.617797875548));
#33122=CARTESIAN_POINT('Ctrl Pts',(-56.9036160521539,-110.775374423119,
173.624948102757));
#33123=CARTESIAN_POINT('Ctrl Pts',(-56.8946111672271,-110.77722014228,173.632153450317));
#33124=CARTESIAN_POINT('Ctrl Pts',(-56.5765691295408,-110.842629856544,
173.889720882783));
#33125=CARTESIAN_POINT('Ctrl Pts',(-56.3209282766764,-110.902645472224,
174.200505809701));
#33126=CARTESIAN_POINT('Ctrl Pts',(-55.9536846276516,-111.006493818502,
174.892869559036));
#33127=CARTESIAN_POINT('Ctrl Pts',(-55.8405246435036,-111.049596828151,
175.264839870551));
#33128=CARTESIAN_POINT('Ctrl Pts',(-55.7588861042098,-111.11835745965,176.047682890698));
#33129=CARTESIAN_POINT('Ctrl Pts',(-55.7976433771382,-111.146988210403,
176.451688187388));
#33130=CARTESIAN_POINT('Ctrl Pts',(-56.0267612449455,-111.187260595197,
177.207271183777));
#33131=CARTESIAN_POINT('Ctrl Pts',(-56.2092372154757,-111.198847496697,
177.553094598093));
#33132=CARTESIAN_POINT('Ctrl Pts',(-56.7037869544156,-111.206182219643,
178.169215612368));
#33133=CARTESIAN_POINT('Ctrl Pts',(-57.0162645787218,-111.205632498413,
178.429792360503));
#33134=CARTESIAN_POINT('Ctrl Pts',(-57.7115341484149,-111.196210146648,
178.806005569765));
#33135=CARTESIAN_POINT('Ctrl Pts',(-58.0846771294381,-111.187471284538,
178.923112706732));
#33136=CARTESIAN_POINT('Ctrl Pts',(-58.8694389846079,-111.163867095625,
179.011612068858));
#33137=CARTESIAN_POINT('Ctrl Pts',(-59.2746243643901,-111.153434058225,
178.976123971552));
#33138=CARTESIAN_POINT('Ctrl Pts',(-60.03278114244,-111.137307648605,178.752594529208));
#33139=CARTESIAN_POINT('Ctrl Pts',(-60.3799359654912,-111.131339868321,
178.572387503619));
#33140=CARTESIAN_POINT('Ctrl Pts',(-60.9989361993644,-111.12540663962,178.081423206973));
#33141=CARTESIAN_POINT('Ctrl Pts',(-61.2615104522396,-111.130176854553,
177.770656343799));
#33142=CARTESIAN_POINT('Ctrl Pts',(-61.642449656401,-111.154264487422,177.078316569314));
#33143=CARTESIAN_POINT('Ctrl Pts',(-61.7621824171466,-111.172541948953,
176.706352665837));
#33144=CARTESIAN_POINT('Ctrl Pts',(-61.8565408761524,-111.222538726042,
175.92351100368));
#33145=CARTESIAN_POINT('Ctrl Pts',(-61.8247197279864,-111.258693414243,
175.519500064209));
#33146=CARTESIAN_POINT('Ctrl Pts',(-61.6092939104062,-111.346357662586,
174.763895744913));
#33147=CARTESIAN_POINT('Ctrl Pts',(-61.4333851363702,-111.396152980288,
174.418057447483));
#33148=CARTESIAN_POINT('Ctrl Pts',(-60.9515359549162,-111.507577050861,
173.80189836882));
#33149=CARTESIAN_POINT('Ctrl Pts',(-60.6459807447754,-111.57291357858,173.541298581809));
#33150=CARTESIAN_POINT('Ctrl Pts',(-59.964371313043,-111.7102762262,173.165036603142));
#33151=CARTESIAN_POINT('Ctrl Pts',(-59.59777797244,-111.780400251476,173.0479043543));
#33152=CARTESIAN_POINT('Ctrl Pts',(-58.8256781502785,-111.922766709292,
172.959353762966));
#33153=CARTESIAN_POINT('Ctrl Pts',(-58.4273947936942,-111.997988639473,
172.994816442521));
#33154=CARTESIAN_POINT('Ctrl Pts',(-57.6937417099188,-112.13995392666,173.215033647115));
#33155=CARTESIAN_POINT('Ctrl Pts',(-57.3625980045214,-112.20564397294,173.387799915435));
#33156=CARTESIAN_POINT('Ctrl Pts',(-57.0716695079633,-112.265075051163,
173.617797875548));
#33157=CARTESIAN_POINT('Ctrl Pts',(-57.1246725101874,-112.762257795992,
173.617797875548));
#33158=CARTESIAN_POINT('Ctrl Pts',(-57.413660289602,-112.703223168834,173.389334178972));
#33159=CARTESIAN_POINT('Ctrl Pts',(-57.742350995899,-112.638008176024,173.217321815072));
#33160=CARTESIAN_POINT('Ctrl Pts',(-58.4730266643655,-112.496575220331,
172.996004506073));
#33161=CARTESIAN_POINT('Ctrl Pts',(-58.8711157663971,-112.421367452974,
172.959534041656));
#33162=CARTESIAN_POINT('Ctrl Pts',(-59.6432556046902,-112.278948873754,
173.046053048715));
#33163=CARTESIAN_POINT('Ctrl Pts',(-60.0100759029152,-112.208881465366,
173.162189732229));
#33164=CARTESIAN_POINT('Ctrl Pts',(-60.6925032651767,-112.071451507064,
173.536518198727));
#33165=CARTESIAN_POINT('Ctrl Pts',(-60.9986721778529,-112.006042527929,
173.796203989923));
#33166=CARTESIAN_POINT('Ctrl Pts',(-61.4820855205812,-111.894400277994,
174.410853305157));
#33167=CARTESIAN_POINT('Ctrl Pts',(-61.6589218717488,-111.844592879084,
174.756101899925));
#33168=CARTESIAN_POINT('Ctrl Pts',(-61.8764311790495,-111.756727901188,
175.510860159495));
#33169=CARTESIAN_POINT('Ctrl Pts',(-61.9094092428966,-111.720442336648,
175.914645945218));
#33170=CARTESIAN_POINT('Ctrl Pts',(-61.8173788624534,-111.670142104047,
176.697539689913));
#33171=CARTESIAN_POINT('Ctrl Pts',(-61.6987995837909,-111.651834906258,
177.069757381944));
#33172=CARTESIAN_POINT('Ctrl Pts',(-61.3200839310779,-111.627533223033,
177.763044700792));
#33173=CARTESIAN_POINT('Ctrl Pts',(-61.0585589056476,-111.622643060867,
178.074525150415));
#33174=CARTESIAN_POINT('Ctrl Pts',(-60.4412868963765,-111.628332662555,
178.567312693833));
#33175=CARTESIAN_POINT('Ctrl Pts',(-60.0948199758521,-111.634327233912,
178.748586648949));
#33176=CARTESIAN_POINT('Ctrl Pts',(-59.3376378629081,-111.650374464427,
178.974533602147));
#33177=CARTESIAN_POINT('Ctrl Pts',(-58.932710516522,-111.660771311206,179.011366477713));
#33178=CARTESIAN_POINT('Ctrl Pts',(-58.147882474537,-111.684318746739,178.92557825714));
#33179=CARTESIAN_POINT('Ctrl Pts',(-57.7744593417187,-111.693194992019,
178.809799546446));
#33180=CARTESIAN_POINT('Ctrl Pts',(-57.0781047024549,-111.702759607706,
178.436166325688));
#33181=CARTESIAN_POINT('Ctrl Pts',(-56.7648069018154,-111.703387451443,
178.176809484026));
#33182=CARTESIAN_POINT('Ctrl Pts',(-56.26815631875,-111.696208136346,177.562703376644));
#33183=CARTESIAN_POINT('Ctrl Pts',(-56.0844672742459,-111.684865996432,
177.217666648423));
#33184=CARTESIAN_POINT('Ctrl Pts',(-55.8525765184924,-111.644917809419,
176.463212957767));
#33185=CARTESIAN_POINT('Ctrl Pts',(-55.8122740399269,-111.616441799022,
176.059508852572));
#33186=CARTESIAN_POINT('Ctrl Pts',(-55.8907915716628,-111.547940237584,
175.276597259374));
#33187=CARTESIAN_POINT('Ctrl Pts',(-56.0024392749427,-111.505122377378,
174.904288442366));
#33188=CARTESIAN_POINT('Ctrl Pts',(-56.3667237210741,-111.401620242415,
174.210661889557));
#33189=CARTESIAN_POINT('Ctrl Pts',(-56.620962479084,-111.341743388782,173.898926136395));
#33190=CARTESIAN_POINT('Ctrl Pts',(-56.9410410403329,-111.275751002892,
173.63742458343));
#33191=CARTESIAN_POINT('Ctrl Pts',(-56.9533153611321,-111.273232048731,
173.627559887839));
#33192=CARTESIAN_POINT('Ctrl Pts',(-56.9656635035151,-111.270709561506,
173.617797875548));
#33193=CARTESIAN_POINT('Origin',(-54.1598171290174,-67.5719248685924,175.985485069079));
#33194=CARTESIAN_POINT('',(-56.7536514946188,-109.281978582192,173.617797875548));
#33195=CARTESIAN_POINT('',(-56.8066544968429,-109.779161327021,173.617797875548));
#33196=CARTESIAN_POINT('',(-52.327900808713,-67.7672193871761,173.617797875548));
#33197=CARTESIAN_POINT('Ctrl Pts',(-56.7536514946188,-109.281978582192,
173.617797875548));
#33198=CARTESIAN_POINT('Ctrl Pts',(-56.7444114652081,-109.283866141909,
173.625102721725));
#33199=CARTESIAN_POINT('Ctrl Pts',(-56.7352127320762,-109.285751731342,
173.632465095959));
#33200=CARTESIAN_POINT('Ctrl Pts',(-56.4170493951529,-109.351196001371,
173.890264770392));
#33201=CARTESIAN_POINT('Ctrl Pts',(-56.1614914509907,-109.411203428396,
174.201106153446));
#33202=CARTESIAN_POINT('Ctrl Pts',(-55.7944229529086,-109.515031296611,
174.893544837145));
#33203=CARTESIAN_POINT('Ctrl Pts',(-55.6813524717919,-109.558117348435,
175.265535181684));
#33204=CARTESIAN_POINT('Ctrl Pts',(-55.5998985858842,-109.626862665881,
176.048382432889));
#33205=CARTESIAN_POINT('Ctrl Pts',(-55.6387473083432,-109.655484272148,
176.452370074809));
#33206=CARTESIAN_POINT('Ctrl Pts',(-55.868029291656,-109.695737482092,177.207886397512));
#33207=CARTESIAN_POINT('Ctrl Pts',(-56.0505770001051,-109.707309838255,
177.553663281513));
#33208=CARTESIAN_POINT('Ctrl Pts',(-56.5452510503984,-109.714635373818,
178.169665278726));
#33209=CARTESIAN_POINT('Ctrl Pts',(-56.8577772827169,-109.714081033111,
178.430169988861));
#33210=CARTESIAN_POINT('Ctrl Pts',(-57.5531111255177,-109.704650268233,
178.806230716513));
#33211=CARTESIAN_POINT('Ctrl Pts',(-57.9262706557755,-109.695903226762,
178.923259339289));
#33212=CARTESIAN_POINT('Ctrl Pts',(-58.7110365519678,-109.672302387285,
179.011598524387));
#33213=CARTESIAN_POINT('Ctrl Pts',(-59.1162068108045,-109.661871485081,
178.976030955739));
#33214=CARTESIAN_POINT('Ctrl Pts',(-59.874306110465,-109.645749751471,178.752358640327));
#33215=CARTESIAN_POINT('Ctrl Pts',(-60.2214202961156,-109.639780337178,
178.572088598617));
#33216=CARTESIAN_POINT('Ctrl Pts',(-60.8403185693232,-109.633861493506,
178.081016570927));
#33217=CARTESIAN_POINT('Ctrl Pts',(-61.1028309355344,-109.638638792637,
177.77020748683));
#33218=CARTESIAN_POINT('Ctrl Pts',(-61.4836388910742,-109.662739067824,
177.077811674308));
#33219=CARTESIAN_POINT('Ctrl Pts',(-61.6033035590136,-109.681018239856,
176.705832791815));
#33220=CARTESIAN_POINT('Ctrl Pts',(-61.6975246410322,-109.731032931215,
175.922987958783));
#33221=CARTESIAN_POINT('Ctrl Pts',(-61.6656352099253,-109.767195351502,
175.518990212935));
#33222=CARTESIAN_POINT('Ctrl Pts',(-61.4500864154564,-109.854871455099,
174.763435739915));
#33223=CARTESIAN_POINT('Ctrl Pts',(-61.2741229161873,-109.904667446682,
174.417632232832));
#33224=CARTESIAN_POINT('Ctrl Pts',(-60.792181426792,-110.016104397719,173.801562135608));
#33225=CARTESIAN_POINT('Ctrl Pts',(-60.486589957542,-110.081445211935,173.54101620596));
#33226=CARTESIAN_POINT('Ctrl Pts',(-59.8049322193929,-110.218811842546,
173.164868231645));
#33227=CARTESIAN_POINT('Ctrl Pts',(-59.4383254942508,-110.288932495851,
173.047794684789));
#33228=CARTESIAN_POINT('Ctrl Pts',(-58.6662232412889,-110.431302039515,
172.959363849016));
#33229=CARTESIAN_POINT('Ctrl Pts',(-58.2679512671702,-110.506523147845,
172.994885945774));
#33230=CARTESIAN_POINT('Ctrl Pts',(-57.5344736456333,-110.648457072547,
173.215168361749));
#33231=CARTESIAN_POINT('Ctrl Pts',(-57.2034746106801,-110.714119105546,
173.387890345956));
#33232=CARTESIAN_POINT('Ctrl Pts',(-56.912660501291,-110.773526816678,173.617797875548));
#33233=CARTESIAN_POINT('Ctrl Pts',(-56.9656635035151,-111.270709561506,
173.617797875548));
#33234=CARTESIAN_POINT('Ctrl Pts',(-57.2530242924217,-111.212007297116,
173.390620421133));
#33235=CARTESIAN_POINT('Ctrl Pts',(-57.5796610124049,-111.147190193251,
173.219244299193));
#33236=CARTESIAN_POINT('Ctrl Pts',(-58.3078397992584,-111.006203887084,
172.997015018109));
#33237=CARTESIAN_POINT('Ctrl Pts',(-58.7057641868601,-110.931008351939,
172.95970017545));
#33238=CARTESIAN_POINT('Ctrl Pts',(-59.4779355658374,-110.78854645965,173.044516359449));
#33239=CARTESIAN_POINT('Ctrl Pts',(-59.8449459276702,-110.7185255451,173.159819039321));
#33240=CARTESIAN_POINT('Ctrl Pts',(-60.5280563098773,-110.581039590946,
173.532527712615));
#33241=CARTESIAN_POINT('Ctrl Pts',(-60.8347373006261,-110.515570320914,
173.791446869636));
#33242=CARTESIAN_POINT('Ctrl Pts',(-61.3194587580523,-110.403745738482,
174.404830339381));
#33243=CARTESIAN_POINT('Ctrl Pts',(-61.4970712714973,-110.353927151605,
174.749585468772));
#33244=CARTESIAN_POINT('Ctrl Pts',(-61.7163224303376,-110.265894560392,
175.503633857603));
#33245=CARTESIAN_POINT('Ctrl Pts',(-61.7502677930237,-110.229499779283,
175.907228754417));
#33246=CARTESIAN_POINT('Ctrl Pts',(-61.6601847599457,-110.178945932191,
176.690163364291));
#33247=CARTESIAN_POINT('Ctrl Pts',(-61.5425695762014,-110.160612637411,
177.062593254234));
#33248=CARTESIAN_POINT('Ctrl Pts',(-61.1657127416764,-110.13613222623,177.756669717359));
#33249=CARTESIAN_POINT('Ctrl Pts',(-60.9050660910469,-110.131141906601,
178.068743926659));
#33250=CARTESIAN_POINT('Ctrl Pts',(-60.2892402183872,-110.136627969695,
178.563052580947));
#33251=CARTESIAN_POINT('Ctrl Pts',(-59.9433474574605,-110.142643484303,
178.745217390532));
#33252=CARTESIAN_POINT('Ctrl Pts',(-59.1869815832755,-110.158624588141,
178.97318046481));
#33253=CARTESIAN_POINT('Ctrl Pts',(-58.782272969959,-110.1689911531,179.011134939961));
#33254=CARTESIAN_POINT('Ctrl Pts',(-57.9973932965281,-110.192491130305,
178.927609078305));
#33255=CARTESIAN_POINT('Ctrl Pts',(-57.6237363130985,-110.20148029302,178.81293809646));
#33256=CARTESIAN_POINT('Ctrl Pts',(-56.9264807797385,-110.211163403075,
178.441456326529));
#33257=CARTESIAN_POINT('Ctrl Pts',(-56.6125027299724,-110.211856329087,
178.183118417219));
#33258=CARTESIAN_POINT('Ctrl Pts',(-56.1141043193472,-110.204806539356,
177.570694390137));
#33259=CARTESIAN_POINT('Ctrl Pts',(-55.9294048654883,-110.19366632275,177.226312697729));
#33260=CARTESIAN_POINT('Ctrl Pts',(-55.6952081929263,-110.153988093797,
176.472802651947));
#33261=CARTESIAN_POINT('Ctrl Pts',(-55.65362061935,-110.125641145017,176.069353712619));
#33262=CARTESIAN_POINT('Ctrl Pts',(-55.7295409368849,-110.057355550999,
175.286389822705));
#33263=CARTESIAN_POINT('Ctrl Pts',(-55.8399309532616,-110.014772600424,
174.913799450684));
#33264=CARTESIAN_POINT('Ctrl Pts',(-56.2017547688197,-109.911558719943,
174.21912806331));
#33265=CARTESIAN_POINT('Ctrl Pts',(-56.4548255081651,-109.851797916736,
173.9066065584));
#33266=CARTESIAN_POINT('Ctrl Pts',(-56.7765766114406,-109.785322912825,
173.641817041259));
#33267=CARTESIAN_POINT('Ctrl Pts',(-56.7915603540426,-109.782244769145,
173.62973078035));
#33268=CARTESIAN_POINT('Ctrl Pts',(-56.8066544968429,-109.779161327021,
173.617797875548));
#33269=CARTESIAN_POINT('Origin',(-54.1598171290174,-67.5719248685924,175.985485069079));
#33270=CARTESIAN_POINT('',(-56.5946424879466,-107.790430347706,173.617797875548));
#33271=CARTESIAN_POINT('',(-56.6476454901706,-108.287613092535,173.617797875548));
#33272=CARTESIAN_POINT('',(-52.327900808713,-67.7672193871761,173.617797875548));
#33273=CARTESIAN_POINT('Ctrl Pts',(-56.5946424879466,-107.790430347706,
173.617797875548));
#33274=CARTESIAN_POINT('Ctrl Pts',(-56.5850528888066,-107.792389317774,
173.625379079406));
#33275=CARTESIAN_POINT('Ctrl Pts',(-56.5755077744589,-107.794346164695,
173.63302224271));
#33276=CARTESIAN_POINT('Ctrl Pts',(-56.2571278640508,-107.859852178723,
173.89123722131));
#33277=CARTESIAN_POINT('Ctrl Pts',(-56.0017181366438,-107.919844961586,
174.20217945882));
#33278=CARTESIAN_POINT('Ctrl Pts',(-55.6349627050625,-108.023636222819,
174.894752021053));
#33279=CARTESIAN_POINT('Ctrl Pts',(-55.5220522045499,-108.066691989198,
175.266778173584));
#33280=CARTESIAN_POINT('Ctrl Pts',(-55.4409283932585,-108.135409927915,
176.049632933467));
#33281=CARTESIAN_POINT('Ctrl Pts',(-55.4799405763947,-108.164015184729,
176.453588965104));
#33282=CARTESIAN_POINT('Ctrl Pts',(-55.7095159037854,-108.20423411699,177.208986061887));
#33283=CARTESIAN_POINT('Ctrl Pts',(-55.8921918566918,-108.215780492895,
177.554679766979));
#33284=CARTESIAN_POINT('Ctrl Pts',(-56.3870881131878,-108.223089603402,
178.170468956079));
#33285=CARTESIAN_POINT('Ctrl Pts',(-56.6997012083162,-108.222527004388,
178.430844852629));
#33286=CARTESIAN_POINT('Ctrl Pts',(-57.3951499180593,-108.213081199548,
178.806632962964));
#33287=CARTESIAN_POINT('Ctrl Pts',(-57.7683390387316,-108.204319553149,
178.92352121324));
#33288=CARTESIAN_POINT('Ctrl Pts',(-58.5531121193096,-108.180724703527,
179.011574005107));
#33289=CARTESIAN_POINT('Ctrl Pts',(-58.9582553034152,-108.170297619943,
178.975864349681));
#33290=CARTESIAN_POINT('Ctrl Pts',(-59.716251799764,-108.154184247559,178.75193659395));
#33291=CARTESIAN_POINT('Ctrl Pts',(-60.0632933251485,-108.148211927685,
178.571553874758));
#33292=CARTESIAN_POINT('Ctrl Pts',(-60.6820092495562,-108.142318806873,
178.080289229826));
#33293=CARTESIAN_POINT('Ctrl Pts',(-60.944410931511,-108.147108773163,177.769404674777));
#33294=CARTESIAN_POINT('Ctrl Pts',(-61.3249841793317,-108.171231653807,
177.076908684947));
#33295=CARTESIAN_POINT('Ctrl Pts',(-61.4445270812119,-108.189513898651,
176.704903015587));
#33296=CARTESIAN_POINT('Ctrl Pts',(-61.5385024833708,-108.239560624799,
175.92205254238));
#33297=CARTESIAN_POINT('Ctrl Pts',(-61.506490942202,-108.275736869974,175.518078420413));
#33298=CARTESIAN_POINT('Ctrl Pts',(-61.2907222307222,-108.363434171794,
174.762613115205));
#33299=CARTESIAN_POINT('Ctrl Pts',(-61.1146608598201,-108.413231380705,
174.416871828143));
#33300=CARTESIAN_POINT('Ctrl Pts',(-60.6325542930779,-108.524691364817,
173.800960895677));
#33301=CARTESIAN_POINT('Ctrl Pts',(-60.3268979935203,-108.590039841336,
173.540511306411));
#33302=CARTESIAN_POINT('Ctrl Pts',(-59.6451538789054,-108.727413591522,
173.16456724127));
#33303=CARTESIAN_POINT('Ctrl Pts',(-59.2785232148838,-108.797528224217,
173.047598688914));
#33304=CARTESIAN_POINT('Ctrl Pts',(-58.5064166364563,-108.939903283303,
172.959382058774));
#33305=CARTESIAN_POINT('Ctrl Pts',(-58.108165043366,-109.015122917537,172.995010430971));
#33306=CARTESIAN_POINT('Ctrl Pts',(-57.3750012843017,-109.15700073919,173.215409376339));
#33307=CARTESIAN_POINT('Ctrl Pts',(-57.0442609969736,-109.22261266833,173.388052101168));
#33308=CARTESIAN_POINT('Ctrl Pts',(-56.7536514946188,-109.281978582192,
173.617797875548));
#33309=CARTESIAN_POINT('Ctrl Pts',(-56.8066544968429,-109.779161327021,
173.617797875548));
#33310=CARTESIAN_POINT('Ctrl Pts',(-57.0911495393457,-109.721044479324,
173.39288598066));
#33311=CARTESIAN_POINT('Ctrl Pts',(-57.4141738946121,-109.656927388934,
173.222639859508));
#33312=CARTESIAN_POINT('Ctrl Pts',(-58.1379530574512,-109.516728615689,
172.998827087965));
#33313=CARTESIAN_POINT('Ctrl Pts',(-58.5355831915522,-109.44155542204,172.96002607628));
#33314=CARTESIAN_POINT('Ctrl Pts',(-59.3078056750551,-109.299018087244,
173.041843688515));
#33315=CARTESIAN_POINT('Ctrl Pts',(-59.6751503694515,-109.229076912984,
173.155678725912));
#33316=CARTESIAN_POINT('Ctrl Pts',(-60.3594578804737,-109.091493285794,
173.525536872694));
#33317=CARTESIAN_POINT('Ctrl Pts',(-60.6670354869716,-109.025918812521,
173.783104843788));
#33318=CARTESIAN_POINT('Ctrl Pts',(-61.1540539887737,-108.913774347019,
174.394258350367));
#33319=CARTESIAN_POINT('Ctrl Pts',(-61.3330304093029,-108.863933709409,
174.73814629728));
#33320=CARTESIAN_POINT('Ctrl Pts',(-61.5553389931981,-108.775607355957,
175.490943063268));
#33321=CARTESIAN_POINT('Ctrl Pts',(-61.5909823940636,-108.739021313527,
175.894197042022));
#33322=CARTESIAN_POINT('Ctrl Pts',(-61.5043197220977,-108.688022485585,
176.677197469897));
#33323=CARTESIAN_POINT('Ctrl Pts',(-61.38839627213,-108.669640650694,177.049999895134));
#33324=CARTESIAN_POINT('Ctrl Pts',(-61.014801889141,-108.644847014232,177.745454875642));
#33325=CARTESIAN_POINT('Ctrl Pts',(-60.755699625328,-108.639681161078,178.0585650829));
#33326=CARTESIAN_POINT('Ctrl Pts',(-60.1424149719043,-108.644810265419,
178.555536733806));
#33327=CARTESIAN_POINT('Ctrl Pts',(-59.7975279520725,-108.650859342097,
178.739262801913));
#33328=CARTESIAN_POINT('Ctrl Pts',(-59.0425978361606,-108.666724527345,
178.970753810606));
#33329=CARTESIAN_POINT('Ctrl Pts',(-58.6382797420984,-108.677037884769,
179.010671108535));
#33330=CARTESIAN_POINT('Ctrl Pts',(-57.8533175485435,-108.700454535644,
178.931107044723));
#33331=CARTESIAN_POINT('Ctrl Pts',(-57.4792508646161,-108.709637658776,
178.818374185432));
#33332=CARTESIAN_POINT('Ctrl Pts',(-56.7804276486958,-108.719527793124,
178.450656786394));
#33333=CARTESIAN_POINT('Ctrl Pts',(-56.4652674748089,-108.720334450473,
178.19410526483));
#33334=CARTESIAN_POINT('Ctrl Pts',(-55.9638197847289,-108.713511139287,
177.584628405587));
#33335=CARTESIAN_POINT('Ctrl Pts',(-55.7773549261986,-108.702719464541,
177.241390696198));
#33336=CARTESIAN_POINT('Ctrl Pts',(-55.5391375163741,-108.663512727931,
176.489535882969));
#33337=CARTESIAN_POINT('Ctrl Pts',(-55.495308995132,-108.635391641772,176.08654209288));
#33338=CARTESIAN_POINT('Ctrl Pts',(-55.5666967264702,-108.567483768668,
175.303497323436));
#33339=CARTESIAN_POINT('Ctrl Pts',(-55.6748935190697,-108.525305592323,
174.930415854593));
#33340=CARTESIAN_POINT('Ctrl Pts',(-56.0324273128658,-108.422595081495,
174.233934107104));
#33341=CARTESIAN_POINT('Ctrl Pts',(-56.283457047243,-108.36303804919,173.920053289181));
#33342=CARTESIAN_POINT('Ctrl Pts',(-56.6080785837145,-108.295725776454,
173.649495489686));
#33343=CARTESIAN_POINT('Ctrl Pts',(-56.6277661435339,-108.29167405947,173.633513796226));
#33344=CARTESIAN_POINT('Ctrl Pts',(-56.6476454901706,-108.287613092535,
173.617797875548));
#33345=CARTESIAN_POINT('Origin',(-54.1598171290174,-67.5719248685924,175.985485069079));
#33346=CARTESIAN_POINT('',(-56.4356334812744,-106.298882113221,173.617797875548));
#33347=CARTESIAN_POINT('',(-56.4886364834984,-106.796064858049,173.617797875548));
#33348=CARTESIAN_POINT('',(-52.327900808713,-67.7672193871761,173.617797875548));
#33349=CARTESIAN_POINT('Ctrl Pts',(-56.4356334812744,-106.298882113221,
173.617797875548));
#33350=CARTESIAN_POINT('Ctrl Pts',(-56.4254200290466,-106.300968524437,
173.625872275979));
#33351=CARTESIAN_POINT('Ctrl Pts',(-56.4152570474672,-106.30305252532,173.634016952005));
#33352=CARTESIAN_POINT('Ctrl Pts',(-56.0964913676981,-106.368668668546,
173.892973755425));
#33353=CARTESIAN_POINT('Ctrl Pts',(-55.8413462486002,-106.428635290865,
174.204095814467));
#33354=CARTESIAN_POINT('Ctrl Pts',(-55.4751495605777,-106.53236120433,174.896907124857));
#33355=CARTESIAN_POINT('Ctrl Pts',(-55.3625245910191,-106.575362999072,
175.268997188014));
#33356=CARTESIAN_POINT('Ctrl Pts',(-55.2819899528662,-106.644032053867,
176.051865176928));
#33357=CARTESIAN_POINT('Ctrl Pts',(-55.3212938805754,-106.672608116728,
176.455764620233));
#33358=CARTESIAN_POINT('Ctrl Pts',(-55.5513927597733,-106.712765858169,
177.210948761198));
#33359=CARTESIAN_POINT('Ctrl Pts',(-55.7342976581586,-106.724265924084,
177.556493980804));
#33360=CARTESIAN_POINT('Ctrl Pts',(-56.229590530456,-106.731545709104,178.171903119991));
#33361=CARTESIAN_POINT('Ctrl Pts',(-56.5423585907699,-106.730968366645,
178.432048950983));
#33362=CARTESIAN_POINT('Ctrl Pts',(-57.2380122593381,-106.721495712049,
178.807350285382));
#33363=CARTESIAN_POINT('Ctrl Pts',(-57.6112542237444,-106.712708047288,
178.923987893515));
#33364=CARTESIAN_POINT('Ctrl Pts',(-58.3960400034764,-106.689123897715,
179.011529255791));
#33365=CARTESIAN_POINT('Ctrl Pts',(-58.80113471485,-106.678703636253,178.975565887805));
#33366=CARTESIAN_POINT('Ctrl Pts',(-59.5589475234609,-106.662605196984,
178.751182020938));
#33367=CARTESIAN_POINT('Ctrl Pts',(-59.9058592904742,-106.656627739491,
178.570598067742));
#33368=CARTESIAN_POINT('Ctrl Pts',(-60.5242494393363,-106.650780562228,
178.078989466319));
#33369=CARTESIAN_POINT('Ctrl Pts',(-60.7864533631301,-106.655593151436,
177.767970199565));
#33370=CARTESIAN_POINT('Ctrl Pts',(-61.1666073584006,-106.679756403993,
177.075295373119));
#33371=CARTESIAN_POINT('Ctrl Pts',(-61.2859327593645,-106.698044182358,
176.703241853839));
#33372=CARTESIAN_POINT('Ctrl Pts',(-61.379469268274,-106.748148129126,175.920381402153));
#33373=CARTESIAN_POINT('Ctrl Pts',(-61.3472395990604,-106.784349062473,
175.516449575185));
#33374=CARTESIAN_POINT('Ctrl Pts',(-61.1310780509395,-106.872084223286,
174.761143641781));
#33375=CARTESIAN_POINT('Ctrl Pts',(-60.9548418280128,-106.921883645804,
174.415513514529));
#33376=CARTESIAN_POINT('Ctrl Pts',(-60.4724403685815,-107.033384771253,
173.79988702853));
#33377=CARTESIAN_POINT('Ctrl Pts',(-60.1666682984753,-107.098746924849,
173.539609622196));
#33378=CARTESIAN_POINT('Ctrl Pts',(-59.4847699184305,-107.236133382704,
173.164029918927));
#33379=CARTESIAN_POINT('Ctrl Pts',(-59.1180964810416,-107.306237290906,
173.04724897829));
#33380=CARTESIAN_POINT('Ctrl Pts',(-58.3459822447139,-107.448622192787,
172.959415139878));
#33381=CARTESIAN_POINT('Ctrl Pts',(-57.9477671412253,-107.523839179786,
172.99523341803));
#33382=CARTESIAN_POINT('Ctrl Pts',(-57.2151643108154,-107.665616726848,
173.215840241925));
#33383=CARTESIAN_POINT('Ctrl Pts',(-56.8848863394666,-107.731139129254,
173.388341172012));
#33384=CARTESIAN_POINT('Ctrl Pts',(-56.5946424879466,-107.790430347706,
173.617797875548));
#33385=CARTESIAN_POINT('Ctrl Pts',(-56.6476454901706,-108.287613092535,
173.617797875548));
#33386=CARTESIAN_POINT('Ctrl Pts',(-56.9271567322471,-108.230514339101,
173.396826000098));
#33387=CARTESIAN_POINT('Ctrl Pts',(-57.2439154945503,-108.16761214956,173.228573427838));
#33388=CARTESIAN_POINT('Ctrl Pts',(-57.9600385015072,-108.028785391668,
173.002076223596));
#33389=CARTESIAN_POINT('Ctrl Pts',(-58.3571443608821,-107.953653470066,
172.96069400138));
#33390=CARTESIAN_POINT('Ctrl Pts',(-59.1294421972055,-107.810987508801,
173.037298982509));
#33391=CARTESIAN_POINT('Ctrl Pts',(-59.4973670458519,-107.741178468716,
173.148585634684));
#33392=CARTESIAN_POINT('Ctrl Pts',(-60.183738614452,-107.603427863765,173.513494069579));
#33393=CARTESIAN_POINT('Ctrl Pts',(-60.4928593242721,-107.537673434034,
173.768709668626));
#33394=CARTESIAN_POINT('Ctrl Pts',(-60.9838513802244,-107.42497650289,174.375984000262));
#33395=CARTESIAN_POINT('Ctrl Pts',(-61.1651902167986,-107.375090420716,
174.718369817544));
#33396=CARTESIAN_POINT('Ctrl Pts',(-61.3927839950836,-107.286257596546,
175.468986101822));
#33397=CARTESIAN_POINT('Ctrl Pts',(-61.4313630690126,-107.249342283814,
175.871633114773));
#33398=CARTESIAN_POINT('Ctrl Pts',(-61.3506197086899,-107.197574793199,
176.654729483581));
#33399=CARTESIAN_POINT('Ctrl Pts',(-61.2376192257481,-107.179100797428,
177.028176172647));
#33400=CARTESIAN_POINT('Ctrl Pts',(-60.8696636141788,-107.15376717538,177.725994234135));
#33401=CARTESIAN_POINT('Ctrl Pts',(-60.6132387257904,-107.148298710394,
178.040876606816));
#33402=CARTESIAN_POINT('Ctrl Pts',(-60.0043555131084,-107.152811678755,
178.542430749144));
#33403=CARTESIAN_POINT('Ctrl Pts',(-59.6612009197382,-107.158909180165,
178.728848560318));
#33404=CARTESIAN_POINT('Ctrl Pts',(-58.9087617030258,-107.174574437879,
178.966405587943));
#33405=CARTESIAN_POINT('Ctrl Pts',(-58.5051382541458,-107.18479566087,179.009698156442));
#33406=CARTESIAN_POINT('Ctrl Pts',(-57.7200575738111,-107.208068199376,
178.936955000543));
#33407=CARTESIAN_POINT('Ctrl Pts',(-57.3452848574596,-107.217573992269,
178.827554031224));
#33408=CARTESIAN_POINT('Ctrl Pts',(-56.6437920571633,-107.227819128835,
178.466308091154));
#33409=CARTESIAN_POINT('Ctrl Pts',(-56.3266238180267,-107.228820871757,
178.212838044334));
#33410=CARTESIAN_POINT('Ctrl Pts',(-55.8199603392634,-107.222386462151,
177.60843981115));
#33411=CARTESIAN_POINT('Ctrl Pts',(-55.6304676592532,-107.212179880791,
177.267162528894));
#33412=CARTESIAN_POINT('Ctrl Pts',(-55.3853790529965,-107.173781187623,
176.518165416363));
#33413=CARTESIAN_POINT('Ctrl Pts',(-55.3377206422314,-107.146048492687,
176.115979638056));
#33414=CARTESIAN_POINT('Ctrl Pts',(-55.401350875959,-107.078789512188,175.332827144021));
#33415=CARTESIAN_POINT('Ctrl Pts',(-55.5057985904533,-107.037288828511,
174.958905787373));
#33416=CARTESIAN_POINT('Ctrl Pts',(-55.856002399949,-106.935440746386,174.259363819959));
#33417=CARTESIAN_POINT('Ctrl Pts',(-56.1035315863118,-106.876236083587,
173.943191795572));
#33418=CARTESIAN_POINT('Ctrl Pts',(-56.4329223458913,-106.807505761024,
173.662674453979));
#33419=CARTESIAN_POINT('Ctrl Pts',(-56.4605880039554,-106.801794621209,
173.639972028838));
#33420=CARTESIAN_POINT('Ctrl Pts',(-56.4886364834982,-106.796064858049,
173.617797875548));
#33421=CARTESIAN_POINT('Origin',(-54.1598171290174,-67.5719248685924,175.985485069079));
#33422=CARTESIAN_POINT('',(-56.2766244746021,-104.807333878735,173.617797875548));
#33423=CARTESIAN_POINT('',(-56.3296274768259,-105.304516623564,173.617797875548));
#33424=CARTESIAN_POINT('',(-52.327900808713,-67.7672193871761,173.617797875548));
#33425=CARTESIAN_POINT('Ctrl Pts',(-56.2766244746021,-104.807333878735,
173.617797875548));
#33426=CARTESIAN_POINT('Ctrl Pts',(-56.2653006888845,-104.809647109659,
173.626750067054));
#33427=CARTESIAN_POINT('Ctrl Pts',(-56.2540389651426,-104.811957373387,
173.635788627629));
#33428=CARTESIAN_POINT('Ctrl Pts',(-55.9345890254792,-104.877769330124,
173.896067820171));
#33429=CARTESIAN_POINT('Ctrl Pts',(-55.6799151601245,-104.93768930917,174.207509397213));
#33430=CARTESIAN_POINT('Ctrl Pts',(-55.3147130356128,-105.041298860261,
174.900745074777));
#33431=CARTESIAN_POINT('Ctrl Pts',(-55.2025963324754,-105.084204839733,
175.272948907266));
#33432=CARTESIAN_POINT('Ctrl Pts',(-55.1231106586534,-105.152786818001,
176.055839897832));
#33433=CARTESIAN_POINT('Ctrl Pts',(-55.1629339199115,-105.181310870104,
176.459638067914));
#33434=CARTESIAN_POINT('Ctrl Pts',(-55.3939647457702,-105.221359647692,
177.214442614334));
#33435=CARTESIAN_POINT('Ctrl Pts',(-55.5772773642361,-105.232777466452,
177.559723426792));
#33436=CARTESIAN_POINT('Ctrl Pts',(-56.0732763221029,-105.240005017301,
178.174455309114));
#33437=CARTESIAN_POINT('Ctrl Pts',(-56.3863200207768,-105.239401417322,
178.434191095882));
#33438=CARTESIAN_POINT('Ctrl Pts',(-57.0823383594249,-105.229880947087,
178.808625258783));
#33439=CARTESIAN_POINT('Ctrl Pts',(-57.4556744888722,-105.22104712134,178.924816364367));
#33440=CARTESIAN_POINT('Ctrl Pts',(-58.2404824815195,-105.197482048637,
179.011446458192));
#33441=CARTESIAN_POINT('Ctrl Pts',(-58.6454904306518,-105.187073952339,
178.9750310886));
#33442=CARTESIAN_POINT('Ctrl Pts',(-59.4029756075432,-105.17100212725,178.749834659797));
#33443=CARTESIAN_POINT('Ctrl Pts',(-59.7496561557124,-105.165015677895,
178.568892085678));
#33444=CARTESIAN_POINT('Ctrl Pts',(-60.3674653767356,-105.159250390754,
178.076670657764));
#33445=CARTESIAN_POINT('Ctrl Pts',(-60.6293166077287,-105.164103297252,
177.765411556099));
#33446=CARTESIAN_POINT('Ctrl Pts',(-61.0087231919709,-105.188338497418,
177.072418255627));
#33447=CARTESIAN_POINT('Ctrl Pts',(-61.1276608703734,-105.206636282563,
176.700279429192));
#33448=CARTESIAN_POINT('Ctrl Pts',(-61.2204148225146,-105.256842230424,
175.917401495486));
#33449=CARTESIAN_POINT('Ctrl Pts',(-61.1877962730522,-105.293087154001,
175.513545374999));
#33450=CARTESIAN_POINT('Ctrl Pts',(-60.9709343922714,-105.380889785063,
174.758523854962));
#33451=CARTESIAN_POINT('Ctrl Pts',(-60.7943863725805,-105.430693278442,
174.413091951295));
#33452=CARTESIAN_POINT('Ctrl Pts',(-60.3114591405253,-105.54226774086,173.797972982327));
#33453=CARTESIAN_POINT('Ctrl Pts',(-60.0054807927948,-105.607654245323,
173.53800282471));
#33454=CARTESIAN_POINT('Ctrl Pts',(-59.3233074853434,-105.745063326069,
173.163073072182));
#33455=CARTESIAN_POINT('Ctrl Pts',(-58.9565577567983,-105.815148211003,
173.046626790759));
#33456=CARTESIAN_POINT('Ctrl Pts',(-58.184430087075,-105.957550630314,172.959475878003));
#33457=CARTESIAN_POINT('Ctrl Pts',(-57.7862803003474,-106.03276285313,172.99563292452));
#33458=CARTESIAN_POINT('Ctrl Pts',(-57.0546783531652,-106.174361450359,
173.21660946132));
#33459=CARTESIAN_POINT('Ctrl Pts',(-56.7252249493366,-106.239724164121,
173.388856923705));
#33460=CARTESIAN_POINT('Ctrl Pts',(-56.4356334812743,-106.298882113221,
173.617797875548));
#33461=CARTESIAN_POINT('Ctrl Pts',(-56.4886364834982,-106.796064858049,
173.617797875548));
#33462=CARTESIAN_POINT('Ctrl Pts',(-56.7596693332081,-106.74069807658,173.403528722494));
#33463=CARTESIAN_POINT('Ctrl Pts',(-57.0658176208757,-106.679855420073,
173.238750333755));
#33464=CARTESIAN_POINT('Ctrl Pts',(-57.768903450155,-106.543369527441,173.007888959857));
#33465=CARTESIAN_POINT('Ctrl Pts',(-58.1650808581089,-106.468314870845,
172.962125616787));
#33466=CARTESIAN_POINT('Ctrl Pts',(-58.9374674226472,-106.325437595314,
173.02986875357));
#33467=CARTESIAN_POINT('Ctrl Pts',(-59.306375777374,-106.255834256616,173.136831075859));
#33468=CARTESIAN_POINT('Ctrl Pts',(-59.9962073277028,-106.117807896946,
173.493340806289));
#33469=CARTESIAN_POINT('Ctrl Pts',(-60.3079061661428,-106.051756025524,
173.74454746787));
#33470=CARTESIAN_POINT('Ctrl Pts',(-60.8055969341733,-105.93813031074,174.345219194373));
#33471=CARTESIAN_POINT('Ctrl Pts',(-60.9909278410113,-105.888146352887,
174.685066619392));
#33472=CARTESIAN_POINT('Ctrl Pts',(-61.2274212948024,-105.798464534594,
175.431962757536));
#33473=CARTESIAN_POINT('Ctrl Pts',(-61.270944175395,-105.760998732939,175.833536994212));
#33474=CARTESIAN_POINT('Ctrl Pts',(-61.2001876164997,-105.707938494202,
176.616743498004));
#33475=CARTESIAN_POINT('Ctrl Pts',(-61.0921055453824,-105.689285486627,
176.991276212819));
#33476=CARTESIAN_POINT('Ctrl Pts',(-60.7336426290013,-105.66304676212,177.693016934879));
#33477=CARTESIAN_POINT('Ctrl Pts',(-60.4817475119257,-105.657071142152,
178.010829710717));
#33478=CARTESIAN_POINT('Ctrl Pts',(-59.8803004238055,-105.660549212733,
178.52004077432));
#33479=CARTESIAN_POINT('Ctrl Pts',(-59.5400458076867,-105.666700898019,
178.710971772271));
#33480=CARTESIAN_POINT('Ctrl Pts',(-58.7918260736236,-105.682030791257,
178.958651454036));
#33481=CARTESIAN_POINT('Ctrl Pts',(-58.3894273848151,-105.692096451067,
179.007576569016));
#33482=CARTESIAN_POINT('Ctrl Pts',(-57.6042154056154,-105.715126122877,
178.946240936123));
#33483=CARTESIAN_POINT('Ctrl Pts',(-57.2282595229731,-105.725139729359,
178.842399324893));
#33484=CARTESIAN_POINT('Ctrl Pts',(-56.522384265223,-105.735974594548,178.491949605217));
#33485=CARTESIAN_POINT('Ctrl Pts',(-56.2019343365732,-105.737300525353,
178.243648763131));
#33486=CARTESIAN_POINT('Ctrl Pts',(-55.6866432506554,-105.731513670933,
177.64775703023));
#33487=CARTESIAN_POINT('Ctrl Pts',(-55.4921181006516,-105.722243834646,
177.309733209288));
#33488=CARTESIAN_POINT('Ctrl Pts',(-55.2356800943781,-105.685186175791,
176.565536774304));
#33489=CARTESIAN_POINT('Ctrl Pts',(-55.1816963441142,-105.658101573039,
176.164769489015));
#33490=CARTESIAN_POINT('Ctrl Pts',(-55.2324810832818,-105.591923835622,
175.381524112892));
#33491=CARTESIAN_POINT('Ctrl Pts',(-55.3307322750497,-105.551502685792,
175.006213016851));
#33492=CARTESIAN_POINT('Ctrl Pts',(-55.668832645442,-105.451085144376,174.301708294574));
#33493=CARTESIAN_POINT('Ctrl Pts',(-55.9105463702708,-105.392473767471,
173.981839983604));
#33494=CARTESIAN_POINT('Ctrl Pts',(-56.2474333770332,-105.321437836364,
173.684598278449));
#33495=CARTESIAN_POINT('Ctrl Pts',(-56.2881090861829,-105.312998029652,
173.650620872498));
#33496=CARTESIAN_POINT('Ctrl Pts',(-56.3296274768257,-105.304516623564,
173.617797875548));
#33497=CARTESIAN_POINT('Origin',(-54.1598171290174,-67.5719248685924,175.985485069079));
#33498=CARTESIAN_POINT('',(-56.1176154679299,-103.31578564425,173.617797875548));
#33499=CARTESIAN_POINT('',(-56.1706184701534,-103.812968389078,173.617797875548));
#33500=CARTESIAN_POINT('',(-52.327900808713,-67.7672193871761,173.617797875548));
#33501=CARTESIAN_POINT('Ctrl Pts',(-56.1176154679299,-103.31578564425,173.617797875548));
#33502=CARTESIAN_POINT('Ctrl Pts',(-56.1043250103344,-103.31850062829,173.628304849502));
#33503=CARTESIAN_POINT('Ctrl Pts',(-56.0911200963041,-103.321211514357,
173.638930756877));
#33504=CARTESIAN_POINT('Ctrl Pts',(-55.7704655142177,-103.387369689626,
173.901558773232));
#33505=CARTESIAN_POINT('Ctrl Pts',(-55.5166273065249,-103.447206792302,
174.213564632224));
#33506=CARTESIAN_POINT('Ctrl Pts',(-55.1531871492074,-103.550610059877,
174.907550219798));
#33507=CARTESIAN_POINT('Ctrl Pts',(-55.0419709606547,-103.593347093109,
175.27995563458));
#33508=CARTESIAN_POINT('Ctrl Pts',(-54.9643443732856,-103.661774607987,
176.062885655826));
#33509=CARTESIAN_POINT('Ctrl Pts',(-55.0050877700344,-103.690206374978,
176.466502692261));
#33510=CARTESIAN_POINT('Ctrl Pts',(-55.2377697079123,-103.730061973367,
177.22063307226));
#33511=CARTESIAN_POINT('Ctrl Pts',(-55.4218052661154,-103.741334665286,
177.565445136868));
#33512=CARTESIAN_POINT('Ctrl Pts',(-55.9190554664435,-103.748469568618,
178.178974772616));
#33513=CARTESIAN_POINT('Ctrl Pts',(-56.2325868532032,-103.747819406367,
178.437982466093));
#33514=CARTESIAN_POINT('Ctrl Pts',(-56.9292507462071,-103.738214153437,
178.810878113076));
#33515=CARTESIAN_POINT('Ctrl Pts',(-57.3027540248708,-103.729299028287,
178.926277061376));
#33516=CARTESIAN_POINT('Ctrl Pts',(-58.0876001328413,-103.705767849205,
179.011289843778));
#33517=CARTESIAN_POINT('Ctrl Pts',(-58.4924528567469,-103.695381373337,
178.97407247311));
#33518=CARTESIAN_POINT('Ctrl Pts',(-59.2493554969251,-103.679356802607,
178.747434357108));
#33519=CARTESIAN_POINT('Ctrl Pts',(-59.5956256336748,-103.673354907713,
178.565855111501));
#33520=CARTESIAN_POINT('Ctrl Pts',(-60.2124023796431,-103.667735045613,
178.072546163384));
#33521=CARTESIAN_POINT('Ctrl Pts',(-60.473626626211,-103.672659530759,177.760862023247));
#33522=CARTESIAN_POINT('Ctrl Pts',(-60.8517054991565,-103.697022462893,
177.067304060869));
#33523=CARTESIAN_POINT('Ctrl Pts',(-60.969954487591,-103.71533847361,176.695013679978));
#33524=CARTESIAN_POINT('Ctrl Pts',(-61.0613178783777,-103.765725594179,
175.912105661457));
#33525=CARTESIAN_POINT('Ctrl Pts',(-61.0280084599689,-103.802048593057,
175.508384995241));
#33526=CARTESIAN_POINT('Ctrl Pts',(-60.8099024547815,-103.889971010162,
174.753869651874));
#33527=CARTESIAN_POINT('Ctrl Pts',(-60.6328002879148,-103.939782129816,
174.408790054078));
#33528=CARTESIAN_POINT('Ctrl Pts',(-60.1489388748962,-104.051486847896,
173.794573999267));
#33529=CARTESIAN_POINT('Ctrl Pts',(-59.8425944395784,-104.116916509466,
173.535150572824));
#33530=CARTESIAN_POINT('Ctrl Pts',(-59.1599330169716,-104.25436567854,173.161376649719));
#33531=CARTESIAN_POINT('Ctrl Pts',(-58.7930476426981,-104.324417073302,
173.045525493603));
#33532=CARTESIAN_POINT('Ctrl Pts',(-58.0208968026134,-104.466850517053,
172.959589366222));
#33533=CARTESIAN_POINT('Ctrl Pts',(-57.6228638881136,-104.542054134394,
172.996348896332));
#33534=CARTESIAN_POINT('Ctrl Pts',(-56.8930427766736,-104.683334248274,
173.217979413356));
#33535=CARTESIAN_POINT('Ctrl Pts',(-56.5650553654821,-104.74841301316,173.389774435697));
#33536=CARTESIAN_POINT('Ctrl Pts',(-56.2766244746021,-104.807333878735,
173.617797875548));
#33537=CARTESIAN_POINT('Ctrl Pts',(-56.3296274768257,-105.304516623564,
173.617797875548));
#33538=CARTESIAN_POINT('Ctrl Pts',(-56.586763420517,-105.251988711846,173.414515133499));
#33539=CARTESIAN_POINT('Ctrl Pts',(-56.8756518272909,-105.194502166347,
173.255656785927));
#33540=CARTESIAN_POINT('Ctrl Pts',(-57.5573407106282,-105.061870497886,
173.018194256532));
#33541=CARTESIAN_POINT('Ctrl Pts',(-57.9518968201824,-104.986961694801,
172.965277848296));
#33542=CARTESIAN_POINT('Ctrl Pts',(-58.7243212130768,-104.843758468797,
173.018509289468));
#33543=CARTESIAN_POINT('Ctrl Pts',(-59.0948334933741,-104.774440321286,
173.118410470703));
#33544=CARTESIAN_POINT('Ctrl Pts',(-59.7901995520874,-104.635984124741,
173.461210596147));
#33545=CARTESIAN_POINT('Ctrl Pts',(-60.10599739235,-104.569468147798,173.70582815698));
#33546=CARTESIAN_POINT('Ctrl Pts',(-60.6145053935603,-104.454349598348,
174.29566698968));
#33547=CARTESIAN_POINT('Ctrl Pts',(-60.8063109448197,-104.404149819734,
174.6313980876));
#33548=CARTESIAN_POINT('Ctrl Pts',(-61.0571505412047,-104.313109652798,
175.37216866749));
#33549=CARTESIAN_POINT('Ctrl Pts',(-61.1086413032927,-104.274767358923,
175.771878782708));
#33550=CARTESIAN_POINT('Ctrl Pts',(-61.0540347236212,-104.219627528265,
176.555125379641));
#33551=CARTESIAN_POINT('Ctrl Pts',(-60.9538742878482,-104.200622191814,
176.931413228329));
#33552=CARTESIAN_POINT('Ctrl Pts',(-60.6107074521862,-104.172935338366,
177.63932970722));
#33553=CARTESIAN_POINT('Ctrl Pts',(-60.3661679600611,-104.166148788114,
177.961723631706));
#33554=CARTESIAN_POINT('Ctrl Pts',(-59.7767728721284,-104.167965410298,
178.483121614131));
#33555=CARTESIAN_POINT('Ctrl Pts',(-59.4411490653884,-104.174132651873,
178.681280605116));
#33556=CARTESIAN_POINT('Ctrl Pts',(-58.6997947488505,-104.188925309346,
178.945040591799));
#33557=CARTESIAN_POINT('Ctrl Pts',(-58.2995114737861,-104.198739234453,
179.002909619764));
#33558=CARTESIAN_POINT('Ctrl Pts',(-57.5142640536464,-104.221376908929,
178.959760465797));
#33559=CARTESIAN_POINT('Ctrl Pts',(-57.13641383133,-104.232117846913,178.864752057889));
#33560=CARTESIAN_POINT('Ctrl Pts',(-56.4321068286097,-104.243744947958,
178.535348806015));
#33561=CARTESIAN_POINT('Ctrl Pts',(-56.1131999486625,-104.245634487,178.302395783125));
#33562=CARTESIAN_POINT('Ctrl Pts',(-55.5795544736227,-104.241255906255,
177.725362130028));
#33563=CARTESIAN_POINT('Ctrl Pts',(-55.3708710635326,-104.233514167147,
177.385921844193));
#33564=CARTESIAN_POINT('Ctrl Pts',(-55.0963565925498,-104.198634152299,
176.64990001692));
#33565=CARTESIAN_POINT('Ctrl Pts',(-55.0320013973361,-104.173357805299,
176.26089693273));
#33566=CARTESIAN_POINT('Ctrl Pts',(-55.0552588305459,-104.109543147896,
175.478035139983));
#33567=CARTESIAN_POINT('Ctrl Pts',(-55.1437153211815,-104.070226160898,
175.09181330523));
#33568=CARTESIAN_POINT('Ctrl Pts',(-55.4618994607109,-103.972199550823,
174.379658006443));
#33569=CARTESIAN_POINT('Ctrl Pts',(-55.6876222709348,-103.915969317528,
174.060082353081));
#33570=CARTESIAN_POINT('Ctrl Pts',(-56.0329504084051,-103.841462858177,
173.731815046431));
#33571=CARTESIAN_POINT('Ctrl Pts',(-56.1005740309949,-103.827277116453,
173.673172575223));
#33572=CARTESIAN_POINT('Ctrl Pts',(-56.1706184701527,-103.812968389078,
173.617797875549));
#33573=CARTESIAN_POINT('Origin',(-54.1598171290174,-67.5719248685924,175.985485069079));
#33574=CARTESIAN_POINT('',(-55.9586064612577,-101.824237409764,173.617797875548));
#33575=CARTESIAN_POINT('',(-56.0116094634814,-102.321420154593,173.617797875548));
#33576=CARTESIAN_POINT('',(-52.327900808713,-67.7672193871761,173.617797875548));
#33577=CARTESIAN_POINT('Ctrl Pts',(-55.9586064612576,-101.824237409764,
173.617797875548));
#33578=CARTESIAN_POINT('Ctrl Pts',(-55.9418620792744,-101.827657963911,
173.631035402105));
#33579=CARTESIAN_POINT('Ctrl Pts',(-55.9252536280251,-101.831071983287,
173.644461594472));
#33580=CARTESIAN_POINT('Ctrl Pts',(-55.602506261032,-101.897836272007,173.911234848305));
#33581=CARTESIAN_POINT('Ctrl Pts',(-55.3501385871355,-101.957527023001,
174.224226559646));
#33582=CARTESIAN_POINT('Ctrl Pts',(-54.9897939381547,-102.060567461356,
174.919523761195));
#33583=CARTESIAN_POINT('Ctrl Pts',(-54.8801600543654,-102.103010161683,
175.29228342645));
#33584=CARTESIAN_POINT('Ctrl Pts',(-54.8058019006491,-102.171165691404,
176.075276683873));
#33585=CARTESIAN_POINT('Ctrl Pts',(-54.8481620778904,-102.199434886067,
176.478570168191));
#33586=CARTESIAN_POINT('Ctrl Pts',(-55.0837450049315,-102.238950667311,
177.231510942236));
#33587=CARTESIAN_POINT('Ctrl Pts',(-55.26905260861,-102.249970204585,177.575498479078));
#33588=CARTESIAN_POINT('Ctrl Pts',(-55.7685021015342,-102.256942000512,
178.186908434787));
#33589=CARTESIAN_POINT('Ctrl Pts',(-56.0828882984817,-102.256209898393,
178.444631835812));
#33590=CARTESIAN_POINT('Ctrl Pts',(-56.7806847889233,-102.246455470237,
178.814817605309));
#33591=CARTESIAN_POINT('Ctrl Pts',(-57.1544827460279,-102.23739901161,178.928821322706));
#33592=CARTESIAN_POINT('Ctrl Pts',(-57.9393919543218,-102.213927680494,
179.010983698272));
#33593=CARTESIAN_POINT('Ctrl Pts',(-58.3439672415085,-102.203579401748,
178.97235351188));
#33594=CARTESIAN_POINT('Ctrl Pts',(-59.0998399032848,-102.1876381752,178.743175887637));
#33595=CARTESIAN_POINT('Ctrl Pts',(-59.4453865710874,-102.181610661658,
178.560473933994));
#33596=CARTESIAN_POINT('Ctrl Pts',(-60.0603391240182,-102.176247373325,
178.065248679065));
#33597=CARTESIAN_POINT('Ctrl Pts',(-60.3204551505627,-102.181298084424,
177.752817376281));
#33598=CARTESIAN_POINT('Ctrl Pts',(-60.6961902382117,-102.205886260206,
177.058265992882));
#33599=CARTESIAN_POINT('Ctrl Pts',(-60.8132236920275,-102.224235850889,
176.685708027717));
#33600=CARTESIAN_POINT('Ctrl Pts',(-60.9021310470988,-102.27494271889,175.90274993751));
#33601=CARTESIAN_POINT('Ctrl Pts',(-60.8676018815838,-102.311403324081,
175.499271413988));
#33602=CARTESIAN_POINT('Ctrl Pts',(-60.6472995091625,-102.399536981531,
174.745652556018));
#33603=CARTESIAN_POINT('Ctrl Pts',(-60.4692182742589,-102.449362802166,
174.40119543767));
#33604=CARTESIAN_POINT('Ctrl Pts',(-59.9837071749626,-102.561297391055,
173.788577520703));
#33605=CARTESIAN_POINT('Ctrl Pts',(-59.6767175857298,-102.626802922418,
173.530122137022));
#33606=CARTESIAN_POINT('Ctrl Pts',(-58.9931953493747,-102.764322547424,
173.158392483586));
#33607=CARTESIAN_POINT('Ctrl Pts',(-58.6260701402944,-102.834315775566,
173.043593874296));
#33608=CARTESIAN_POINT('Ctrl Pts',(-57.8538805758677,-102.976803691064,
172.959807279232));
#33609=CARTESIAN_POINT('Ctrl Pts',(-57.4560566189888,-103.051991670284,
172.997632518835));
#33610=CARTESIAN_POINT('Ctrl Pts',(-56.7293880942506,-103.192707713498,
173.220408735396));
#33611=CARTESIAN_POINT('Ctrl Pts',(-56.4039923758953,-103.257284367751,
173.391398243217));
#33612=CARTESIAN_POINT('Ctrl Pts',(-56.1176154679299,-103.31578564425,173.617797875548));
#33613=CARTESIAN_POINT('Ctrl Pts',(-56.1706184701527,-103.812968389078,
173.617797875549));
#33614=CARTESIAN_POINT('Ctrl Pts',(-56.404804740164,-103.765128652867,173.432658348049));
#33615=CARTESIAN_POINT('Ctrl Pts',(-56.6655756121463,-103.713125305891,
173.28416603257));
#33616=CARTESIAN_POINT('Ctrl Pts',(-57.3044614716826,-103.588350311415,
173.040169017636));
#33617=CARTESIAN_POINT('Ctrl Pts',(-57.6876611425556,-103.515301776179,
172.975313466901));
#33618=CARTESIAN_POINT('Ctrl Pts',(-58.459499061551,-103.371543657016,172.998304157061));
#33619=CARTESIAN_POINT('Ctrl Pts',(-58.8405222939703,-103.301242302207,
173.086729527027));
#33620=CARTESIAN_POINT('Ctrl Pts',(-59.544647309321,-103.162157013392,173.40658130172));
#33621=CARTESIAN_POINT('Ctrl Pts',(-59.8614447323563,-103.096156684249,
173.634213697219));
#33622=CARTESIAN_POINT('Ctrl Pts',(-60.3916584272211,-102.978084198385,
174.201298967928));
#33623=CARTESIAN_POINT('Ctrl Pts',(-60.5994160828054,-102.926356504137,
174.535657821284));
#33624=CARTESIAN_POINT('Ctrl Pts',(-60.8740312425169,-102.833106151377,
175.265760314739));
#33625=CARTESIAN_POINT('Ctrl Pts',(-60.93892768182,-102.793929024314,175.654271971896));
#33626=CARTESIAN_POINT('Ctrl Pts',(-60.9169777722008,-102.734645718886,
176.436822929872));
#33627=CARTESIAN_POINT('Ctrl Pts',(-60.8298978453232,-102.714451234301,
176.82326307178));
#33628=CARTESIAN_POINT('Ctrl Pts',(-60.512540236509,-102.684358018243,177.541078380302));
#33629=CARTESIAN_POINT('Ctrl Pts',(-60.285789784968,-102.676240964764,177.865680022517));
#33630=CARTESIAN_POINT('Ctrl Pts',(-59.7209647535357,-102.674754719218,
178.410737605796));
#33631=CARTESIAN_POINT('Ctrl Pts',(-59.3882039794029,-102.680851603804,
178.625795338374));
#33632=CARTESIAN_POINT('Ctrl Pts',(-58.6588191637221,-102.694734749673,
178.916334908194));
#33633=CARTESIAN_POINT('Ctrl Pts',(-58.2694213622247,-102.703925358076,
178.989125475152));
#33634=CARTESIAN_POINT('Ctrl Pts',(-57.4849943314814,-102.725771328283,
178.981565949238));
#33635=CARTESIAN_POINT('Ctrl Pts',(-57.0975304536677,-102.737798083385,
178.901359005251));
#33636=CARTESIAN_POINT('Ctrl Pts',(-56.373984974966,-102.751112893838,178.596975999604));
#33637=CARTESIAN_POINT('Ctrl Pts',(-56.0450780673281,-102.75382305394,178.37562206328));
#33638=CARTESIAN_POINT('Ctrl Pts',(-55.4909578422365,-102.751036339809,
177.820144068511));
#33639=CARTESIAN_POINT('Ctrl Pts',(-55.2708822806514,-102.745313930212,
177.491617213069));
#33640=CARTESIAN_POINT('Ctrl Pts',(-54.9672570694395,-102.713919309601,
176.768487387816));
#33641=CARTESIAN_POINT('Ctrl Pts',(-54.8871168552745,-102.690077603063,
176.380711597023));
#33642=CARTESIAN_POINT('Ctrl Pts',(-54.8796652807629,-102.628930472901,
175.598674121186));
#33643=CARTESIAN_POINT('Ctrl Pts',(-54.9518913884919,-102.592139071519,
175.211999444296));
#33644=CARTESIAN_POINT('Ctrl Pts',(-55.2394031848712,-102.497784884128,
174.487925439198));
#33645=CARTESIAN_POINT('Ctrl Pts',(-55.4526238491403,-102.442637439968,
174.157716548369));
#33646=CARTESIAN_POINT('Ctrl Pts',(-55.8135995248757,-102.362651165773,
173.785235233275));
#33647=CARTESIAN_POINT('Ctrl Pts',(-55.9100255219117,-102.342171793738,
173.698106609885));
#33648=CARTESIAN_POINT('Ctrl Pts',(-56.0116094634811,-102.321420154593,
173.617797875548));
#33649=CARTESIAN_POINT('Origin',(-54.1598171290174,-67.5719248685924,175.985485069079));
#33650=CARTESIAN_POINT('',(-55.7995974545854,-100.332689175279,173.617797875548));
#33651=CARTESIAN_POINT('',(-55.8526004568095,-100.829871920107,173.617797875548));
#33652=CARTESIAN_POINT('',(-52.327900808713,-67.7672193871761,173.617797875548));
#33653=CARTESIAN_POINT('Ctrl Pts',(-55.7995974545853,-100.332689175279,
173.617797875548));
#33654=CARTESIAN_POINT('Ctrl Pts',(-55.7768768391306,-100.337330558609,
173.635760004624));
#33655=CARTESIAN_POINT('Ctrl Pts',(-55.7544069815204,-100.341959811824,
173.654069124129));
#33656=CARTESIAN_POINT('Ctrl Pts',(-55.4281078338695,-100.409766928785,
173.928074962219));
#33657=CARTESIAN_POINT('Ctrl Pts',(-55.1782933068223,-100.469202046876,
174.242756886089));
#33658=CARTESIAN_POINT('Ctrl Pts',(-54.8233080316795,-100.571613042545,
174.940307330757));
#33659=CARTESIAN_POINT('Ctrl Pts',(-54.7164144709026,-100.613553643858,
175.31368069076));
#33660=CARTESIAN_POINT('Ctrl Pts',(-54.6477220275006,-100.681236411179,
176.096767285812));
#33661=CARTESIAN_POINT('Ctrl Pts',(-54.692882020349,-100.709222813559,176.499484491269));
#33662=CARTESIAN_POINT('Ctrl Pts',(-54.9334882488888,-100.748148956567,
177.250349960554));
#33663=CARTESIAN_POINT('Ctrl Pts',(-55.1210041782264,-100.758735702979,
177.592906895632));
#33664=CARTESIAN_POINT('Ctrl Pts',(-55.624264502085,-100.765424077113,178.200624182367));
#33665=CARTESIAN_POINT('Ctrl Pts',(-55.9401245508787,-100.764549700056,
178.456108510789));
#33666=CARTESIAN_POINT('Ctrl Pts',(-56.639877235172,-100.754536320114,178.821581568571));
#33667=CARTESIAN_POINT('Ctrl Pts',(-57.0141885239434,-100.745239747563,
178.933158919805));
#33668=CARTESIAN_POINT('Ctrl Pts',(-57.7991951657605,-100.721872951851,
179.010358891003));
#33669=CARTESIAN_POINT('Ctrl Pts',(-58.2032756935156,-100.71159145232,178.969271146376));
#33670=CARTESIAN_POINT('Ctrl Pts',(-58.9573451962122,-100.69579551028,178.735676551618));
#33671=CARTESIAN_POINT('Ctrl Pts',(-59.3016318924727,-100.689728304205,
178.551018089997));
#33672=CARTESIAN_POINT('Ctrl Pts',(-59.9133948054434,-100.684812524346,
178.052457832929));
#33673=CARTESIAN_POINT('Ctrl Pts',(-60.1715717458335,-100.690083204903,
177.738731743298));
#33674=CARTESIAN_POINT('Ctrl Pts',(-60.5432149011014,-100.715063895377,
177.042456253659));
#33675=CARTESIAN_POINT('Ctrl Pts',(-60.6581267585883,-100.733476433594,
176.669430948199));
#33676=CARTESIAN_POINT('Ctrl Pts',(-60.7427422172093,-100.784741310593,
175.886394761431));
#33677=CARTESIAN_POINT('Ctrl Pts',(-60.7060830699926,-100.82144148114,175.483348270929));
#33678=CARTESIAN_POINT('Ctrl Pts',(-60.4819457218199,-100.909943273934,
174.731303566548));
#33679=CARTESIAN_POINT('Ctrl Pts',(-60.3021525491174,-100.959798580448,
174.387934937461));
#33680=CARTESIAN_POINT('Ctrl Pts',(-59.8137595275919,-101.072134280656,
173.778120185689));
#33681=CARTESIAN_POINT('Ctrl Pts',(-59.5056469930805,-101.137771296492,
173.521363784633));
#33682=CARTESIAN_POINT('Ctrl Pts',(-58.8206245124076,-101.275412969076,
173.153215134721));
#33683=CARTESIAN_POINT('Ctrl Pts',(-58.453079395942,-101.345307598008,173.040260243925));
#33684=CARTESIAN_POINT('Ctrl Pts',(-57.6808289635357,-101.487889698087,
172.96024209395));
#33685=CARTESIAN_POINT('Ctrl Pts',(-57.2833779854965,-101.563048993529,
172.999934506361));
#33686=CARTESIAN_POINT('Ctrl Pts',(-56.5622407027566,-101.702774554781,
173.224683780349));
#33687=CARTESIAN_POINT('Ctrl Pts',(-56.2413813271945,-101.766471960948,
173.39424589248));
#33688=CARTESIAN_POINT('Ctrl Pts',(-55.9586064612576,-101.824237409764,
173.617797875548));
#33689=CARTESIAN_POINT('Ctrl Pts',(-56.0116094634811,-102.321420154593,
173.617797875548));
#33690=CARTESIAN_POINT('Ctrl Pts',(-56.2117256298421,-102.280540283156,
173.459592988117));
#33691=CARTESIAN_POINT('Ctrl Pts',(-56.4315113442584,-102.236567527639,
173.32794348206));
#33692=CARTESIAN_POINT('Ctrl Pts',(-57.0210459134878,-102.120764142274,
173.072451862829));
#33693=CARTESIAN_POINT('Ctrl Pts',(-57.4027420083367,-102.04762488143,172.990678263125));
#33694=CARTESIAN_POINT('Ctrl Pts',(-58.1734791760833,-101.903350281501,
172.980801890339));
#33695=CARTESIAN_POINT('Ctrl Pts',(-58.555048337918,-101.833753291797,173.051813399071));
#33696=CARTESIAN_POINT('Ctrl Pts',(-59.2716187222599,-101.693785878013,
173.338771470462));
#33697=CARTESIAN_POINT('Ctrl Pts',(-59.59950055985,-101.626352796783,173.552932301273));
#33698=CARTESIAN_POINT('Ctrl Pts',(-60.152626675811,-101.505191935652,174.095270609366));
#33699=CARTESIAN_POINT('Ctrl Pts',(-60.3733722096372,-101.452818719277,
174.417318372121));
#33700=CARTESIAN_POINT('Ctrl Pts',(-60.6807670840991,-101.356539785396,
175.132477821969));
#33701=CARTESIAN_POINT('Ctrl Pts',(-60.7634495819521,-101.31521637537,175.519219398591));
#33702=CARTESIAN_POINT('Ctrl Pts',(-60.7760051648476,-101.251598266524,
176.300490372137));
#33703=CARTESIAN_POINT('Ctrl Pts',(-60.7072285105988,-101.230163282846,
176.687412322417));
#33704=CARTESIAN_POINT('Ctrl Pts',(-60.4244698747711,-101.196868880839,
177.418150190422));
#33705=CARTESIAN_POINT('Ctrl Pts',(-60.2119626544106,-101.186985144412,
177.754385613528));
#33706=CARTESIAN_POINT('Ctrl Pts',(-59.6731240769558,-101.18206326524,178.323655970417));
#33707=CARTESIAN_POINT('Ctrl Pts',(-59.3532738220543,-101.187461424002,
178.552315730304));
#33708=CARTESIAN_POINT('Ctrl Pts',(-58.6397518992478,-101.200161996454,
178.877291385991));
#33709=CARTESIAN_POINT('Ctrl Pts',(-58.2523927315438,-101.208889944517,
178.968885456107));
#33710=CARTESIAN_POINT('Ctrl Pts',(-57.4694270027641,-101.229907422773,
178.997798186083));
#33711=CARTESIAN_POINT('Ctrl Pts',(-57.0815394412167,-101.242619116289,
178.93672303185));
#33712=CARTESIAN_POINT('Ctrl Pts',(-56.3448618659264,-101.257863366675,
178.668720994274));
#33713=CARTESIAN_POINT('Ctrl Pts',(-56.0040013908307,-101.261606484908,
178.462523802351));
#33714=CARTESIAN_POINT('Ctrl Pts',(-55.4248118944299,-101.260813912043,
177.934557342879));
#33715=CARTESIAN_POINT('Ctrl Pts',(-55.1907517584213,-101.257179714369,
177.619451304459));
#33716=CARTESIAN_POINT('Ctrl Pts',(-54.8516849912401,-101.230113400579,
176.913092274527));
#33717=CARTESIAN_POINT('Ctrl Pts',(-54.7520715760218,-101.208111268598,
176.527713217197));
#33718=CARTESIAN_POINT('Ctrl Pts',(-54.7068453558597,-101.150308825965,
175.747492359658));
#33719=CARTESIAN_POINT('Ctrl Pts',(-54.7594532240998,-101.116159496669,
175.36031299947));
#33720=CARTESIAN_POINT('Ctrl Pts',(-55.0094861140096,-101.026370753261,
174.62276410895));
#33721=CARTESIAN_POINT('Ctrl Pts',(-55.2069070993651,-100.972677229107,
174.280310302316));
#33722=CARTESIAN_POINT('Ctrl Pts',(-55.5827888417636,-100.88647057148,173.851760673119));
#33723=CARTESIAN_POINT('Ctrl Pts',(-55.7127247867848,-100.858445820516,
173.72837871983));
#33724=CARTESIAN_POINT('Ctrl Pts',(-55.8526004568095,-100.829871920107,
173.617797875548));
#33725=CARTESIAN_POINT('Origin',(-54.1598171290174,-67.5719248685924,175.985485069079));
#33726=CARTESIAN_POINT('',(-55.6405884479131,-98.8411409407929,173.617797875548));
#33727=CARTESIAN_POINT('',(-55.6935914501374,-99.3383236856214,173.617797875548));
#33728=CARTESIAN_POINT('',(-52.327900808713,-67.7672193871761,173.617797875548));
#33729=CARTESIAN_POINT('Ctrl Pts',(-55.640588447913,-98.8411409407929,173.617797875548));
#33730=CARTESIAN_POINT('Ctrl Pts',(-55.607788426525,-98.8478413522682,173.643728432713));
#33731=CARTESIAN_POINT('Ctrl Pts',(-55.575512754977,-98.8545161247301,173.670380738806));
#33732=CARTESIAN_POINT('Ctrl Pts',(-55.2434249722054,-98.9240644878506,
173.956755143452));
#33733=CARTESIAN_POINT('Ctrl Pts',(-54.9979411072923,-98.983061603104,174.274242696089));
#33734=CARTESIAN_POINT('Ctrl Pts',(-54.6520043673395,-99.0844062653321,
174.975547078861));
#33735=CARTESIAN_POINT('Ctrl Pts',(-54.5497403041806,-99.1255207794924,
175.349957929002));
#33736=CARTESIAN_POINT('Ctrl Pts',(-54.490633611945,-99.1923999624474,176.133155312395));
#33737=CARTESIAN_POINT('Ctrl Pts',(-54.5405219281655,-99.2199051296011,
176.534853017101));
#33738=CARTESIAN_POINT('Ctrl Pts',(-54.7896112751938,-99.2578320053393,
177.282169330645));
#33739=CARTESIAN_POINT('Ctrl Pts',(-54.9808733909374,-99.2677041213008,
177.622301954674));
#33740=CARTESIAN_POINT('Ctrl Pts',(-55.4905764275471,-99.273911004575,178.223718473287));
#33741=CARTESIAN_POINT('Ctrl Pts',(-55.80890658979,-99.2727952582687,178.475377649671));
#33742=CARTESIAN_POINT('Ctrl Pts',(-56.5119481278214,-99.2623427169079,
178.832833145827));
#33743=CARTESIAN_POINT('Ctrl Pts',(-56.8871354514819,-99.2526542811345,
178.940282456497));
#33744=CARTESIAN_POINT('Ctrl Pts',(-57.6722717244173,-99.2294666609831,
179.009024583519));
#33745=CARTESIAN_POINT('Ctrl Pts',(-58.0754745824138,-99.2192997909092,
178.963754653268));
#33746=CARTESIAN_POINT('Ctrl Pts',(-58.8264415096819,-99.2037520153808,
178.722644060913));
#33747=CARTESIAN_POINT('Ctrl Pts',(-59.168579358959,-99.1976316660925,178.534644993543));
#33748=CARTESIAN_POINT('Ctrl Pts',(-59.7748651888666,-99.1934810387267,
178.030404263522));
#33749=CARTESIAN_POINT('Ctrl Pts',(-60.0297087292874,-99.1991272360973,
177.714489261805));
#33750=CARTESIAN_POINT('Ctrl Pts',(-60.3943437977552,-99.2247780241239,
177.01529115874));
#33751=CARTESIAN_POINT('Ctrl Pts',(-60.5056235297006,-99.2433112190769,
176.64146480497));
#33752=CARTESIAN_POINT('Ctrl Pts',(-60.582876625282,-99.2955310960124,175.858322552814));
#33753=CARTESIAN_POINT('Ctrl Pts',(-60.5425684063517,-99.3326395226713,
175.456043508555));
#33754=CARTESIAN_POINT('Ctrl Pts',(-60.3118618363862,-99.4217698445741,
174.706721474383));
#33755=CARTESIAN_POINT('Ctrl Pts',(-60.1291287544452,-99.4716870873749,
174.36522220523));
#33756=CARTESIAN_POINT('Ctrl Pts',(-59.6357948033637,-99.5847090949079,
173.760247118106));
#33757=CARTESIAN_POINT('Ctrl Pts',(-59.3257694087996,-99.6505683657844,
173.506426873974));
#33758=CARTESIAN_POINT('Ctrl Pts',(-58.6381854022676,-99.7884161986188,
173.144446851875));
#33759=CARTESIAN_POINT('Ctrl Pts',(-58.2699175162785,-99.8581508629596,
173.034667925421));
#33760=CARTESIAN_POINT('Ctrl Pts',(-57.4975831329424,-100.000891499135,
172.961150408848));
#33761=CARTESIAN_POINT('Ctrl Pts',(-57.1007954373251,-100.075997516825,
173.004060058922));
#33762=CARTESIAN_POINT('Ctrl Pts',(-56.3892116996093,-100.214009883933,
173.232106306747));
#33763=CARTESIAN_POINT('Ctrl Pts',(-56.0761555924101,-100.276193684061,
173.399160621705));
#33764=CARTESIAN_POINT('Ctrl Pts',(-55.7995974545854,-100.332689175279,
173.617797875548));
#33765=CARTESIAN_POINT('Ctrl Pts',(-55.8526004568095,-100.829871920107,
173.617797875548));
#33766=CARTESIAN_POINT('Ctrl Pts',(-56.0122382705985,-100.797260995049,
173.491593767107));
#33767=CARTESIAN_POINT('Ctrl Pts',(-56.1846045510077,-100.762638723928,
173.382123827381));
#33768=CARTESIAN_POINT('Ctrl Pts',(-56.7157333838001,-100.657561827589,
173.117982968677));
#33769=CARTESIAN_POINT('Ctrl Pts',(-57.094698693149,-100.584490179927,173.016058522839));
#33770=CARTESIAN_POINT('Ctrl Pts',(-57.8632760701796,-100.439761135245,
172.967130150488));
#33771=CARTESIAN_POINT('Ctrl Pts',(-58.2454035950996,-100.370550178192,
173.0178651937));
#33772=CARTESIAN_POINT('Ctrl Pts',(-58.9755114142945,-100.229746977069,
173.266016957432));
#33773=CARTESIAN_POINT('Ctrl Pts',(-59.3156712917826,-100.160789298229,
173.463728513916));
#33774=CARTESIAN_POINT('Ctrl Pts',(-59.8949166349951,-100.036160879726,
173.97655855762));
#33775=CARTESIAN_POINT('Ctrl Pts',(-60.1304479748,-99.9825994660196,174.284510981315));
#33776=CARTESIAN_POINT('Ctrl Pts',(-60.4749888012005,-99.8829850771357,
174.981520655192));
#33777=CARTESIAN_POINT('Ctrl Pts',(-60.5780912424543,-99.8392777678074,
175.365219219352));
#33778=CARTESIAN_POINT('Ctrl Pts',(-60.6301874634811,-99.7707646401272,
176.144112017309));
#33779=CARTESIAN_POINT('Ctrl Pts',(-60.5819096245653,-99.7474725453235,
176.531552855466));
#33780=CARTESIAN_POINT('Ctrl Pts',(-60.3384998584582,-99.7106236091981,
177.275775863669));
#33781=CARTESIAN_POINT('Ctrl Pts',(-60.142764833812,-99.698754297114,177.624377307971));
#33782=CARTESIAN_POINT('Ctrl Pts',(-59.6338082020946,-99.6899722706143,
178.220216958606));
#33783=CARTESIAN_POINT('Ctrl Pts',(-59.3281466891011,-99.6941240637893,
178.463851602083));
#33784=CARTESIAN_POINT('Ctrl Pts',(-58.6331919999401,-99.7054999209037,
178.826382081363));
#33785=CARTESIAN_POINT('Ctrl Pts',(-58.2491406899139,-99.713687805704,178.938738164386));
#33786=CARTESIAN_POINT('Ctrl Pts',(-57.4687325225704,-99.7337650841091,
179.007890508407));
#33787=CARTESIAN_POINT('Ctrl Pts',(-57.0803506489573,-99.7467323005111,
178.967502295266));
#33788=CARTESIAN_POINT('Ctrl Pts',(-56.3305357616791,-99.7640445546346,
178.739317008762));
#33789=CARTESIAN_POINT('Ctrl Pts',(-55.9774945802472,-99.7689094944188,
178.550283591324));
#33790=CARTESIAN_POINT('Ctrl Pts',(-55.3718512221691,-99.7702782468859,
178.052764535689));
#33791=CARTESIAN_POINT('Ctrl Pts',(-55.1229119696622,-99.7683688291766,
177.751904538663));
#33792=CARTESIAN_POINT('Ctrl Pts',(-54.7466827634431,-99.7459428741996,
177.064420399678));
#33793=CARTESIAN_POINT('Ctrl Pts',(-54.6264136550257,-99.7259772250701,
176.682662160461));
#33794=CARTESIAN_POINT('Ctrl Pts',(-54.5411023803683,-99.6717996406146,
175.905326025461));
#33795=CARTESIAN_POINT('Ctrl Pts',(-54.5732422656808,-99.6399064579199,
175.517630649645));
#33796=CARTESIAN_POINT('Ctrl Pts',(-54.7838400046977,-99.5550096737611,
174.767133841076));
#33797=CARTESIAN_POINT('Ctrl Pts',(-54.9640775679547,-99.5029939958601,
174.412709780171));
#33798=CARTESIAN_POINT('Ctrl Pts',(-55.3505156020313,-99.4108574829576,
173.92319016178));
#33799=CARTESIAN_POINT('Ctrl Pts',(-55.5136939909607,-99.3750732653116,
173.760018555645));
#33800=CARTESIAN_POINT('Ctrl Pts',(-55.6935914501376,-99.3383236856213,
173.617797875548));
#33801=CARTESIAN_POINT('Origin',(-54.1598171290174,-67.5719248685924,175.985485069079));
#33802=CARTESIAN_POINT('',(-55.4815794412406,-97.3495927063074,173.617797875548));
#33803=CARTESIAN_POINT('',(-55.5345824434656,-97.8467754511356,173.617797875547));
#33804=CARTESIAN_POINT('',(-52.327900808713,-67.7672193871761,173.617797875548));
#33805=CARTESIAN_POINT('Ctrl Pts',(-55.4815794412403,-97.3495927063074,
173.617797875548));
#33806=CARTESIAN_POINT('Ctrl Pts',(-55.4324890366522,-97.3596209287386,
173.656607043608));
#33807=CARTESIAN_POINT('Ctrl Pts',(-55.3845798951133,-97.3695903433992,
173.697027556825));
#33808=CARTESIAN_POINT('Ctrl Pts',(-55.0436838390214,-97.4419036621428,
174.003831822454));
#33809=CARTESIAN_POINT('Ctrl Pts',(-54.8052622584124,-97.5001748970722,
174.325732895783));
#33810=CARTESIAN_POINT('Ctrl Pts',(-54.4739751665481,-97.5997836371241,
175.032982163991));
#33811=CARTESIAN_POINT('Ctrl Pts',(-54.3792161531924,-97.6396186592439,
175.40907756234));
#33812=CARTESIAN_POINT('Ctrl Pts',(-54.3356822249732,-97.705182341791,176.192328114917));
#33813=CARTESIAN_POINT('Ctrl Pts',(-54.3932265261256,-97.7318984584026,
176.592250427641));
#33814=CARTESIAN_POINT('Ctrl Pts',(-54.6560551944903,-97.7681974970615,
177.33369930248));
#33815=CARTESIAN_POINT('Ctrl Pts',(-54.853432028735,-97.7769564622805,177.669882492492));
#33816=CARTESIAN_POINT('Ctrl Pts',(-55.3735876312399,-97.7823758155381,
178.260918672993));
#33817=CARTESIAN_POINT('Ctrl Pts',(-55.695865173458,-97.7808662960632,178.506265131895));
#33818=CARTESIAN_POINT('Ctrl Pts',(-56.4041928409522,-97.7696975138237,
178.850576320867));
#33819=CARTESIAN_POINT('Ctrl Pts',(-56.7808247104566,-97.7594122769474,
178.951256000448));
#33820=CARTESIAN_POINT('Ctrl Pts',(-57.5660739648741,-97.736522069505,179.006089715428));
#33821=CARTESIAN_POINT('Ctrl Pts',(-57.9677393275844,-97.7265458884034,
178.953961714379));
#33822=CARTESIAN_POINT('Ctrl Pts',(-58.7135241150777,-97.7114077004069,
178.700524956017));
#33823=CARTESIAN_POINT('Ctrl Pts',(-59.0521242732877,-97.7052403557551,
178.507014713227));
#33824=CARTESIAN_POINT('Ctrl Pts',(-59.6492906014397,-97.702354641487,177.993443668406));
#33825=CARTESIAN_POINT('Ctrl Pts',(-59.8985748487986,-97.7086198657127,
177.6739799838));
#33826=CARTESIAN_POINT('Ctrl Pts',(-60.2515922105049,-97.7353755898406,
176.970020213686));
#33827=CARTESIAN_POINT('Ctrl Pts',(-60.3568537551407,-97.7541449326304,
176.594863477064));
#33828=CARTESIAN_POINT('Ctrl Pts',(-60.4218689325865,-97.8079460282848,
175.811623141943));
#33829=CARTESIAN_POINT('Ctrl Pts',(-60.3755094456941,-97.8457253912998,
175.410693317903));
#33830=CARTESIAN_POINT('Ctrl Pts',(-60.1339094023174,-97.9358921711707,
174.665959338533));
#33831=CARTESIAN_POINT('Ctrl Pts',(-59.9462795676491,-97.9859446250264,
174.327573621966));
#33832=CARTESIAN_POINT('Ctrl Pts',(-59.4447409410051,-98.1001023645264,
173.730730865837));
#33833=CARTESIAN_POINT('Ctrl Pts',(-59.1315747563405,-98.1663216537997,
173.481851668649));
#33834=CARTESIAN_POINT('Ctrl Pts',(-58.4397669818307,-98.3045031186173,
173.130197603657));
#33835=CARTESIAN_POINT('Ctrl Pts',(-58.0702903996877,-98.3739982357447,
173.025735741239));
#33836=CARTESIAN_POINT('Ctrl Pts',(-57.2978751733484,-98.5169936655727,
172.96312581397));
#33837=CARTESIAN_POINT('Ctrl Pts',(-56.9022569518373,-98.5919994740118,
173.011422547399));
#33838=CARTESIAN_POINT('Ctrl Pts',(-56.2067337174236,-98.7271248655238,
173.244696526083));
#33839=CARTESIAN_POINT('Ctrl Pts',(-55.9067072812291,-98.7867779980545,
173.407413573101));
#33840=CARTESIAN_POINT('Ctrl Pts',(-55.640588447913,-98.8411409407929,173.617797875548));
#33841=CARTESIAN_POINT('Ctrl Pts',(-55.6935914501376,-99.3383236856214,
173.617797875548));
#33842=CARTESIAN_POINT('Ctrl Pts',(-55.8119561040419,-99.3141440707393,
173.52422289314));
#33843=CARTESIAN_POINT('Ctrl Pts',(-55.9374403171867,-99.2888338257374,
173.439753139739));
#33844=CARTESIAN_POINT('Ctrl Pts',(-56.4097362742124,-99.1946815732135,
173.172347526528));
#33845=CARTESIAN_POINT('Ctrl Pts',(-56.7848532814029,-99.1218779352154,
173.049886449515));
#33846=CARTESIAN_POINT('Ctrl Pts',(-57.550288318462,-98.9768606303945,172.961111387978));
#33847=CARTESIAN_POINT('Ctrl Pts',(-57.9329176837078,-98.9075434504376,
172.991548501756));
#33848=CARTESIAN_POINT('Ctrl Pts',(-58.6755232042986,-98.7661086789391,
173.200450042894));
#33849=CARTESIAN_POINT('Ctrl Pts',(-59.0271977849536,-98.6957931179957,
173.38097589479));
#33850=CARTESIAN_POINT('Ctrl Pts',(-59.6319148992309,-98.5678406174091,
173.863622452769));
#33851=CARTESIAN_POINT('Ctrl Pts',(-59.8819084866275,-98.5126235340329,
174.157734558481));
#33852=CARTESIAN_POINT('Ctrl Pts',(-60.2624486880925,-98.4098755731448,
174.835908151001));
#33853=CARTESIAN_POINT('Ctrl Pts',(-60.38553977356,-98.3639189197615,175.215566976975));
#33854=CARTESIAN_POINT('Ctrl Pts',(-60.4764166993533,-98.2906788232303,
175.991195226444));
#33855=CARTESIAN_POINT('Ctrl Pts',(-60.4478242869101,-98.2651150805417,
176.379140518398));
#33856=CARTESIAN_POINT('Ctrl Pts',(-60.2426635425665,-98.2248942633597,
177.135299993822));
#33857=CARTESIAN_POINT('Ctrl Pts',(-60.0637521456281,-98.211124838614,177.495017551851));
#33858=CARTESIAN_POINT('Ctrl Pts',(-59.5841734003338,-98.1986352035317,
178.115748546278));
#33859=CARTESIAN_POINT('Ctrl Pts',(-59.2918518313182,-98.2011354802375,
178.373532359831));
#33860=CARTESIAN_POINT('Ctrl Pts',(-58.6153963646659,-98.2112443778198,
178.771031797104));
#33861=CARTESIAN_POINT('Ctrl Pts',(-58.2354796130484,-98.2188965152296,
178.902892638674));
#33862=CARTESIAN_POINT('Ctrl Pts',(-57.4583833275023,-98.238062825233,179.009966870332));
#33863=CARTESIAN_POINT('Ctrl Pts',(-57.0694769111357,-98.2508035073108,
178.988739952553));
#33864=CARTESIAN_POINT('Ctrl Pts',(-56.3085049635686,-98.2700077840799,
178.797739873155));
#33865=CARTESIAN_POINT('Ctrl Pts',(-55.9449597657812,-98.2759088831958,
178.625214785807));
#33866=CARTESIAN_POINT('Ctrl Pts',(-55.3154969191486,-98.2792776073073,
178.156448816577));
#33867=CARTESIAN_POINT('Ctrl Pts',(-55.052973867085,-98.278484464857,177.868517942429));
#33868=CARTESIAN_POINT('Ctrl Pts',(-54.6434796448366,-98.2603028194195,
177.199076188219));
#33869=CARTESIAN_POINT('Ctrl Pts',(-54.5045782719281,-98.2422508173813,
176.821554461221));
#33870=CARTESIAN_POINT('Ctrl Pts',(-54.3829538671168,-98.1914242422077,
176.047682812831));
#33871=CARTESIAN_POINT('Ctrl Pts',(-54.396798663844,-98.1611041902518,175.659501141255));
#33872=CARTESIAN_POINT('Ctrl Pts',(-54.5719943824211,-98.080673037502,174.898412435821));
#33873=CARTESIAN_POINT('Ctrl Pts',(-54.7363787847236,-98.0302852478859,
174.53405956253));
#33874=CARTESIAN_POINT('Ctrl Pts',(-55.1277451028881,-97.9334031371019,
173.988501298653));
#33875=CARTESIAN_POINT('Ctrl Pts',(-55.3189885889602,-97.8908171156101,
173.788238885403));
#33876=CARTESIAN_POINT('Ctrl Pts',(-55.5345824434661,-97.8467754511356,
173.617797875547));
#33877=CARTESIAN_POINT('Origin',(-54.1598171290174,-67.5719248685924,175.985485069079));
#33878=CARTESIAN_POINT('',(-55.3225704345682,-95.8580444718219,173.617797875548));
#33879=CARTESIAN_POINT('',(-55.3755734367933,-96.3552272166501,173.617797875547));
#33880=CARTESIAN_POINT('',(-52.327900808713,-67.7672193871761,173.617797875548));
#33881=CARTESIAN_POINT('Ctrl Pts',(-55.3225704345676,-95.8580444718219,
173.617797875549));
#33882=CARTESIAN_POINT('Ctrl Pts',(-55.2488731603477,-95.8730994029159,
173.676060379693));
#33883=CARTESIAN_POINT('Ctrl Pts',(-55.1778627825142,-95.8880167521154,
173.737934784587));
#33884=CARTESIAN_POINT('Ctrl Pts',(-54.8249870529423,-95.9643813640093,
174.076580476363));
#33885=CARTESIAN_POINT('Ctrl Pts',(-54.597372284845,-96.0215149400869,174.404859949676));
#33886=CARTESIAN_POINT('Ctrl Pts',(-54.2882731068297,-96.1184723951104,
175.120804814625));
#33887=CARTESIAN_POINT('Ctrl Pts',(-54.2049127919938,-96.1565070312605,
175.499467074234));
#33888=CARTESIAN_POINT('Ctrl Pts',(-54.1850904046615,-96.2200437067127,
176.282494925006));
#33889=CARTESIAN_POINT('Ctrl Pts',(-54.2542224515368,-96.2455419636194,
176.679431477551));
#33890=CARTESIAN_POINT('Ctrl Pts',(-54.5378711477107,-96.2793518199959,
177.411705233674));
#33891=CARTESIAN_POINT('Ctrl Pts',(-54.7446348646939,-96.2865318732696,
177.741846305529));
#33892=CARTESIAN_POINT('Ctrl Pts',(-55.2806673506312,-96.2907393806808,
178.316727233652));
#33893=CARTESIAN_POINT('Ctrl Pts',(-55.6087897538596,-96.2886267840918,
178.552229429508));
#33894=CARTESIAN_POINT('Ctrl Pts',(-56.3250267020568,-96.2763608196003,
178.876240067672));
#33895=CARTESIAN_POINT('Ctrl Pts',(-56.7039131937275,-96.2652663653476,
178.966453550718));
#33896=CARTESIAN_POINT('Ctrl Pts',(-57.4890895773673,-96.2428445615668,
178.999703351349));
#33897=CARTESIAN_POINT('Ctrl Pts',(-57.8881374663501,-96.2331695364305,
178.936986522126));
#33898=CARTESIAN_POINT('Ctrl Pts',(-58.6256832980654,-96.2186706420911,
178.664503387791));
#33899=CARTESIAN_POINT('Ctrl Pts',(-58.9587820211762,-96.2125323238485,
178.462391207497));
#33900=CARTESIAN_POINT('Ctrl Pts',(-59.5415135492665,-96.2116260635046,
177.934371177825));
#33901=CARTESIAN_POINT('Ctrl Pts',(-59.781980393862,-96.2188550670068,177.609532782097));
#33902=CARTESIAN_POINT('Ctrl Pts',(-60.1167365593899,-96.2473328199456,
176.898295990638));
#33903=CARTESIAN_POINT('Ctrl Pts',(-60.2125417189749,-96.2665659682249,
176.521039619842));
#33904=CARTESIAN_POINT('Ctrl Pts',(-60.25823774542,-96.3228473669527,175.737844252544));
#33905=CARTESIAN_POINT('Ctrl Pts',(-60.2023665625948,-96.3616658116569,
175.33923089605));
#33906=CARTESIAN_POINT('Ctrl Pts',(-59.9436358359537,-96.4534477282677,
174.601897903333));
#33907=CARTESIAN_POINT('Ctrl Pts',(-59.7482466819457,-96.5037977056866,
174.268444396503));
#33908=CARTESIAN_POINT('Ctrl Pts',(-59.2337794277028,-96.6197348806844,
173.684665947776));
#33909=CARTESIAN_POINT('Ctrl Pts',(-58.9157588068247,-96.6864976977044,
173.443739655222));
#33910=CARTESIAN_POINT('Ctrl Pts',(-58.217372008235,-96.8251823854556,173.108571771223));
#33911=CARTESIAN_POINT('Ctrl Pts',(-57.8459670981744,-96.8943692598478,
173.012603888321));
#33912=CARTESIAN_POINT('Ctrl Pts',(-57.0735798911608,-97.0377436029253,
172.967475998217));
#33913=CARTESIAN_POINT('Ctrl Pts',(-56.6799835746226,-97.1125605083365,
173.024374207843));
#33914=CARTESIAN_POINT('Ctrl Pts',(-56.0102631250932,-97.2430296646259,
173.265226820711));
#33915=CARTESIAN_POINT('Ctrl Pts',(-55.7309492235603,-97.2986512715054,
173.420654790818));
#33916=CARTESIAN_POINT('Ctrl Pts',(-55.4815794412403,-97.3495927063074,
173.617797875548));
#33917=CARTESIAN_POINT('Ctrl Pts',(-55.5345824434661,-97.8467754511356,
173.617797875547));
#33918=CARTESIAN_POINT('Ctrl Pts',(-55.6169947154963,-97.8299402141496,
173.552645596965));
#33919=CARTESIAN_POINT('Ctrl Pts',(-55.7029083231513,-97.812546688353,173.491868566507));
#33920=CARTESIAN_POINT('Ctrl Pts',(-56.1249583779839,-97.7278219892561,
173.226108125279));
#33921=CARTESIAN_POINT('Ctrl Pts',(-56.4958492165941,-97.6554167225456,
173.085828859448));
#33922=CARTESIAN_POINT('Ctrl Pts',(-57.2577653903279,-97.5102937615483,
172.962314436423));
#33923=CARTESIAN_POINT('Ctrl Pts',(-57.6408149160444,-97.4404766568418,
172.97531750956));
#33924=CARTESIAN_POINT('Ctrl Pts',(-58.3932849875013,-97.2986633757301,
173.150303933633));
#33925=CARTESIAN_POINT('Ctrl Pts',(-58.7541614205803,-97.2273241008258,
173.315593868565));
#33926=CARTESIAN_POINT('Ctrl Pts',(-59.3801444776652,-97.0966437361646,
173.771882659817));
#33927=CARTESIAN_POINT('Ctrl Pts',(-59.6423184034501,-97.0396408082212,
174.054346491916));
#33928=CARTESIAN_POINT('Ctrl Pts',(-60.0527598071511,-96.9343665917044,
174.715910845847));
#33929=CARTESIAN_POINT('Ctrl Pts',(-60.192552060891,-96.8865955714797,175.091374886531));
#33930=CARTESIAN_POINT('Ctrl Pts',(-60.3160027291459,-96.809442177424,175.8635415251));
#33931=CARTESIAN_POINT('Ctrl Pts',(-60.3036791023499,-96.7816290859376,
176.25193825129));
#33932=CARTESIAN_POINT('Ctrl Pts',(-60.1303662911291,-96.7386612800413,
177.017184179734));
#33933=CARTESIAN_POINT('Ctrl Pts',(-59.9658025339903,-96.7233365783403,
177.385464851777));
#33934=CARTESIAN_POINT('Ctrl Pts',(-59.5109353546182,-96.7077917799697,
178.026239753016));
#33935=CARTESIAN_POINT('Ctrl Pts',(-59.2294130920298,-96.7086026675069,
178.295564051087));
#33936=CARTESIAN_POINT('Ctrl Pts',(-58.5686504671049,-96.7176722648981,
178.721086600531));
#33937=CARTESIAN_POINT('Ctrl Pts',(-58.1928009595376,-96.7248726180441,
178.868652601948));
#33938=CARTESIAN_POINT('Ctrl Pts',(-57.4190331249111,-96.743283136341,179.00644614402));
#33939=CARTESIAN_POINT('Ctrl Pts',(-57.0296416326923,-96.7555187290039,
179.00055145821));
#33940=CARTESIAN_POINT('Ctrl Pts',(-56.2604596669238,-96.7762161512854,
178.839419262271));
#33941=CARTESIAN_POINT('Ctrl Pts',(-55.8890973332672,-96.7829392925134,
178.680444217046));
#33942=CARTESIAN_POINT('Ctrl Pts',(-55.2411027402459,-96.7879021772012,
178.234996012765));
#33943=CARTESIAN_POINT('Ctrl Pts',(-54.9678379975261,-96.7876829656282,
177.957218172685));
#33944=CARTESIAN_POINT('Ctrl Pts',(-54.5325795329967,-96.7728490488621,
177.302515713011));
#33945=CARTESIAN_POINT('Ctrl Pts',(-54.3791937444477,-96.7563360778038,
176.928937952964));
#33946=CARTESIAN_POINT('Ctrl Pts',(-54.2291523730752,-96.7081766400537,
176.158344477697));
#33947=CARTESIAN_POINT('Ctrl Pts',(-54.2288040560873,-96.6787881573269,
175.769759226876));
#33948=CARTESIAN_POINT('Ctrl Pts',(-54.3765212283317,-96.6018697724001,
175.001099244294));
#33949=CARTESIAN_POINT('Ctrl Pts',(-54.5283593919543,-96.5528199541182,
174.629581185717));
#33950=CARTESIAN_POINT('Ctrl Pts',(-54.9205751349598,-96.4526499836936,
174.039918340427));
#33951=CARTESIAN_POINT('Ctrl Pts',(-55.1324371633112,-96.4048952658755,
173.810012964794));
#33952=CARTESIAN_POINT('Ctrl Pts',(-55.3755734367937,-96.35522721665,173.617797875547));
#33953=CARTESIAN_POINT('Origin',(-54.1598171290174,-67.5719248685924,175.985485069079));
#33954=CARTESIAN_POINT('',(-55.1635614278963,-94.3664962373362,173.617797875548));
#33955=CARTESIAN_POINT('',(-55.2165644301208,-94.8636789821645,173.617797875548));
#33956=CARTESIAN_POINT('',(-52.327900808713,-67.7672193871761,173.617797875548));
#33957=CARTESIAN_POINT('Ctrl Pts',(-55.163561427896,-94.3664962373362,173.617797875548));
#33958=CARTESIAN_POINT('Ctrl Pts',(-55.056218364382,-94.3884243539691,173.702659571575));
#33959=CARTESIAN_POINT('Ctrl Pts',(-54.9546523839058,-94.4100448203152,
173.795122112537));
#33960=CARTESIAN_POINT('Ctrl Pts',(-54.588095380377,-94.4916767822101,174.17906603512));
#33961=CARTESIAN_POINT('Ctrl Pts',(-54.375501714509,-94.5471774826487,174.515492085468));
#33962=CARTESIAN_POINT('Ctrl Pts',(-54.0968551211791,-94.6404534404216,
175.242776758176));
#33963=CARTESIAN_POINT('Ctrl Pts',(-54.0292270717692,-94.6762889180113,
175.62500182216));
#33964=CARTESIAN_POINT('Ctrl Pts',(-54.0421926615871,-94.7369743988195,
176.407110581385));
#33965=CARTESIAN_POINT('Ctrl Pts',(-54.1271843755252,-94.7607583875431,
176.799360193194));
#33966=CARTESIAN_POINT('Ctrl Pts',(-54.4394251787236,-94.7911050175151,
177.518466198867));
#33967=CARTESIAN_POINT('Ctrl Pts',(-54.6593448976417,-94.7963387031362,
177.84018550867));
#33968=CARTESIAN_POINT('Ctrl Pts',(-55.2172395846646,-94.798844867514,178.392010226581));
#33969=CARTESIAN_POINT('Ctrl Pts',(-55.5530860010683,-94.7958926645089,
178.613444558317));
#33970=CARTESIAN_POINT('Ctrl Pts',(-56.2799683754373,-94.7820964283054,
178.908802794561));
#33971=CARTESIAN_POINT('Ctrl Pts',(-56.662094212939,-94.7700953287221,178.984201982332));
#33972=CARTESIAN_POINT('Ctrl Pts',(-57.4466423122614,-94.7483537445882,
178.986775780572));
#33973=CARTESIAN_POINT('Ctrl Pts',(-57.8414883194669,-94.739117177713,178.909142731616));
#33974=CARTESIAN_POINT('Ctrl Pts',(-58.5669122135515,-94.7255345791514,
178.609761049303));
#33975=CARTESIAN_POINT('Ctrl Pts',(-58.892161692691,-94.7196585115898,178.395302043432));
#33976=CARTESIAN_POINT('Ctrl Pts',(-59.4537702240862,-94.7216002585186,
177.846821950288));
#33977=CARTESIAN_POINT('Ctrl Pts',(-59.6813123838403,-94.730203656332,177.514644370105));
#33978=CARTESIAN_POINT('Ctrl Pts',(-59.989620948833,-94.7611439463418,176.793310965176));
#33979=CARTESIAN_POINT('Ctrl Pts',(-60.0717228469572,-94.7812542368023,
176.412988750328));
#33980=CARTESIAN_POINT('Ctrl Pts',(-60.0892594696137,-94.841115825725,175.630300886533));
#33981=CARTESIAN_POINT('Ctrl Pts',(-60.0196295797508,-94.8814029590579,
175.235471098125));
#33982=CARTESIAN_POINT('Ctrl Pts',(-59.7360736259875,-94.9754930330783,
174.509272205753));
#33983=CARTESIAN_POINT('Ctrl Pts',(-59.5292974353456,-95.0264678405705,
174.183050393779));
#33984=CARTESIAN_POINT('Ctrl Pts',(-58.9960460002618,-95.1449670913247,
173.618822843707));
#33985=CARTESIAN_POINT('Ctrl Pts',(-58.6711941602365,-95.2124648371533,
173.389819924504));
#33986=CARTESIAN_POINT('Ctrl Pts',(-57.9634202187307,-95.3518299433625,
173.079094406885));
#33987=CARTESIAN_POINT('Ctrl Pts',(-57.5891546966644,-95.4207308213124,
172.99574207915));
#33988=CARTESIAN_POINT('Ctrl Pts',(-56.8171726429903,-95.5646023159323,
172.976684919917));
#33989=CARTESIAN_POINT('Ctrl Pts',(-56.4269278469765,-95.6390727589893,
173.046323931544));
#33990=CARTESIAN_POINT('Ctrl Pts',(-55.7957642864128,-95.7625431312478,
173.296634934914));
#33991=CARTESIAN_POINT('Ctrl Pts',(-55.5469343965475,-95.8122112436145,
173.44042352347));
#33992=CARTESIAN_POINT('Ctrl Pts',(-55.3225704345677,-95.8580444718219,
173.617797875549));
#33993=CARTESIAN_POINT('Ctrl Pts',(-55.3755734367937,-96.35522721665,173.617797875547));
#33994=CARTESIAN_POINT('Ctrl Pts',(-55.4307651910792,-96.3439526062045,
173.574165192428));
#33995=CARTESIAN_POINT('Ctrl Pts',(-55.4875430741737,-96.3324243840167,
173.532482528561));
#33996=CARTESIAN_POINT('Ctrl Pts',(-55.8724009271436,-96.2547381147215,
173.270675811687));
#33997=CARTESIAN_POINT('Ctrl Pts',(-56.2395551487011,-96.182736586261,173.116986678507));
#33998=CARTESIAN_POINT('Ctrl Pts',(-56.9983211435042,-96.0376240798129,
172.967152893997));
#33999=CARTESIAN_POINT('Ctrl Pts',(-57.3816828039697,-95.9671829248927,
172.967075834089));
#34000=CARTESIAN_POINT('Ctrl Pts',(-58.1410184669512,-95.8251835602254,
173.116566059386));
#34001=CARTESIAN_POINT('Ctrl Pts',(-58.5083499151732,-95.753165851405,173.270197441364));
#34002=CARTESIAN_POINT('Ctrl Pts',(-59.1498803587327,-95.6205203225493,
173.70650315128));
#34003=CARTESIAN_POINT('Ctrl Pts',(-59.4210480577474,-95.5619683302694,
173.980372408889));
#34004=CARTESIAN_POINT('Ctrl Pts',(-59.8532696072757,-95.4548985128898,
174.629277399653));
#34005=CARTESIAN_POINT('Ctrl Pts',(-60.0052557757833,-95.4058409991536,
175.001197164812));
#34006=CARTESIAN_POINT('Ctrl Pts',(-60.1526461672196,-95.3258448395883,
175.770400507816));
#34007=CARTESIAN_POINT('Ctrl Pts',(-60.1521527002433,-95.2961838508183,
176.159145644728));
#34008=CARTESIAN_POINT('Ctrl Pts',(-60.0020756560049,-95.25124541977,176.930549171593));
#34009=CARTESIAN_POINT('Ctrl Pts',(-59.8481492936629,-95.2348033599355,
177.304675965347));
#34010=CARTESIAN_POINT('Ctrl Pts',(-59.4114542618371,-95.2170471154485,
177.959694992412));
#34011=CARTESIAN_POINT('Ctrl Pts',(-59.1376578950276,-95.2164539288486,
178.237323092304));
#34012=CARTESIAN_POINT('Ctrl Pts',(-58.4884866437325,-95.2247742367641,
178.682694049653));
#34013=CARTESIAN_POINT('Ctrl Pts',(-58.115931013141,-95.2316427901242,178.841401776965));
#34014=CARTESIAN_POINT('Ctrl Pts',(-57.3448951470266,-95.2495037021288,
179.001135652719));
#34015=CARTESIAN_POINT('Ctrl Pts',(-56.955125254993,-95.2612079064579,179.00610941923));
#34016=CARTESIAN_POINT('Ctrl Pts',(-56.1805126479013,-95.2829505974448,
178.866164044176));
#34017=CARTESIAN_POINT('Ctrl Pts',(-55.803943202269,-95.290250419438,178.716937553678));
#34018=CARTESIAN_POINT('Ctrl Pts',(-55.1431193746723,-95.2963377805561,
178.288149902574));
#34019=CARTESIAN_POINT('Ctrl Pts',(-54.8623109504861,-95.296361893453,178.017466611653));
#34020=CARTESIAN_POINT('Ctrl Pts',(-54.4092692797554,-95.2838700527111,
177.373334850441));
#34021=CARTESIAN_POINT('Ctrl Pts',(-54.2458760236569,-95.2684472974855,
177.002822289733));
#34022=CARTESIAN_POINT('Ctrl Pts',(-54.0760681605979,-95.2221663811948,
176.234803937473));
#34023=CARTESIAN_POINT('Ctrl Pts',(-54.0658951530641,-95.1932770792832,
175.845926949155));
#34024=CARTESIAN_POINT('Ctrl Pts',(-54.1946194628085,-95.1188098143918,
175.072356420616));
#34025=CARTESIAN_POINT('Ctrl Pts',(-54.3376779401713,-95.0707207130394,
174.696164868778));
#34026=CARTESIAN_POINT('Ctrl Pts',(-54.7289680209749,-94.9684859243212,
174.075800391413));
#34027=CARTESIAN_POINT('Ctrl Pts',(-54.9544853247051,-94.9172166864417,
173.82498850949));
#34028=CARTESIAN_POINT('Ctrl Pts',(-55.216564430121,-94.8636789821645,173.617797875547));
#34029=CARTESIAN_POINT('Origin',(-54.1598171290174,-67.5719248685924,175.985485069079));
#34030=CARTESIAN_POINT('',(-55.0045524212243,-92.8749480028505,173.617797875548));
#34031=CARTESIAN_POINT('',(-55.0575554234485,-93.372130747679,173.617797875548));
#34032=CARTESIAN_POINT('',(-52.327900808713,-67.7672193871761,173.617797875548));
#34033=CARTESIAN_POINT('Ctrl Pts',(-55.0045524212243,-92.8749480028505,
173.617797875548));
#34034=CARTESIAN_POINT('Ctrl Pts',(-54.8569032582738,-92.9051098778702,
173.734524173221));
#34035=CARTESIAN_POINT('Ctrl Pts',(-54.7203662707415,-92.9346522820336,
173.865484200462));
#34036=CARTESIAN_POINT('Ctrl Pts',(-54.3417383663621,-93.0221247962368,
174.306035059822));
#34037=CARTESIAN_POINT('Ctrl Pts',(-54.1474550333502,-93.0755584336755,
174.651322880573));
#34038=CARTESIAN_POINT('Ctrl Pts',(-53.9054598013013,-93.1643391309631,
175.391357838398));
#34039=CARTESIAN_POINT('Ctrl Pts',(-53.8569545310989,-93.1979466769663,
175.777944186085));
#34040=CARTESIAN_POINT('Ctrl Pts',(-53.9097491119168,-93.2550918971405,
176.557964426028));
#34041=CARTESIAN_POINT('Ctrl Pts',(-54.0136985785005,-93.2767515783228,
176.94366000401));
#34042=CARTESIAN_POINT('Ctrl Pts',(-54.3603654084999,-93.3028574026009,
177.646013455223));
#34043=CARTESIAN_POINT('Ctrl Pts',(-54.5965912360363,-93.3061079766006,
177.957369754161));
#34044=CARTESIAN_POINT('Ctrl Pts',(-55.1808634586347,-93.3065067763144,
178.480019859168));
#34045=CARTESIAN_POINT('Ctrl Pts',(-55.5254726227184,-93.3025286745695,
178.683672507102));
#34046=CARTESIAN_POINT('Ctrl Pts',(-56.2647985713167,-93.2868531592762,
178.943290967325));
#34047=CARTESIAN_POINT('Ctrl Pts',(-56.651071733831,-93.2741130933769,179.000096571975));
#34048=CARTESIAN_POINT('Ctrl Pts',(-57.4339392821045,-93.2532521783921,
178.964063884305));
#34049=CARTESIAN_POINT('Ctrl Pts',(-57.8227022361252,-93.2445836133361,
178.867925910384));
#34050=CARTESIAN_POINT('Ctrl Pts',(-58.5321780022402,-93.2321672139304,
178.534974955654));
#34051=CARTESIAN_POINT('Ctrl Pts',(-58.8474774466859,-93.2270067601978,
178.304732794236));
#34052=CARTESIAN_POINT('Ctrl Pts',(-59.3814483982118,-93.2325912463974,
177.730658867794));
#34053=CARTESIAN_POINT('Ctrl Pts',(-59.5920834337611,-93.242927406223,177.389796722879));
#34054=CARTESIAN_POINT('Ctrl Pts',(-59.8662607427621,-93.2769916073557,
176.656193721462));
#34055=CARTESIAN_POINT('Ctrl Pts',(-59.9306275100233,-93.2986032359834,
176.271859584237));
#34056=CARTESIAN_POINT('Ctrl Pts',(-59.911513575484,-93.3630613791081,175.490628628338));
#34057=CARTESIAN_POINT('Ctrl Pts',(-59.8242017213171,-93.4051742501552,
175.101439271628));
#34058=CARTESIAN_POINT('Ctrl Pts',(-59.5085893254885,-93.5021867078949,
174.390349822164));
#34059=CARTESIAN_POINT('Ctrl Pts',(-59.2868218922751,-93.554330421169,174.073633436082));
#34060=CARTESIAN_POINT('Ctrl Pts',(-58.7292535184541,-93.6761025352044,
173.535787883294));
#34061=CARTESIAN_POINT('Ctrl Pts',(-58.3959881887055,-93.7444477798263,
173.322880107027));
#34062=CARTESIAN_POINT('Ctrl Pts',(-57.6763776517792,-93.8845996153561,
173.044716985648));
#34063=CARTESIAN_POINT('Ctrl Pts',(-57.2982879865103,-93.9534434547723,
172.978244121145));
#34064=CARTESIAN_POINT('Ctrl Pts',(-56.5275433446037,-94.097852994184,172.994197789256));
#34065=CARTESIAN_POINT('Ctrl Pts',(-56.1424275208482,-94.1717364822287,
173.080752024789));
#34066=CARTESIAN_POINT('Ctrl Pts',(-55.5630058610648,-94.2857381652413,
173.340270659517));
#34067=CARTESIAN_POINT('Ctrl Pts',(-55.3543190155038,-94.3275281429596,
173.466991555285));
#34068=CARTESIAN_POINT('Ctrl Pts',(-55.163561427896,-94.3664962373362,173.617797875548));
#34069=CARTESIAN_POINT('Ctrl Pts',(-55.216564430121,-94.8636789821645,173.617797875547));
#34070=CARTESIAN_POINT('Ctrl Pts',(-55.2532799768635,-94.8561787044115,
173.588771840095));
#34071=CARTESIAN_POINT('Ctrl Pts',(-55.2907018285174,-94.8485652993067,
173.560605332552));
#34072=CARTESIAN_POINT('Ctrl Pts',(-55.6508164104634,-94.775591169922,173.302776237068));
#34073=CARTESIAN_POINT('Ctrl Pts',(-56.0151735547999,-94.7039136072724,
173.140038565322));
#34074=CARTESIAN_POINT('Ctrl Pts',(-56.7715612575832,-94.5588528925702,
172.97233220456));
#34075=CARTESIAN_POINT('Ctrl Pts',(-57.1551311161026,-94.4878711261834,
172.963423206831));
#34076=CARTESIAN_POINT('Ctrl Pts',(-57.918841782984,-94.3457926735877,173.095700543124));
#34077=CARTESIAN_POINT('Ctrl Pts',(-58.2903049931619,-94.2733609867026,
173.241373548713));
#34078=CARTESIAN_POINT('Ctrl Pts',(-58.9421223829594,-94.1394295431226,
173.664106773207));
#34079=CARTESIAN_POINT('Ctrl Pts',(-59.2192919982907,-94.0797358692806,
173.932241960795));
#34080=CARTESIAN_POINT('Ctrl Pts',(-59.6658914264387,-93.9715016179453,
174.572526583826));
#34081=CARTESIAN_POINT('Ctrl Pts',(-59.8259305467065,-93.9216125355567,
174.941878357353));
#34082=CARTESIAN_POINT('Ctrl Pts',(-59.9892246444878,-93.8397435228945,
175.708915779253));
#34083=CARTESIAN_POINT('Ctrl Pts',(-59.9965407460571,-93.8087655348136,
176.097899047269));
#34084=CARTESIAN_POINT('Ctrl Pts',(-59.8618177030415,-93.7625400837011,
176.873158317106));
#34085=CARTESIAN_POINT('Ctrl Pts',(-59.7149900573912,-93.7453683695564,
177.250961385648));
#34086=CARTESIAN_POINT('Ctrl Pts',(-59.2903691729418,-93.7261587425722,
177.915219986264));
#34087=CARTESIAN_POINT('Ctrl Pts',(-59.0216153581125,-93.7245615280262,
178.198287673508));
#34088=CARTESIAN_POINT('Ctrl Pts',(-58.3801618852297,-93.7323908620532,
178.656507648529));
#34089=CARTESIAN_POINT('Ctrl Pts',(-58.0099231073576,-93.7390395105877,
178.822428560122));
#34090=CARTESIAN_POINT('Ctrl Pts',(-57.2408258148254,-93.7565381598963,
178.996447660266));
#34091=CARTESIAN_POINT('Ctrl Pts',(-56.8507964687961,-93.7678219607524,
179.008467958561));
#34092=CARTESIAN_POINT('Ctrl Pts',(-56.0728355882105,-93.7902359073096,
178.882250596652));
#34093=CARTESIAN_POINT('Ctrl Pts',(-55.6930426259906,-93.7979062500858,
178.739394748503));
#34094=CARTESIAN_POINT('Ctrl Pts',(-55.0240443173154,-93.8047194732275,
178.321455511669));
#34095=CARTESIAN_POINT('Ctrl Pts',(-54.7383776431007,-93.8048320736551,
178.055327229978));
#34096=CARTESIAN_POINT('Ctrl Pts',(-54.2740247564696,-93.7938434797566,
177.418090509773));
#34097=CARTESIAN_POINT('Ctrl Pts',(-54.1042673274708,-93.779125687626,177.049674695849));
#34098=CARTESIAN_POINT('Ctrl Pts',(-53.9218210197265,-93.734055954135,176.283430443779));
#34099=CARTESIAN_POINT('Ctrl Pts',(-53.9053820092821,-93.7054239240535,
175.894363042321));
#34100=CARTESIAN_POINT('Ctrl Pts',(-54.0220154697562,-93.6325267082092,
175.117801278641));
#34101=CARTESIAN_POINT('Ctrl Pts',(-54.1594435951317,-93.5850638346546,
174.738753876289));
#34102=CARTESIAN_POINT('Ctrl Pts',(-54.5495048403043,-93.4816043007811,
174.09877951738));
#34103=CARTESIAN_POINT('Ctrl Pts',(-54.7834613811529,-93.4281228717259,
173.834487101089));
#34104=CARTESIAN_POINT('Ctrl Pts',(-55.0575554234485,-93.372130747679,173.617797875548));
#34105=CARTESIAN_POINT('Origin',(-54.1598171290174,-67.5719248685924,175.985485069079));
#34106=CARTESIAN_POINT('',(-54.8455434145523,-91.3833997683648,173.617797875548));
#34107=CARTESIAN_POINT('',(-54.8985464167762,-91.8805825131934,173.617797875548));
#34108=CARTESIAN_POINT('',(-52.327900808713,-67.7672193871761,173.617797875548));
#34109=CARTESIAN_POINT('Ctrl Pts',(-54.8455434145526,-91.3833997683648,
173.617797875547));
#34110=CARTESIAN_POINT('Ctrl Pts',(-54.6565253335548,-91.4220125151056,
173.76722900233));
#34111=CARTESIAN_POINT('Ctrl Pts',(-54.4860219465301,-91.4595477719293,
173.939743355083));
#34112=CARTESIAN_POINT('Ctrl Pts',(-54.1001265638809,-91.5524166507176,
174.440593638359));
#34113=CARTESIAN_POINT('Ctrl Pts',(-53.9249220525858,-91.6036119642123,
174.79393662834));
#34114=CARTESIAN_POINT('Ctrl Pts',(-53.7207399973051,-91.6876830864498,
175.546124447473));
#34115=CARTESIAN_POINT('Ctrl Pts',(-53.6922572054311,-91.7194669392612,
175.937272343594));
#34116=CARTESIAN_POINT('Ctrl Pts',(-53.7865525319358,-91.7728324375254,
176.713966170903));
#34117=CARTESIAN_POINT('Ctrl Pts',(-53.9098262191694,-91.7922372835231,
177.091848532611));
#34118=CARTESIAN_POINT('Ctrl Pts',(-54.292013977408,-91.8138836063467,177.775855580414));
#34119=CARTESIAN_POINT('Ctrl Pts',(-54.5456631560371,-91.8155251406082,
178.076189528251));
#34120=CARTESIAN_POINT('Ctrl Pts',(-55.1571631643673,-91.8136797426504,
178.567013800483));
#34121=CARTESIAN_POINT('Ctrl Pts',(-55.5100946048466,-91.808629984099,178.751362100129));
#34122=CARTESIAN_POINT('Ctrl Pts',(-56.2617722088354,-91.7909724493156,
178.972609206582));
#34123=CARTESIAN_POINT('Ctrl Pts',(-56.6526203471813,-91.7779293408117,
179.009236096806));
#34124=CARTESIAN_POINT('Ctrl Pts',(-57.4325276120376,-91.758054815642,178.93134134647));
#34125=CARTESIAN_POINT('Ctrl Pts',(-57.813712217306,-91.7500205513923,178.815543006379));
#34126=CARTESIAN_POINT('Ctrl Pts',(-58.5050152274851,-91.7388854271101,
178.446542967835));
#34127=CARTESIAN_POINT('Ctrl Pts',(-58.8093801021319,-91.7350109740523,
178.198823734832));
#34128=CARTESIAN_POINT('Ctrl Pts',(-59.3119933624224,-91.7446198199896,
177.597240068657));
#34129=CARTESIAN_POINT('Ctrl Pts',(-59.5035171706838,-91.7568310469166,
177.24773698331));
#34130=CARTESIAN_POINT('Ctrl Pts',(-59.7395806933547,-91.7943131744684,
176.501424313155));
#34131=CARTESIAN_POINT('Ctrl Pts',(-59.7840082400886,-91.8181063823523,
176.112536338177));
#34132=CARTESIAN_POINT('Ctrl Pts',(-59.7235636554942,-91.8876608546724,
175.334046855008));
#34133=CARTESIAN_POINT('Ctrl Pts',(-59.6166815717699,-91.9317093374407,
174.952172532456));
#34134=CARTESIAN_POINT('Ctrl Pts',(-59.2652605338654,-92.0319062920826,
174.258968497943));
#34135=CARTESIAN_POINT('Ctrl Pts',(-59.0263023246206,-92.08587485512,173.953143163745));
#34136=CARTESIAN_POINT('Ctrl Pts',(-58.4415336682585,-92.2112437707519,
173.446376314883));
#34137=CARTESIAN_POINT('Ctrl Pts',(-58.0995025750682,-92.2803846238087,
173.252374409362));
#34138=CARTESIAN_POINT('Ctrl Pts',(-57.3671026897501,-92.4212806505717,
173.011983670517));
#34139=CARTESIAN_POINT('Ctrl Pts',(-56.9845499457477,-92.4905300386684,
172.96525589994));
#34140=CARTESIAN_POINT('Ctrl Pts',(-56.216284091542,-92.635377266259,173.022212362854));
#34141=CARTESIAN_POINT('Ctrl Pts',(-55.8380764927768,-92.7083973345374,
173.128234533467));
#34142=CARTESIAN_POINT('Ctrl Pts',(-55.3188346949646,-92.8112758246322,
173.393439625609));
#34143=CARTESIAN_POINT('Ctrl Pts',(-55.1559496924782,-92.8440204616262,
173.49810845369));
#34144=CARTESIAN_POINT('Ctrl Pts',(-55.0045524212243,-92.8749480028505,
173.617797875548));
#34145=CARTESIAN_POINT('Ctrl Pts',(-55.0575554234485,-93.372130747679,173.617797875548));
#34146=CARTESIAN_POINT('Ctrl Pts',(-55.0826501717059,-93.3670043748268,
173.597958839575));
#34147=CARTESIAN_POINT('Ctrl Pts',(-55.1080760854621,-93.3618249067256,
173.57852039083));
#34148=CARTESIAN_POINT('Ctrl Pts',(-55.4528584352249,-93.2917830015913,
173.323717361705));
#34149=CARTESIAN_POINT('Ctrl Pts',(-55.8153492922638,-93.22032977783,173.155314509966));
#34150=CARTESIAN_POINT('Ctrl Pts',(-56.5701409630624,-93.0753202870361,
172.976363563093));
#34151=CARTESIAN_POINT('Ctrl Pts',(-56.9538396838264,-93.0039511914057,
172.961915225107));
#34152=CARTESIAN_POINT('Ctrl Pts',(-57.7201870735368,-92.8618419731353,
173.083405439403));
#34153=CARTESIAN_POINT('Ctrl Pts',(-58.0941464128959,-92.7891688593354,
173.224058494334));
#34154=CARTESIAN_POINT('Ctrl Pts',(-58.7523253532587,-92.6544481586586,
173.638252468771));
#34155=CARTESIAN_POINT('Ctrl Pts',(-59.0332297739802,-92.5940009461163,
173.902819260972));
#34156=CARTESIAN_POINT('Ctrl Pts',(-59.4887090310732,-92.4850559455269,
174.537673954038));
#34157=CARTESIAN_POINT('Ctrl Pts',(-59.6537202371819,-92.4346607096272,
174.905348495639));
#34158=CARTESIAN_POINT('Ctrl Pts',(-59.8268767927802,-92.3516365901475,
175.670963162657));
#34159=CARTESIAN_POINT('Ctrl Pts',(-59.8390186337771,-92.3198066129628,
176.060096237857));
#34160=CARTESIAN_POINT('Ctrl Pts',(-59.7137837922629,-92.2727917671927,
176.837654715681));
#34161=CARTESIAN_POINT('Ctrl Pts',(-59.5713681586131,-92.2551727805481,
177.217655119944));
#34162=CARTESIAN_POINT('Ctrl Pts',(-59.1542349634437,-92.2350681269231,
177.887555270179));
#34163=CARTESIAN_POINT('Ctrl Pts',(-58.8885745411324,-92.2328210251685,
178.17396692491));
#34164=CARTESIAN_POINT('Ctrl Pts',(-58.2519116722656,-92.2403486057468,
178.640023495696));
#34165=CARTESIAN_POINT('Ctrl Pts',(-57.8831575336419,-92.246861193658,178.810341960741));
#34166=CARTESIAN_POINT('Ctrl Pts',(-57.1153094579654,-92.2641363601497,
178.993105557227));
#34167=CARTESIAN_POINT('Ctrl Pts',(-56.7251166733867,-92.2751344100561,
179.009429420874));
#34168=CARTESIAN_POINT('Ctrl Pts',(-55.9451775899093,-92.2979556768727,
178.891589253066));
#34169=CARTESIAN_POINT('Ctrl Pts',(-55.5634757749293,-92.3058508359901,
178.752640123539));
#34170=CARTESIAN_POINT('Ctrl Pts',(-54.8895422164754,-92.3131059527131,
178.34134143223));
#34171=CARTESIAN_POINT('Ctrl Pts',(-54.600921528257,-92.3132467009483,178.077978006958));
#34172=CARTESIAN_POINT('Ctrl Pts',(-54.129746242459,-92.3031699421057,177.444965202739));
#34173=CARTESIAN_POINT('Ctrl Pts',(-53.95615204043,-92.2888815881815,177.077869618163));
#34174=CARTESIAN_POINT('Ctrl Pts',(-53.7660578707382,-92.2445486141228,
176.312747534025));
#34175=CARTESIAN_POINT('Ctrl Pts',(-53.7458319553549,-92.2160493616996,
175.923563743096));
#34176=CARTESIAN_POINT('Ctrl Pts',(-53.8551691600749,-92.1441031926879,
175.145247067551));
#34177=CARTESIAN_POINT('Ctrl Pts',(-53.9891852928614,-92.0970235596548,
174.764521270207));
#34178=CARTESIAN_POINT('Ctrl Pts',(-54.3782657801789,-91.9928589589126,
174.112695179671));
#34179=CARTESIAN_POINT('Ctrl Pts',(-54.6172195876594,-91.9380521560273,
173.840205091023));
#34180=CARTESIAN_POINT('Ctrl Pts',(-54.8985464167762,-91.8805825131934,
173.617797875548));
#34181=CARTESIAN_POINT('Origin',(-54.1598171290174,-67.5719248685924,175.985485069079));
#34182=CARTESIAN_POINT('',(-54.6865344078804,-89.8918515338791,173.617797875547));
#34183=CARTESIAN_POINT('',(-54.739537410104,-90.3890342787078,173.617797875548));
#34184=CARTESIAN_POINT('',(-52.327900808713,-67.7672193871761,173.617797875548));
#34185=CARTESIAN_POINT('Ctrl Pts',(-54.686534407881,-89.891851533879,173.617797875547));
#34186=CARTESIAN_POINT('Ctrl Pts',(-54.4633167153865,-89.9374506013485,
173.794266026801));
#34187=CARTESIAN_POINT('Ctrl Pts',(-54.2662753749012,-89.9814742982852,
174.002644386251));
#34188=CARTESIAN_POINT('Ctrl Pts',(-53.8744147557856,-90.0792998157546,
174.560342096286));
#34189=CARTESIAN_POINT('Ctrl Pts',(-53.7134765841226,-90.1293243049206,
174.926721926365));
#34190=CARTESIAN_POINT('Ctrl Pts',(-53.5458718952793,-90.2087890541603,
175.689958129594));
#34191=CARTESIAN_POINT('Ctrl Pts',(-53.5359469632516,-90.2388267308604,
176.078248986262));
#34192=CARTESIAN_POINT('Ctrl Pts',(-53.6654007924014,-90.2889223883734,
176.851267187356));
#34193=CARTESIAN_POINT('Ctrl Pts',(-53.8083029365153,-90.3065538368161,
177.22775708202));
#34194=CARTESIAN_POINT('Ctrl Pts',(-54.2249191190689,-90.3238154041645,
177.893191928766));
#34195=CARTESIAN_POINT('Ctrl Pts',(-54.4903906452805,-90.3244240736402,
178.178329691486));
#34196=CARTESIAN_POINT('Ctrl Pts',(-55.1249692417654,-90.3206187220871,
178.64074427075));
#34197=CARTESIAN_POINT('Ctrl Pts',(-55.4907054350572,-90.3144920361692,
178.809591114113));
#34198=CARTESIAN_POINT('Ctrl Pts',(-56.2539859372547,-90.2948774807113,
178.992430457108));
#34199=CARTESIAN_POINT('Ctrl Pts',(-56.6430191620045,-90.2822463249235,
179.009465058108));
#34200=CARTESIAN_POINT('Ctrl Pts',(-57.4192658904802,-90.2632843494434,
178.894021241466));
#34201=CARTESIAN_POINT('Ctrl Pts',(-57.7981378905664,-90.2557537741638,
178.757871111041));
#34202=CARTESIAN_POINT('Ctrl Pts',(-58.4703801255018,-90.2459268970991,
178.352709714571));
#34203=CARTESIAN_POINT('Ctrl Pts',(-58.759760035485,-90.2438552899847,178.091790194712));
#34204=CARTESIAN_POINT('Ctrl Pts',(-59.2326888009695,-90.2571726407939,
177.465587105964));
#34205=CARTESIAN_POINT('Ctrl Pts',(-59.4077546669428,-90.2713645633644,
177.103495021403));
#34206=CARTESIAN_POINT('Ctrl Pts',(-59.6043161995092,-90.3123324179346,
176.344807191295));
#34207=CARTESIAN_POINT('Ctrl Pts',(-59.6285073907552,-90.3384712918412,
175.956743027903));
#34208=CARTESIAN_POINT('Ctrl Pts',(-59.5288616190547,-90.4127699722497,
175.181982068486));
#34209=CARTESIAN_POINT('Ctrl Pts',(-59.4012644009517,-90.4592220492257,
174.803380814995));
#34210=CARTESIAN_POINT('Ctrl Pts',(-59.0126446018412,-90.5626595348428,
174.12960818678));
#34211=CARTESIAN_POINT('Ctrl Pts',(-58.7593768324647,-90.6183213238378,
173.838628285224));
#34212=CARTESIAN_POINT('Ctrl Pts',(-58.1489228992904,-90.7470140885838,
173.362985019365));
#34213=CARTESIAN_POINT('Ctrl Pts',(-57.794726357837,-90.8176161826738,173.18648906466));
#34214=CARTESIAN_POINT('Ctrl Pts',(-57.049407235224,-90.9591667760492,172.986630995271));
#34215=CARTESIAN_POINT('Ctrl Pts',(-56.6666652198049,-91.0285802500661,
172.960849429604));
#34216=CARTESIAN_POINT('Ctrl Pts',(-55.9061538922212,-91.172868747317,173.058338296301));
#34217=CARTESIAN_POINT('Ctrl Pts',(-55.5358170768977,-91.2448364349498,
173.183416544522));
#34218=CARTESIAN_POINT('Ctrl Pts',(-55.0759192312235,-91.3366282705884,
173.448860726571));
#34219=CARTESIAN_POINT('Ctrl Pts',(-54.9575343983508,-91.3605221713019,
173.529261695251));
#34220=CARTESIAN_POINT('Ctrl Pts',(-54.8455434145526,-91.3833997683648,
173.617797875547));
#34221=CARTESIAN_POINT('Ctrl Pts',(-54.8985464167762,-91.8805825131934,
173.617797875548));
#34222=CARTESIAN_POINT('Ctrl Pts',(-54.9166810916879,-91.8768779490274,
173.603461231711));
#34223=CARTESIAN_POINT('Ctrl Pts',(-54.9349890694865,-91.8731455836112,
173.589333497864));
#34224=CARTESIAN_POINT('Ctrl Pts',(-55.2706786758864,-91.8048472129455,
173.336533768563));
#34225=CARTESIAN_POINT('Ctrl Pts',(-55.6320124378843,-91.7335359313884,
173.164748325449));
#34226=CARTESIAN_POINT('Ctrl Pts',(-56.3858109203006,-91.5885640570063,
172.979061269994));
#34227=CARTESIAN_POINT('Ctrl Pts',(-56.7695858610019,-91.5169457857638,
172.961300143484));
#34228=CARTESIAN_POINT('Ctrl Pts',(-57.5374706866368,-91.374825024809,173.076344111801));
#34229=CARTESIAN_POINT('Ctrl Pts',(-57.9128873597064,-91.3020142352857,
173.2139861571));
#34230=CARTESIAN_POINT('Ctrl Pts',(-58.5748367120917,-91.1668279668907,
173.623064850725));
#34231=CARTESIAN_POINT('Ctrl Pts',(-58.857963704019,-91.1059167792226,173.885507747618));
#34232=CARTESIAN_POINT('Ctrl Pts',(-59.3187021614947,-90.9965538807659,
174.517108019837));
#34233=CARTESIAN_POINT('Ctrl Pts',(-59.4866569982001,-90.9458616320282,
174.883756248298));
#34234=CARTESIAN_POINT('Ctrl Pts',(-59.6656693259464,-90.8621539735064,
175.648497203549));
#34235=CARTESIAN_POINT('Ctrl Pts',(-59.6806707514033,-90.8298055031703,
176.037719840239));
#34236=CARTESIAN_POINT('Ctrl Pts',(-59.5610573016957,-90.7823250908908,
176.816610699042));
#34237=CARTESIAN_POINT('Ctrl Pts',(-59.421264166161,-90.764442457344,177.19788608769));
#34238=CARTESIAN_POINT('Ctrl Pts',(-59.0085766208076,-90.7438086481022,
177.871104180369));
#34239=CARTESIAN_POINT('Ctrl Pts',(-58.7447412256737,-90.7411661130838,
178.159490981354));
#34240=CARTESIAN_POINT('Ctrl Pts',(-58.1109238709733,-90.7485155107734,
178.630153630412));
#34241=CARTESIAN_POINT('Ctrl Pts',(-57.7430677366468,-90.7549474481067,
178.803055769306));
#34242=CARTESIAN_POINT('Ctrl Pts',(-56.9759778588354,-90.7720903515221,
178.990970442362));
#34243=CARTESIAN_POINT('Ctrl Pts',(-56.5856872827903,-90.7829101058451,
179.009826258095));
#34244=CARTESIAN_POINT('Ctrl Pts',(-55.8046079374573,-90.8059700487964,
178.896911433344));
#34245=CARTESIAN_POINT('Ctrl Pts',(-55.4218044306841,-90.8139969176569,
178.760265658305));
#34246=CARTESIAN_POINT('Ctrl Pts',(-54.7449879083774,-90.8215114762877,
178.352878528531));
#34247=CARTESIAN_POINT('Ctrl Pts',(-54.4546340104405,-90.8216598206604,
178.091135798334));
#34248=CARTESIAN_POINT('Ctrl Pts',(-53.9794754661803,-90.8121172399509,
177.460611953341));
#34249=CARTESIAN_POINT('Ctrl Pts',(-53.8036420816968,-90.7980810670428,
177.094306568579));
#34250=CARTESIAN_POINT('Ctrl Pts',(-53.6090739848902,-90.7541804381832,
176.329858004511));
#34251=CARTESIAN_POINT('Ctrl Pts',(-53.5866342074026,-90.7257509734569,
175.940605797033));
#34252=CARTESIAN_POINT('Ctrl Pts',(-53.6917102782147,-90.6543614750933,
175.161281567195));
#34253=CARTESIAN_POINT('Ctrl Pts',(-53.8237290083727,-90.6075074843315,
174.779591227941));
#34254=CARTESIAN_POINT('Ctrl Pts',(-54.2121538026836,-90.5029429956027,
174.120838580762));
#34255=CARTESIAN_POINT('Ctrl Pts',(-54.4539929001211,-90.4473655123602,
173.843539442958));
#34256=CARTESIAN_POINT('Ctrl Pts',(-54.7395374101039,-90.3890342787078,
173.617797875548));
#34257=CARTESIAN_POINT('Origin',(-54.1598171290174,-67.5719248685924,175.985485069079));
#34258=CARTESIAN_POINT('',(-54.527525401208,-88.4003032993935,173.617797875547));
#34259=CARTESIAN_POINT('',(-54.5805284034317,-88.8974860442222,173.617797875548));
#34260=CARTESIAN_POINT('',(-52.327900808713,-67.7672193871761,173.617797875548));
#34261=CARTESIAN_POINT('Ctrl Pts',(-54.5275254012084,-88.4003032993935,
173.617797875547));
#34262=CARTESIAN_POINT('Ctrl Pts',(-54.278959213732,-88.4510805752748,173.814305666117));
#34263=CARTESIAN_POINT('Ctrl Pts',(-54.0631391385075,-88.4998460783872,
174.050160506599));
#34264=CARTESIAN_POINT('Ctrl Pts',(-53.6710624598621,-88.6006245172416,
174.648595393675));
#34265=CARTESIAN_POINT('Ctrl Pts',(-53.5217286468206,-88.6494022957689,
175.021474411702));
#34266=CARTESIAN_POINT('Ctrl Pts',(-53.3794474284676,-88.7256210554948,
175.791566490734));
#34267=CARTESIAN_POINT('Ctrl Pts',(-53.3826058558834,-88.7548547030929,
176.180234237913));
#34268=CARTESIAN_POINT('Ctrl Pts',(-53.5382939506053,-88.8024794567196,
176.950116833368));
#34269=CARTESIAN_POINT('Ctrl Pts',(-53.694544846128,-88.8186825700164,177.322845741933));
#34270=CARTESIAN_POINT('Ctrl Pts',(-54.1348950035689,-88.8328485434147,
177.974555021883));
#34271=CARTESIAN_POINT('Ctrl Pts',(-54.4103082949843,-88.8329851822358,
178.250309372985));
#34272=CARTESIAN_POINT('Ctrl Pts',(-55.0619731676736,-88.8277023916178,
178.691035708699));
#34273=CARTESIAN_POINT('Ctrl Pts',(-55.4348430505563,-88.8208148853015,
178.847252783794));
#34274=CARTESIAN_POINT('Ctrl Pts',(-56.2056002236782,-88.7998194230701,
179.002367411531));
#34275=CARTESIAN_POINT('Ctrl Pts',(-56.595096367605,-88.7877202098109,179.005175375157));
#34276=CARTESIAN_POINT('Ctrl Pts',(-57.3681199604207,-88.7694646375483,
178.861163165126));
#34277=CARTESIAN_POINT('Ctrl Pts',(-57.7430685887949,-88.7623575781902,
178.710432055626));
#34278=CARTESIAN_POINT('Ctrl Pts',(-58.4005781238326,-88.7534997661608,
178.279269721459));
#34279=CARTESIAN_POINT('Ctrl Pts',(-58.6799123287478,-88.7530699805666,
178.007597618008));
#34280=CARTESIAN_POINT('Ctrl Pts',(-59.1296739375624,-88.7692390572475,
177.362779114218));
#34281=CARTESIAN_POINT('Ctrl Pts',(-59.2912554998927,-88.7848799843777,
176.992817647715));
#34282=CARTESIAN_POINT('Ctrl Pts',(-59.4580244949498,-88.8284055944828,
176.225797860729));
#34283=CARTESIAN_POINT('Ctrl Pts',(-59.4670141404289,-88.8567214239698,
175.837304583598));
#34284=CARTESIAN_POINT('Ctrl Pts',(-59.3368366833603,-88.934676455815,175.065934646549));
#34285=CARTESIAN_POINT('Ctrl Pts',(-59.1936101856561,-88.9828130954779,
174.691427261397));
#34286=CARTESIAN_POINT('Ctrl Pts',(-58.7770321126355,-89.0885970625982,
174.033381480313));
#34287=CARTESIAN_POINT('Ctrl Pts',(-58.5123353943137,-89.1460148183289,
173.753328914884));
#34288=CARTESIAN_POINT('Ctrl Pts',(-57.8819764068814,-89.2772508593794,
173.302601761779));
#34289=CARTESIAN_POINT('Ctrl Pts',(-57.5192586279044,-89.3487873024151,
173.140548522746));
#34290=CARTESIAN_POINT('Ctrl Pts',(-56.7648259432275,-89.4906608863938,
172.972676652572));
#34291=CARTESIAN_POINT('Ctrl Pts',(-56.3816889784975,-89.5606307884222,
172.963324417664));
#34292=CARTESIAN_POINT('Ctrl Pts',(-55.6206076806915,-89.7057586889692,
173.09416500872));
#34293=CARTESIAN_POINT('Ctrl Pts',(-55.2507109162235,-89.7780603762169,
173.238186049348));
#34294=CARTESIAN_POINT('Ctrl Pts',(-54.8390972685506,-89.8608153127105,
173.503077007167));
#34295=CARTESIAN_POINT('Ctrl Pts',(-54.7613681906975,-89.8765644360083,
173.558636887198));
#34296=CARTESIAN_POINT('Ctrl Pts',(-54.686534407881,-89.891851533879,173.617797875547));
#34297=CARTESIAN_POINT('Ctrl Pts',(-54.7395374101039,-90.3890342787078,
173.617797875548));
#34298=CARTESIAN_POINT('Ctrl Pts',(-54.7536254637881,-90.3861563611768,
173.606660349841));
#34299=CARTESIAN_POINT('Ctrl Pts',(-54.7678182303282,-90.3832616402047,
173.595648805531));
#34300=CARTESIAN_POINT('Ctrl Pts',(-55.0982533651628,-90.3159724008806,
173.344078904514));
#34301=CARTESIAN_POINT('Ctrl Pts',(-55.4589009037588,-90.244746248267,173.170330584284));
#34302=CARTESIAN_POINT('Ctrl Pts',(-56.2121090481486,-90.0997986432487,
172.980726626293));
#34303=CARTESIAN_POINT('Ctrl Pts',(-56.595927926668,-90.0280296445997,172.961040933605));
#34304=CARTESIAN_POINT('Ctrl Pts',(-57.364692387148,-89.8859045163428,173.072342018584));
#34305=CARTESIAN_POINT('Ctrl Pts',(-57.740943444431,-89.8130160471777,173.208232122973));
#34306=CARTESIAN_POINT('Ctrl Pts',(-58.4050713366844,-89.677561539593,173.614336496615));
#34307=CARTESIAN_POINT('Ctrl Pts',(-58.6894857142339,-89.6163763313695,
173.875548982126));
#34308=CARTESIAN_POINT('Ctrl Pts',(-59.1532617495717,-89.5067731061024,
174.505256478686));
#34309=CARTESIAN_POINT('Ctrl Pts',(-59.3229162292159,-89.455910265214,174.871300750203));
#34310=CARTESIAN_POINT('Ctrl Pts',(-59.5053156644829,-89.3718080168573,
175.635526450194));
#34311=CARTESIAN_POINT('Ctrl Pts',(-59.5219693261846,-89.3391553739719,
176.024801063651));
#34312=CARTESIAN_POINT('Ctrl Pts',(-59.4056032603791,-89.2914067264333,
176.80445156296));
#34313=CARTESIAN_POINT('Ctrl Pts',(-59.2673278848242,-89.2733722520209,
177.186454382289));
#34314=CARTESIAN_POINT('Ctrl Pts',(-58.8572117329723,-89.2524331345483,
177.861580919718));
#34315=CARTESIAN_POINT('Ctrl Pts',(-58.5944281193864,-89.2495586805081,
178.151106738878));
#34316=CARTESIAN_POINT('Ctrl Pts',(-57.9622569533401,-89.2568053463866,
178.624417870856));
#34317=CARTESIAN_POINT('Ctrl Pts',(-57.5949256922417,-89.2631906837858,
178.798805174538));
#34318=CARTESIAN_POINT('Ctrl Pts',(-56.8282798696182,-89.280257229962,178.989685525946));
#34319=CARTESIAN_POINT('Ctrl Pts',(-56.4379325091458,-89.2909710055577,
179.009998109976));
#34320=CARTESIAN_POINT('Ctrl Pts',(-55.6562050183527,-89.3141679414693,
178.899915840531));
#34321=CARTESIAN_POINT('Ctrl Pts',(-55.2727748448249,-89.3222703955619,
178.764596795762));
#34322=CARTESIAN_POINT('Ctrl Pts',(-54.5943065964784,-89.3299340357216,
178.359461637739));
#34323=CARTESIAN_POINT('Ctrl Pts',(-54.3029571080176,-89.3300837842501,
178.098649388314));
#34324=CARTESIAN_POINT('Ctrl Pts',(-53.8255171030039,-89.3208477620272,
177.469558737649));
#34325=CARTESIAN_POINT('Ctrl Pts',(-53.6484015612722,-89.3069565074131,
177.103712395319));
#34326=CARTESIAN_POINT('Ctrl Pts',(-53.4512680624326,-89.2633042403586,
176.339655732208));
#34327=CARTESIAN_POINT('Ctrl Pts',(-53.4275592631866,-89.2349121908259,
175.950364200724));
#34328=CARTESIAN_POINT('Ctrl Pts',(-53.5301943217796,-89.1638419955626,
175.170468526992));
#34329=CARTESIAN_POINT('Ctrl Pts',(-53.661067303405,-89.117117863704,174.788230851258));
#34330=CARTESIAN_POINT('Ctrl Pts',(-54.0490890144365,-89.0123282517972,
174.125508908105));
#34331=CARTESIAN_POINT('Ctrl Pts',(-54.292569942137,-88.9563104015491,173.845447828985));
#34332=CARTESIAN_POINT('Ctrl Pts',(-54.5805284034317,-88.8974860442222,
173.617797875548));
#34333=CARTESIAN_POINT('Origin',(-54.1598171290174,-67.5719248685924,175.985485069079));
#34334=CARTESIAN_POINT('',(-54.3685163945356,-86.908755064908,173.617797875548));
#34335=CARTESIAN_POINT('',(-54.4215193967595,-87.4059378097366,173.617797875548));
#34336=CARTESIAN_POINT('',(-52.327900808713,-67.7672193871761,173.617797875548));
#34337=CARTESIAN_POINT('Ctrl Pts',(-54.3685163945357,-86.908755064908,173.617797875548));
#34338=CARTESIAN_POINT('Ctrl Pts',(-54.1029134234621,-86.9630126269441,
173.827774355231));
#34339=CARTESIAN_POINT('Ctrl Pts',(-53.8749031255443,-87.0149320416049,
174.082522212409));
#34340=CARTESIAN_POINT('Ctrl Pts',(-53.4839217198981,-87.1175329221976,
174.708627630965));
#34341=CARTESIAN_POINT('Ctrl Pts',(-53.3425096711802,-87.165439707321,175.085665523802));
#34342=CARTESIAN_POINT('Ctrl Pts',(-53.217327784721,-87.2394477467716,175.860123223724));
#34343=CARTESIAN_POINT('Ctrl Pts',(-53.2293355299918,-87.2682568338261,
176.249055654486));
#34344=CARTESIAN_POINT('Ctrl Pts',(-53.4028417589691,-87.3141841401225,
177.016565188295));
#34345=CARTESIAN_POINT('Ctrl Pts',(-53.5681002985076,-87.3294012224974,
177.386475181806));
#34346=CARTESIAN_POINT('Ctrl Pts',(-54.0244567155213,-87.3414536350706,
178.02860024861));
#34347=CARTESIAN_POINT('Ctrl Pts',(-54.3066838638898,-87.3413982130645,
178.297952302799));
#34348=CARTESIAN_POINT('Ctrl Pts',(-54.9699021379563,-87.3350990058782,
178.723581420034));
#34349=CARTESIAN_POINT('Ctrl Pts',(-55.3474236314889,-87.3276908946758,
178.870954732385));
#34350=CARTESIAN_POINT('Ctrl Pts',(-56.1230261659881,-87.3057520135597,
179.006897705685));
#34351=CARTESIAN_POINT('Ctrl Pts',(-56.5128705872014,-87.2941642204602,
178.999870109779));
#34352=CARTESIAN_POINT('Ctrl Pts',(-57.2833550787784,-87.2764084214759,
178.835977058011));
#34353=CARTESIAN_POINT('Ctrl Pts',(-57.655250097498,-87.2696035857755,178.67516561695));
#34354=CARTESIAN_POINT('Ctrl Pts',(-58.3021881708129,-87.2614259727787,
178.226047615204));
#34355=CARTESIAN_POINT('Ctrl Pts',(-58.5745176094255,-87.2623041320782,
177.94683862187));
#34356=CARTESIAN_POINT('Ctrl Pts',(-59.0077172301551,-87.2804824200033,
177.289126552806));
#34357=CARTESIAN_POINT('Ctrl Pts',(-59.1595907756512,-87.2971367709562,
176.913918521583));
#34358=CARTESIAN_POINT('Ctrl Pts',(-59.3052160159744,-87.3424495960633,
176.141379741915));
#34359=CARTESIAN_POINT('Ctrl Pts',(-59.3034448447673,-87.3724845845416,
175.752566156436));
#34360=CARTESIAN_POINT('Ctrl Pts',(-59.1514503037943,-87.4530242277975,
174.98397360187));
#34361=CARTESIAN_POINT('Ctrl Pts',(-58.9971285531111,-87.5023244100845,
174.612779848241));
#34362=CARTESIAN_POINT('Ctrl Pts',(-58.5607371146546,-87.6097336617945,
173.966353225289));
#34363=CARTESIAN_POINT('Ctrl Pts',(-58.2878343094946,-87.6686068793633,
173.694141673873));
#34364=CARTESIAN_POINT('Ctrl Pts',(-57.6433222454351,-87.8016263280554,
173.261740441671));
#34365=CARTESIAN_POINT('Ctrl Pts',(-57.2747814021579,-87.8737669662917,
173.110395606436));
#34366=CARTESIAN_POINT('Ctrl Pts',(-56.5141636936474,-88.0157929314995,
172.965865670225));
#34367=CARTESIAN_POINT('Ctrl Pts',(-56.1307417720863,-88.0863800636285,
172.968487293171));
#34368=CARTESIAN_POINT('Ctrl Pts',(-55.3726400952361,-88.2314813856136,
173.123462718543));
#34369=CARTESIAN_POINT('Ctrl Pts',(-55.0062691489335,-88.3033938284711,
173.279760181978));
#34370=CARTESIAN_POINT('Ctrl Pts',(-54.6285746166461,-88.3797183894738,
173.540528378013));
#34371=CARTESIAN_POINT('Ctrl Pts',(-54.5774011679008,-88.3901146426384,
173.578367827498));
#34372=CARTESIAN_POINT('Ctrl Pts',(-54.5275254012084,-88.4003032993935,
173.617797875547));
#34373=CARTESIAN_POINT('Ctrl Pts',(-54.5805284034317,-88.8974860442222,
173.617797875548));
#34374=CARTESIAN_POINT('Ctrl Pts',(-54.592304347756,-88.89508044602,173.608488223159));
#34375=CARTESIAN_POINT('Ctrl Pts',(-54.604153503143,-88.8926630974012,173.599266555514));
#34376=CARTESIAN_POINT('Ctrl Pts',(-54.9315971883393,-88.8259488965967,
173.348420700598));
#34377=CARTESIAN_POINT('Ctrl Pts',(-55.291848201925,-88.7547722417383,173.173552135254));
#34378=CARTESIAN_POINT('Ctrl Pts',(-56.0447147782708,-88.6098392974242,
172.981710015181));
#34379=CARTESIAN_POINT('Ctrl Pts',(-56.4285586273302,-88.537982258094,172.960925148545));
#34380=CARTESIAN_POINT('Ctrl Pts',(-57.1978210124498,-88.3958554029432,
173.070089317494));
#34381=CARTESIAN_POINT('Ctrl Pts',(-57.5745445588047,-88.3229233273283,
173.204978017596));
#34382=CARTESIAN_POINT('Ctrl Pts',(-58.239912727543,-88.1873163601604,173.609382874055));
#34383=CARTESIAN_POINT('Ctrl Pts',(-58.5250611020044,-88.1259731967198,
173.869893773846));
#34384=CARTESIAN_POINT('Ctrl Pts',(-58.9905661098442,-88.0162335199632,
174.498519613728));
#34385=CARTESIAN_POINT('Ctrl Pts',(-59.1611878212844,-87.9652738946288,
174.86421645565));
#34386=CARTESIAN_POINT('Ctrl Pts',(-59.3455168063876,-87.8809471158559,
175.62814538344));
#34387=CARTESIAN_POINT('Ctrl Pts',(-59.363111134507,-87.8481198021688,176.017449655811));
#34388=CARTESIAN_POINT('Ctrl Pts',(-59.2485936583136,-87.8002186934163,
176.797529305977));
#34389=CARTESIAN_POINT('Ctrl Pts',(-59.1111831652141,-87.7820979358716,
177.179943240195));
#34390=CARTESIAN_POINT('Ctrl Pts',(-58.7025318440207,-87.7609851429597,
177.856153465695));
#34391=CARTESIAN_POINT('Ctrl Pts',(-58.4403461617647,-87.757977536504,178.146327034948));
#34392=CARTESIAN_POINT('Ctrl Pts',(-57.8091128610305,-87.7651657876644,
178.621141802717));
#34393=CARTESIAN_POINT('Ctrl Pts',(-57.4420823604527,-87.7715245954983,
178.796372126317));
#34394=CARTESIAN_POINT('Ctrl Pts',(-56.6756912855874,-87.7885476910923,
178.988937440833));
#34395=CARTESIAN_POINT('Ctrl Pts',(-56.2853115113751,-87.7992001763368,
179.010077390318));
#34396=CARTESIAN_POINT('Ctrl Pts',(-55.5032184787108,-87.8224748083139,
178.901603419635));
#34397=CARTESIAN_POINT('Ctrl Pts',(-55.1194347368525,-87.8306201261721,
178.7670383405));
#34398=CARTESIAN_POINT('Ctrl Pts',(-54.4400306868328,-87.8383683735314,
178.363182624418));
#34399=CARTESIAN_POINT('Ctrl Pts',(-54.1481162878296,-87.8385179630927,
178.102898192409));
#34400=CARTESIAN_POINT('Ctrl Pts',(-53.6693839012453,-87.8294557922013,
177.474621870949));
#34401=CARTESIAN_POINT('Ctrl Pts',(-53.4915421823287,-87.8156467834496,
177.109037647409));
#34402=CARTESIAN_POINT('Ctrl Pts',(-53.2929545172073,-87.7721354430938,
176.345204975317));
#34403=CARTESIAN_POINT('Ctrl Pts',(-53.268526519972,-87.7437637642731,175.955891126618));
#34404=CARTESIAN_POINT('Ctrl Pts',(-53.3697786896165,-87.6728745941867,
175.175673567676));
#34405=CARTESIAN_POINT('Ctrl Pts',(-53.5000020944734,-87.6262242224846,
174.793127496324));
#34406=CARTESIAN_POINT('Ctrl Pts',(-53.8877865868758,-87.5213083526867,
174.128156458117));
#34407=CARTESIAN_POINT('Ctrl Pts',(-54.1321940868959,-87.465041387852,173.846528411968));
#34408=CARTESIAN_POINT('Ctrl Pts',(-54.4215193967595,-87.4059378097366,
173.617797875548));
#34409=CARTESIAN_POINT('Origin',(-54.1598171290174,-67.5719248685924,175.985485069079));
#34410=CARTESIAN_POINT('',(-54.2095073878632,-85.4172068304224,173.617797875548));
#34411=CARTESIAN_POINT('',(-54.2625103900873,-85.914389575251,173.617797875548));
#34412=CARTESIAN_POINT('',(-52.327900808713,-67.7672193871761,173.617797875548));
#34413=CARTESIAN_POINT('Ctrl Pts',(-54.2095073878633,-85.4172068304224,
173.617797875548));
#34414=CARTESIAN_POINT('Ctrl Pts',(-53.9332619774107,-85.473638437472,173.836187897997));
#34415=CARTESIAN_POINT('Ctrl Pts',(-53.6978124997361,-85.5275145906288,
174.102912189541));
#34416=CARTESIAN_POINT('Ctrl Pts',(-53.3080240280004,-85.631186385472,174.746408240766));
#34417=CARTESIAN_POINT('Ctrl Pts',(-53.1716090248673,-85.6785357557079,
175.12595808378));
#34418=CARTESIAN_POINT('Ctrl Pts',(-53.0571443781225,-85.7511505542224,
175.903045422152));
#34419=CARTESIAN_POINT('Ctrl Pts',(-53.0747085639042,-85.7797413584373,
176.29214731336));
#34420=CARTESIAN_POINT('Ctrl Pts',(-53.2594265255084,-85.8245925543852,
177.058062082337));
#34421=CARTESIAN_POINT('Ctrl Pts',(-53.4303247636375,-85.8391830097732,
177.426089782173));
#34422=CARTESIAN_POINT('Ctrl Pts',(-53.8967058701507,-85.8499009319195,
178.062075923266));
#34423=CARTESIAN_POINT('Ctrl Pts',(-54.1832488382114,-85.8497779723597,
178.32738366672));
#34424=CARTESIAN_POINT('Ctrl Pts',(-54.8537139825916,-85.842833703405,178.74335647834));
#34425=CARTESIAN_POINT('Ctrl Pts',(-55.2340772721629,-85.8350966284344,
178.885055963083));
#34426=CARTESIAN_POINT('Ctrl Pts',(-56.0126295423935,-85.8125617841953,
179.008790586575));
#34427=CARTESIAN_POINT('Ctrl Pts',(-56.4027069366073,-85.8013603685799,
178.995495185527));
#34428=CARTESIAN_POINT('Ctrl Pts',(-57.1714392733414,-85.7839277598787,
178.818886663266));
#34429=CARTESIAN_POINT('Ctrl Pts',(-57.5412436559841,-85.7773192886942,
178.651662075905));
#34430=CARTESIAN_POINT('Ctrl Pts',(-58.1812837764483,-85.769579214134,178.191119255375));
#34431=CARTESIAN_POINT('Ctrl Pts',(-58.4491221618275,-85.7713660718236,
177.907062514141));
#34432=CARTESIAN_POINT('Ctrl Pts',(-58.8715335140524,-85.790840307223,177.241132176311));
#34433=CARTESIAN_POINT('Ctrl Pts',(-59.017059928142,-85.8081444246837,176.862674162691));
#34434=CARTESIAN_POINT('Ctrl Pts',(-59.1489804595095,-85.85460350698,176.086729179939));
#34435=CARTESIAN_POINT('Ctrl Pts',(-59.1402390484174,-85.8858301162748,
175.697701855906));
#34436=CARTESIAN_POINT('Ctrl Pts',(-58.974034668921,-85.968040490002,174.931077916915));
#34437=CARTESIAN_POINT('Ctrl Pts',(-58.8125265331801,-86.0180796985493,
174.56221435483));
#34438=CARTESIAN_POINT('Ctrl Pts',(-58.363303890959,-86.1265245857877,173.923525340057));
#34439=CARTESIAN_POINT('Ctrl Pts',(-58.0850332582311,-86.1864369832083,
173.656442059579));
#34440=CARTESIAN_POINT('Ctrl Pts',(-57.4313372083917,-86.3206019885938,
173.236218802077));
#34441=CARTESIAN_POINT('Ctrl Pts',(-57.0591320567907,-86.393106152254,173.092020404767));
#34442=CARTESIAN_POINT('Ctrl Pts',(-56.294637190197,-86.5351951521233,172.962917148004));
#34443=CARTESIAN_POINT('Ctrl Pts',(-55.9110292620967,-86.6062870231821,
172.973455605913));
#34444=CARTESIAN_POINT('Ctrl Pts',(-55.1551026662993,-86.7513341797469,
173.144467091908));
#34445=CARTESIAN_POINT('Ctrl Pts',(-54.7912855834294,-86.8229474419353,
173.308872270221));
#34446=CARTESIAN_POINT('Ctrl Pts',(-54.4356971143808,-86.8950569693321,
173.56585347481));
#34447=CARTESIAN_POINT('Ctrl Pts',(-54.4018159408511,-86.9019526101287,
173.591472411333));
#34448=CARTESIAN_POINT('Ctrl Pts',(-54.3685163945357,-86.908755064908,173.617797875548));
#34449=CARTESIAN_POINT('Ctrl Pts',(-54.4215193967595,-87.4059378097366,
173.617797875548));
#34450=CARTESIAN_POINT('Ctrl Pts',(-54.4319874202367,-87.4037993945264,
173.609522219933));
#34451=CARTESIAN_POINT('Ctrl Pts',(-54.4425133166328,-87.401651689743,173.601316073085));
#34452=CARTESIAN_POINT('Ctrl Pts',(-54.7682682986267,-87.3352622732361,
173.350886654411));
#34453=CARTESIAN_POINT('Ctrl Pts',(-55.1282935773606,-87.2641138943975,
173.175384803604));
#34454=CARTESIAN_POINT('Ctrl Pts',(-55.8809655577316,-87.1191894994919,
172.982276537438));
#34455=CARTESIAN_POINT('Ctrl Pts',(-56.2648234871258,-87.0472820411832,
172.960870028795));
#34456=CARTESIAN_POINT('Ctrl Pts',(-57.0343660410513,-86.9051544556821,
173.068825910744));
#34457=CARTESIAN_POINT('Ctrl Pts',(-57.4113554997123,-86.8321979622416,
173.203148010723));
#34458=CARTESIAN_POINT('Ctrl Pts',(-58.0774238349211,-86.6965050095272,
173.606591451899));
#34459=CARTESIAN_POINT('Ctrl Pts',(-58.3629869156974,-86.6350720497216,
173.866705931947));
#34460=CARTESIAN_POINT('Ctrl Pts',(-58.8294678567425,-86.5252554612533,
174.494719841926));
#34461=CARTESIAN_POINT('Ctrl Pts',(-59.0006354631639,-86.4742413068587,
174.860219401169));
#34462=CARTESIAN_POINT('Ctrl Pts',(-59.1860541207935,-86.3897878119418,
175.623979691486));
#34463=CARTESIAN_POINT('Ctrl Pts',(-59.2041794913773,-86.3568614115411,
176.01330072742));
#34464=CARTESIAN_POINT('Ctrl Pts',(-59.0907055295616,-86.308874314158,176.79362158147));
#34465=CARTESIAN_POINT('Ctrl Pts',(-58.9537835370001,-86.2907048997491,
177.176266632583));
#34466=CARTESIAN_POINT('Ctrl Pts',(-58.5459594382781,-86.2694941077165,
177.853087725861));
#34467=CARTESIAN_POINT('Ctrl Pts',(-58.2841110305906,-86.2664109768285,
178.14362674106));
#34468=CARTESIAN_POINT('Ctrl Pts',(-57.6534073895263,-86.2735662744409,
178.619289013214));
#34469=CARTESIAN_POINT('Ctrl Pts',(-57.286547293649,-86.2799101059405,178.79499443983));
#34470=CARTESIAN_POINT('Ctrl Pts',(-56.5203006495415,-86.2969086792263,
178.988509859046));
#34471=CARTESIAN_POINT('Ctrl Pts',(-56.1299025507582,-86.3075262609867,
179.010116242818));
#34472=CARTESIAN_POINT('Ctrl Pts',(-55.3476042608382,-86.3308446599301,
178.902548818617));
#34473=CARTESIAN_POINT('Ctrl Pts',(-54.9636219411715,-86.339014121752,178.768408933986));
#34474=CARTESIAN_POINT('Ctrl Pts',(-54.28369105841,-86.3468100467483,178.365274651518));
#34475=CARTESIAN_POINT('Ctrl Pts',(-53.9914583566946,-86.3469592427903,
178.105287575512));
#34476=CARTESIAN_POINT('Ctrl Pts',(-53.5119984547237,-86.3379949994304,
177.477470446987));
#34477=CARTESIAN_POINT('Ctrl Pts',(-53.3337479942983,-86.3242323378271,
177.112034440454));
#34478=CARTESIAN_POINT('Ctrl Pts',(-53.1343414415493,-86.2808004043142,
176.348328493555));
#34479=CARTESIAN_POINT('Ctrl Pts',(-53.1095084810868,-86.2524399309787,
175.959002069361));
#34480=CARTESIAN_POINT('Ctrl Pts',(-53.209982146529,-86.1816527120886,175.178603891707));
#34481=CARTESIAN_POINT('Ctrl Pts',(-53.3398397165186,-86.1350439249261,
174.795884743041));
#34482=CARTESIAN_POINT('Ctrl Pts',(-53.7274878481633,-86.0300573849754,
174.129647447484));
#34483=CARTESIAN_POINT('Ctrl Pts',(-53.9724158334711,-85.9736502956349,
173.84713655172));
#34484=CARTESIAN_POINT('Ctrl Pts',(-54.2625103900873,-85.914389575251,173.617797875548));
#34485=CARTESIAN_POINT('Origin',(-54.1598171290174,-67.5719248685924,175.985485069079));
#34486=CARTESIAN_POINT('',(-54.050498381191,-83.9256585959369,173.617797875548));
#34487=CARTESIAN_POINT('',(-54.1035013834151,-84.4228413407654,173.617797875548));
#34488=CARTESIAN_POINT('',(-52.327900808713,-67.7672193871761,173.617797875548));
#34489=CARTESIAN_POINT('Ctrl Pts',(-54.050498381191,-83.9256585959369,173.617797875548));
#34490=CARTESIAN_POINT('Ctrl Pts',(-53.7679065572478,-83.9833866528051,
173.841205151976));
#34491=CARTESIAN_POINT('Ctrl Pts',(-53.5280851485867,-84.0384247724667,
174.115135380727));
#34492=CARTESIAN_POINT('Ctrl Pts',(-53.1391948368034,-84.1427101835225,
174.769037761665));
#34493=CARTESIAN_POINT('Ctrl Pts',(-53.0057771809645,-84.1897223073407,
175.150053949138));
#34494=CARTESIAN_POINT('Ctrl Pts',(-52.8977174976408,-84.2615016781384,
175.928674036426));
#34495=CARTESIAN_POINT('Ctrl Pts',(-52.9186069647449,-84.2899794092634,
176.317878307109));
#34496=CARTESIAN_POINT('Ctrl Pts',(-53.1100418741121,-84.3341829233429,
177.082799875532));
#34497=CARTESIAN_POINT('Ctrl Pts',(-53.2843075286004,-84.3483957778167,
177.449660036152));
#34498=CARTESIAN_POINT('Ctrl Pts',(-53.7566771132667,-84.3583125141355,
178.081928347658));
#34499=CARTESIAN_POINT('Ctrl Pts',(-54.0458168038138,-84.3581688027116,
178.344806348492));
#34500=CARTESIAN_POINT('Ctrl Pts',(-54.7206146471591,-84.3508360098067,
178.75493492402));
#34501=CARTESIAN_POINT('Ctrl Pts',(-55.1026477851618,-84.3429013946851,
178.893195176074));
#34502=CARTESIAN_POINT('Ctrl Pts',(-55.8829299011184,-84.3200086326902,
179.009561251224));
#34503=CARTESIAN_POINT('Ctrl Pts',(-56.2731518250052,-84.3090631467957,
178.992479748983));
#34504=CARTESIAN_POINT('Ctrl Pts',(-57.0407748322682,-84.2918274973282,
178.808175263482));
#34505=CARTESIAN_POINT('Ctrl Pts',(-57.4092621611192,-84.2853389965204,
178.637083382537));
#34506=CARTESIAN_POINT('Ctrl Pts',(-58.0450756540518,-84.2778646839619,
178.169648162453));
#34507=CARTESIAN_POINT('Ctrl Pts',(-58.3101903712652,-84.280229093688,177.882646086267));
#34508=CARTESIAN_POINT('Ctrl Pts',(-58.7259964278775,-84.3004918881376,
177.21175299148));
#34509=CARTESIAN_POINT('Ctrl Pts',(-58.8676293943606,-84.3181897297269,
176.831369667309));
#34510=CARTESIAN_POINT('Ctrl Pts',(-58.991185174051,-84.3653438008588,176.053410903082));
#34511=CARTESIAN_POINT('Ctrl Pts',(-58.9781892577483,-84.3973275787765,
175.66425113474));
#34512=CARTESIAN_POINT('Ctrl Pts',(-58.8032846239125,-84.4805559295001,
174.898895026642));
#34513=CARTESIAN_POINT('Ctrl Pts',(-58.6373939973216,-84.5310401060385,
174.531524492106));
#34514=CARTESIAN_POINT('Ctrl Pts',(-58.1803437281115,-84.6401101784401,
173.897638942517));
#34515=CARTESIAN_POINT('Ctrl Pts',(-57.8987762263253,-84.7006946036871,
173.633705756515));
#34516=CARTESIAN_POINT('Ctrl Pts',(-57.2394712011691,-84.8355545270622,
173.221035260935));
#34517=CARTESIAN_POINT('Ctrl Pts',(-56.8650748640176,-84.9082691861619,
173.081278690915));
#34518=CARTESIAN_POINT('Ctrl Pts',(-56.0982663102263,-85.0503823778178,
172.96170957192));
#34519=CARTESIAN_POINT('Ctrl Pts',(-55.7145448066483,-85.1218243504424,
172.977144954069));
#34520=CARTESIAN_POINT('Ctrl Pts',(-54.9600460210043,-85.266823182249,173.158102082311));
#34521=CARTESIAN_POINT('Ctrl Pts',(-54.5978967227242,-85.3382347224806,
173.327513253623));
#34522=CARTESIAN_POINT('Ctrl Pts',(-54.255829777542,-85.4077563100731,173.581734482978));
#34523=CARTESIAN_POINT('Ctrl Pts',(-54.2325291387492,-85.4125039309337,
173.599597679264));
#34524=CARTESIAN_POINT('Ctrl Pts',(-54.2095073878633,-85.4172068304224,
173.617797875548));
#34525=CARTESIAN_POINT('Ctrl Pts',(-54.2625103900873,-85.914389575251,173.617797875548));
#34526=CARTESIAN_POINT('Ctrl Pts',(-54.272242730254,-85.9124014459457,173.610103825594));
#34527=CARTESIAN_POINT('Ctrl Pts',(-54.2820251050254,-85.910405284795,173.602469849516));
#34528=CARTESIAN_POINT('Ctrl Pts',(-54.6068313405509,-85.8441983922685,
173.352276841814));
#34529=CARTESIAN_POINT('Ctrl Pts',(-54.9667291943884,-85.7730660057973,
173.17641891249));
#34530=CARTESIAN_POINT('Ctrl Pts',(-55.7192912802216,-85.6281465011847,
172.982598442595));
#34531=CARTESIAN_POINT('Ctrl Pts',(-56.1031571149052,-85.556210487934,172.96084231474));
#34532=CARTESIAN_POINT('Ctrl Pts',(-56.8728567841258,-85.4140825697339,
173.068118723903));
#34533=CARTESIAN_POINT('Ctrl Pts',(-57.2499953804115,-85.3411124208112,
173.202122083087));
#34534=CARTESIAN_POINT('Ctrl Pts',(-57.9164570917249,-85.2053711845814,
173.605024735824));
#34535=CARTESIAN_POINT('Ctrl Pts',(-58.2022532786323,-85.1438875755383,
173.864916380031));
#34536=CARTESIAN_POINT('Ctrl Pts',(-58.6692824949556,-85.0340278130821,
174.492586073101));
#34537=CARTESIAN_POINT('Ctrl Pts',(-58.8407567608416,-84.9829830568063,
174.857974428286));
#34538=CARTESIAN_POINT('Ctrl Pts',(-59.0267877573062,-84.8984583802647,
175.621639622987));
#34539=CARTESIAN_POINT('Ctrl Pts',(-59.0452114899296,-84.865476157542,176.010970083441));
#34540=CARTESIAN_POINT('Ctrl Pts',(-58.9323237898062,-84.8174407740576,
176.791426117773));
#34541=CARTESIAN_POINT('Ctrl Pts',(-58.7956763323207,-84.7992440391595,
177.174200711645));
#34542=CARTESIAN_POINT('Ctrl Pts',(-58.3883170860243,-84.7779782022207,
177.851364725428));
#34543=CARTESIAN_POINT('Ctrl Pts',(-58.1266580846683,-84.7748525265982,
178.142108989257));
#34544=CARTESIAN_POINT('Ctrl Pts',(-57.4962520903143,-84.7819893171045,
178.618246995242));
#34545=CARTESIAN_POINT('Ctrl Pts',(-57.1294879282161,-84.7883247345141,
178.79421909619));
#34546=CARTESIAN_POINT('Ctrl Pts',(-56.3633226256829,-84.8053095324604,
178.988267968054));
#34547=CARTESIAN_POINT('Ctrl Pts',(-55.9729142234731,-84.8159074086289,
179.01013620997));
#34548=CARTESIAN_POINT('Ctrl Pts',(-55.1905009603469,-84.8392503674809,
178.903077677773));
#34549=CARTESIAN_POINT('Ctrl Pts',(-54.8064073951959,-84.8474333771942,
178.769176542408));
#34550=CARTESIAN_POINT('Ctrl Pts',(-54.1261809785311,-84.855256062124,178.366447318394));
#34551=CARTESIAN_POINT('Ctrl Pts',(-53.8337696343528,-84.8554049414776,
178.10662711442));
#34552=CARTESIAN_POINT('Ctrl Pts',(-53.3539016423839,-84.8464956488437,
177.479067812005));
#34553=CARTESIAN_POINT('Ctrl Pts',(-53.1754219176799,-84.8327590004161,
177.1137151551));
#34554=CARTESIAN_POINT('Ctrl Pts',(-52.9755559264343,-84.7893716329479,
176.350080493459));
#34555=CARTESIAN_POINT('Ctrl Pts',(-52.9504957729693,-84.7610173627157,
175.960747011359));
#34556=CARTESIAN_POINT('Ctrl Pts',(-53.050532734403,-84.6902873469128,175.180247700522));
#34557=CARTESIAN_POINT('Ctrl Pts',(-53.1801850405792,-84.64370190587,174.797431632577));
#34558=CARTESIAN_POINT('Ctrl Pts',(-53.5677557922408,-84.5386758518192,
174.130483990877));
#34559=CARTESIAN_POINT('Ctrl Pts',(-53.8129753877958,-84.4821901958128,
173.847477632404));
#34560=CARTESIAN_POINT('Ctrl Pts',(-54.1035013834151,-84.4228413407654,
173.617797875548));
#34561=CARTESIAN_POINT('Origin',(-54.1598171290174,-67.5719248685924,175.985485069079));
#34562=CARTESIAN_POINT('',(-53.8914893745187,-82.4341103614513,173.617797875548));
#34563=CARTESIAN_POINT('',(-53.9444923767428,-82.9312931062798,173.617797875548));
#34564=CARTESIAN_POINT('',(-52.327900808713,-67.7672193871761,173.617797875548));
#34565=CARTESIAN_POINT('Ctrl Pts',(-53.8914893745187,-82.4341103614513,
173.617797875548));
#34566=CARTESIAN_POINT('Ctrl Pts',(-53.6052173838758,-82.4925902053654,
173.844114563889));
#34567=CARTESIAN_POINT('Ctrl Pts',(-53.3628827650752,-82.548300455384,174.122245324128));
#34568=CARTESIAN_POINT('Ctrl Pts',(-52.9745773142937,-82.6529330761562,
174.782193804106));
#34569=CARTESIAN_POINT('Ctrl Pts',(-52.8429036775367,-82.6997479866898,
175.164049452677));
#34570=CARTESIAN_POINT('Ctrl Pts',(-52.7385630731543,-82.7710413119158,
175.943546295482));
#34571=CARTESIAN_POINT('Ctrl Pts',(-52.7613851386593,-82.7994593074702,
176.332810341507));
#34572=CARTESIAN_POINT('Ctrl Pts',(-52.9567259886705,-82.8432851590703,
177.09714129416));
#34573=CARTESIAN_POINT('Ctrl Pts',(-53.1329457267273,-82.8572777035077,
177.463308860173));
#34574=CARTESIAN_POINT('Ctrl Pts',(-53.6087916933352,-82.8667279618698,
178.093401456761));
#34575=CARTESIAN_POINT('Ctrl Pts',(-53.8994453490787,-82.8665789681866,
178.354863996896));
#34576=CARTESIAN_POINT('Ctrl Pts',(-54.5767595142852,-82.8590195272374,
178.761573480636));
#34577=CARTESIAN_POINT('Ctrl Pts',(-54.9597521761209,-82.8509698951223,
178.897820073131));
#34578=CARTESIAN_POINT('Ctrl Pts',(-55.7410271945383,-82.82786869725,179.00988231131));
#34579=CARTESIAN_POINT('Ctrl Pts',(-56.1313348213151,-82.8170805779664,
178.990588066779));
#34580=CARTESIAN_POINT('Ctrl Pts',(-56.8982916580408,-82.7999606351723,
178.801780992175));
#34581=CARTESIAN_POINT('Ctrl Pts',(-57.2659904558858,-82.7935427075112,
178.62843176922));
#34582=CARTESIAN_POINT('Ctrl Pts',(-57.8993130645951,-82.7862242116862,
178.156971903279));
#34583=CARTESIAN_POINT('Ctrl Pts',(-58.162832051056,-82.7889362062128,177.868242504181));
#34584=CARTESIAN_POINT('Ctrl Pts',(-58.5747467536174,-82.8096618354097,
177.194450000255));
#34585=CARTESIAN_POINT('Ctrl Pts',(-58.714083785481,-82.8275901558622,176.812955208202));
#34586=CARTESIAN_POINT('Ctrl Pts',(-58.8327209080309,-82.8751512680903,
176.033835190665));
#34587=CARTESIAN_POINT('Ctrl Pts',(-58.8172227638605,-82.9075908303593,
175.644596944486));
#34588=CARTESIAN_POINT('Ctrl Pts',(-58.6371924350539,-82.9914171440261,
174.880010087987));
#34589=CARTESIAN_POINT('Ctrl Pts',(-58.4687265318774,-83.0421607578069,
174.513542586584));
#34590=CARTESIAN_POINT('Ctrl Pts',(-58.0070747818638,-83.1515959942863,
173.882510394372));
#34591=CARTESIAN_POINT('Ctrl Pts',(-57.723561004971,-83.2125891039599,173.620437149146));
#34592=CARTESIAN_POINT('Ctrl Pts',(-57.0609567057928,-83.3478560739444,
173.212251191466));
#34593=CARTESIAN_POINT('Ctrl Pts',(-56.6852885925139,-83.4206903615588,
173.075134902459));
#34594=CARTESIAN_POINT('Ctrl Pts',(-55.9171386449002,-83.5628126136344,
172.961214764093));
#34595=CARTESIAN_POINT('Ctrl Pts',(-55.5333504855745,-83.6344756760652,
172.979553669503));
#34596=CARTESIAN_POINT('Ctrl Pts',(-54.7797281985092,-83.7794404514502,
173.166416362847));
#34597=CARTESIAN_POINT('Ctrl Pts',(-54.4185993701294,-83.8507263819771,
173.338791269425));
#34598=CARTESIAN_POINT('Ctrl Pts',(-54.0844894249589,-83.9187214986427,
173.591226869333));
#34599=CARTESIAN_POINT('Ctrl Pts',(-54.0674184433917,-83.9222021537111,
173.604421462315));
#34600=CARTESIAN_POINT('Ctrl Pts',(-54.050498381191,-83.9256585959369,173.617797875548));
#34601=CARTESIAN_POINT('Ctrl Pts',(-54.1035013834151,-84.4228413407654,
173.617797875548));
#34602=CARTESIAN_POINT('Ctrl Pts',(-54.1128212346228,-84.4209374749952,
173.610429925032));
#34603=CARTESIAN_POINT('Ctrl Pts',(-54.1221869743567,-84.4190262427001,
173.603117059851));
#34604=CARTESIAN_POINT('Ctrl Pts',(-54.4464616129933,-84.3529216380611,
173.353057288645));
#34605=CARTESIAN_POINT('Ctrl Pts',(-54.8062878786021,-84.281798245904,173.17699975264));
#34606=CARTESIAN_POINT('Ctrl Pts',(-55.5587882099357,-84.1368815088752,
172.982779952793));
#34607=CARTESIAN_POINT('Ctrl Pts',(-55.9426584723413,-84.0649294238171,
172.960827811178));
#34608=CARTESIAN_POINT('Ctrl Pts',(-56.7124460848245,-83.9228013436527,
173.067723300916));
#34609=CARTESIAN_POINT('Ctrl Pts',(-57.0896681643246,-83.8498235631671,
173.201547934183));
#34610=CARTESIAN_POINT('Ctrl Pts',(-57.7563502935406,-83.7140552807198,
173.604147370507));
#34611=CARTESIAN_POINT('Ctrl Pts',(-58.0422771302896,-83.6525432291579,
173.863914118319));
#34612=CARTESIAN_POINT('Ctrl Pts',(-58.509613547136,-83.5426592870856,174.491390807906));
#34613=CARTESIAN_POINT('Ctrl Pts',(-58.6812596282787,-83.4915973946548,
174.856716738244));
#34614=CARTESIAN_POINT('Ctrl Pts',(-58.8676337722894,-83.4070328370076,
175.620328538552));
#34615=CARTESIAN_POINT('Ctrl Pts',(-58.8862246860382,-83.3740192878531,
176.009664281697));
#34616=CARTESIAN_POINT('Ctrl Pts',(-58.7736654764938,-83.3259568564042,
176.790195955194));
#34617=CARTESIAN_POINT('Ctrl Pts',(-58.6371718724744,-83.3077448183863,
177.173043038668));
#34618=CARTESIAN_POINT('Ctrl Pts',(-58.2300731230129,-83.2864481429317,
177.850399109429));
#34619=CARTESIAN_POINT('Ctrl Pts',(-57.9685202237763,-83.283298593099,178.141258356762));
#34620=CARTESIAN_POINT('Ctrl Pts',(-57.3382810288697,-83.2904250159173,
178.61766279528));
#34621=CARTESIAN_POINT('Ctrl Pts',(-56.9715706818997,-83.2967557187476,
178.793784240335));
#34622=CARTESIAN_POINT('Ctrl Pts',(-56.2054510184505,-83.3137327987006,
178.988131909377));
#34623=CARTESIAN_POINT('Ctrl Pts',(-55.8150368404808,-83.3243196033431,
179.010146813958));
#34624=CARTESIAN_POINT('Ctrl Pts',(-55.0325592640291,-83.3476763143398,
178.903373289319));
#34625=CARTESIAN_POINT('Ctrl Pts',(-54.6484034664701,-83.3558669099257,
178.769605887138));
#34626=CARTESIAN_POINT('Ctrl Pts',(-53.9680115988919,-83.36370458063,178.367103543302));
#34627=CARTESIAN_POINT('Ctrl Pts',(-53.6755002168483,-83.3638532525733,
178.107376781389));
#34628=CARTESIAN_POINT('Ctrl Pts',(-53.1954037669401,-83.3549747287394,
177.479961893673));
#34629=CARTESIAN_POINT('Ctrl Pts',(-53.0167956993358,-83.3412526478882,
177.114655963443));
#34630=CARTESIAN_POINT('Ctrl Pts',(-52.8166724744574,-83.2978902369778,
176.351061271843));
#34631=CARTESIAN_POINT('Ctrl Pts',(-52.7914851224319,-83.2695394135183,
175.961723837377));
#34632=CARTESIAN_POINT('Ctrl Pts',(-52.8912776032413,-83.1988414259702,
175.181167967157));
#34633=CARTESIAN_POINT('Ctrl Pts',(-53.0208149813474,-83.1522690608241,
174.798297693757));
#34634=CARTESIAN_POINT('Ctrl Pts',(-53.4083421346692,-83.0472209258735,
174.130952367036));
#34635=CARTESIAN_POINT('Ctrl Pts',(-53.6537248706633,-82.9906912972542,
173.847668562182));
#34636=CARTESIAN_POINT('Ctrl Pts',(-53.9444923767429,-82.9312931062798,
173.617797875548));
#34637=CARTESIAN_POINT('Origin',(-54.1598171290174,-67.5719248685924,175.985485069079));
#34638=CARTESIAN_POINT('',(-53.7324803678465,-80.9425621269657,173.617797875548));
#34639=CARTESIAN_POINT('',(-53.7854833700705,-81.4397448717942,173.617797875548));
#34640=CARTESIAN_POINT('',(-52.327900808713,-67.7672193871761,173.617797875548));
#34641=CARTESIAN_POINT('Ctrl Pts',(-53.7324803678465,-80.9425621269657,
173.617797875548));
#34642=CARTESIAN_POINT('Ctrl Pts',(-53.4441088643015,-81.0014708608545,
173.845774365835));
#34643=CARTESIAN_POINT('Ctrl Pts',(-53.2003477048595,-81.0575640078217,
174.126308725592));
#34644=CARTESIAN_POINT('Ctrl Pts',(-52.8123969930906,-81.1623918656509,
174.789710194828));
#34645=CARTESIAN_POINT('Ctrl Pts',(-52.6817202418458,-81.2090937257845,
175.172041179413));
#34646=CARTESIAN_POINT('Ctrl Pts',(-52.5795030176814,-81.2801092351177,
175.952034250505));
#34647=CARTESIAN_POINT('Ctrl Pts',(-52.6034290990334,-81.3084950668171,
176.34133252214));
#34648=CARTESIAN_POINT('Ctrl Pts',(-52.8010019068039,-81.3521047705371,
177.105321657696));
#34649=CARTESIAN_POINT('Ctrl Pts',(-52.978336875166,-81.3659711860284,177.471088959042));
#34650=CARTESIAN_POINT('Ctrl Pts',(-53.4561673771093,-81.375154693423,178.099933745925));
#34651=CARTESIAN_POINT('Ctrl Pts',(-53.7476874832628,-81.3750049200971,
178.36058656955));
#34652=CARTESIAN_POINT('Ctrl Pts',(-54.4264384758535,-81.367315727599,178.765335428131));
#34653=CARTESIAN_POINT('Ctrl Pts',(-54.8099755898715,-81.3592003256552,
178.900426843859));
#34654=CARTESIAN_POINT('Ctrl Pts',(-55.5918136536326,-81.335979920787,179.010023446643));
#34655=CARTESIAN_POINT('Ctrl Pts',(-55.9821707892603,-81.3252845681812,
178.989461036256));
#34656=CARTESIAN_POINT('Ctrl Pts',(-56.7487398844479,-81.3082311356992,
178.798071949872));
#34657=CARTESIAN_POINT('Ctrl Pts',(-57.1159805326535,-81.301853804198,178.623430055959));
#34658=CARTESIAN_POINT('Ctrl Pts',(-57.7478687290417,-81.2946247716651,
178.149664851699));
#34659=CARTESIAN_POINT('Ctrl Pts',(-58.0104718390867,-81.2975393219991,
177.859943506638));
#34660=CARTESIAN_POINT('Ctrl Pts',(-58.4201460168419,-81.3185308603792,
177.184489728788));
#34661=CARTESIAN_POINT('Ctrl Pts',(-58.5581604568431,-81.3365913849285,
176.802362616119));
#34662=CARTESIAN_POINT('Ctrl Pts',(-58.6739686579132,-81.3843860597891,
176.02258235797));
#34663=CARTESIAN_POINT('Ctrl Pts',(-58.6570311332583,-81.4170912985052,
175.633298799305));
#34664=CARTESIAN_POINT('Ctrl Pts',(-58.4740495100569,-81.5012613123642,
174.869162393817));
#34665=CARTESIAN_POINT('Ctrl Pts',(-58.3041031171488,-81.5521533857258,
174.503222692046));
#34666=CARTESIAN_POINT('Ctrl Pts',(-57.8398053009967,-81.661797816338,173.873841296063));
#34667=CARTESIAN_POINT('Ctrl Pts',(-57.555169507049,-81.723030541439,173.612840443946));
#34668=CARTESIAN_POINT('Ctrl Pts',(-56.8906673356877,-81.8585310762853,
173.207248459729));
#34669=CARTESIAN_POINT('Ctrl Pts',(-56.5142735001098,-81.9314327519905,
173.071660243962));
#34670=CARTESIAN_POINT('Ctrl Pts',(-55.7453585609871,-82.073558459601,172.961003554594));
#34671=CARTESIAN_POINT('Ctrl Pts',(-55.3615321434295,-82.1453538554173,
172.981020677109));
#34672=CARTESIAN_POINT('Ctrl Pts',(-54.6084266529547,-82.2902971011637,
173.171299416638));
#34673=CARTESIAN_POINT('Ctrl Pts',(-54.2478983250722,-82.3615083960981,
173.345385584072));
#34674=CARTESIAN_POINT('Ctrl Pts',(-53.9183659285772,-82.428624144687,173.596738821088));
#34675=CARTESIAN_POINT('Ctrl Pts',(-53.9048803387418,-82.4313748458465,
173.607211444546));
#34676=CARTESIAN_POINT('Ctrl Pts',(-53.8914893745187,-82.4341103614513,
173.617797875548));
#34677=CARTESIAN_POINT('Ctrl Pts',(-53.9444923767429,-82.9312931062798,
173.617797875548));
#34678=CARTESIAN_POINT('Ctrl Pts',(-53.9535813647071,-82.9294364014157,
173.61061243749));
#34679=CARTESIAN_POINT('Ctrl Pts',(-53.962713998754,-82.9275726898846,173.603479387289));
#34680=CARTESIAN_POINT('Ctrl Pts',(-54.2866912226434,-82.8615253180011,
173.353494400607));
#34681=CARTESIAN_POINT('Ctrl Pts',(-54.6464773768003,-82.7904069684609,
173.177325161358));
#34682=CARTESIAN_POINT('Ctrl Pts',(-55.3989431018931,-82.6454917884509,
172.982881861345));
#34683=CARTESIAN_POINT('Ctrl Pts',(-55.7828158409426,-82.5735306890303,
172.960820018304));
#34684=CARTESIAN_POINT('Ctrl Pts',(-56.5526526269826,-82.431402525919,173.067502330347));
#34685=CARTESIAN_POINT('Ctrl Pts',(-56.929921387865,-82.3584204819804,173.201226930041));
#34686=CARTESIAN_POINT('Ctrl Pts',(-57.5967268363666,-82.2226370702945,
173.603656660308));
#34687=CARTESIAN_POINT('Ctrl Pts',(-57.8827267800039,-82.1611090861183,
173.863353519765));
#34688=CARTESIAN_POINT('Ctrl Pts',(-58.3502350657911,-82.05121161974,174.490722186914));
#34689=CARTESIAN_POINT('Ctrl Pts',(-58.5219772698673,-82.0001401433687,
174.856013155927));
#34690=CARTESIAN_POINT('Ctrl Pts',(-58.7085434103299,-81.9155532742003,
175.619595048659));
#34691=CARTESIAN_POINT('Ctrl Pts',(-58.7272278590927,-81.8825221835531,
176.008933747952));
#34692=CARTESIAN_POINT('Ctrl Pts',(-58.6148524315187,-81.8344446217895,
176.789507706957));
#34693=CARTESIAN_POINT('Ctrl Pts',(-58.4784449131681,-81.8162240236186,
177.172395316719));
#34694=CARTESIAN_POINT('Ctrl Pts',(-58.071491915452,-81.7949100960382,177.849858811396));
#34695=CARTESIAN_POINT('Ctrl Pts',(-57.8099983698264,-81.7917471779939,
178.140782382714));
#34696=CARTESIAN_POINT('Ctrl Pts',(-57.1798525023496,-81.7988678010176,
178.617335843328));
#34697=CARTESIAN_POINT('Ctrl Pts',(-56.8131722829807,-81.8051958661488,
178.793540818343));
#34698=CARTESIAN_POINT('Ctrl Pts',(-56.0470781729116,-81.8221686282478,
178.988055624169));
#34699=CARTESIAN_POINT('Ctrl Pts',(-55.6566607627439,-81.832749229207,179.010152563904));
#34700=CARTESIAN_POINT('Ctrl Pts',(-54.8741472383782,-81.8561136313191,
178.903538452364));
#34701=CARTESIAN_POINT('Ctrl Pts',(-54.4899566546963,-81.8643084693757,
178.769845857466));
#34702=CARTESIAN_POINT('Ctrl Pts',(-53.8094722657113,-81.8721545216685,
178.367470422246));
#34703=CARTESIAN_POINT('Ctrl Pts',(-53.516904933227,-81.8723030682003,178.107795920391));
#34704=CARTESIAN_POINT('Ctrl Pts',(-53.0366807297978,-81.8634417521832,
177.480461813644));
#34705=CARTESIAN_POINT('Ctrl Pts',(-52.8580008943164,-81.8497278190171,
177.115182033494));
#34706=CARTESIAN_POINT('Ctrl Pts',(-52.6577338152889,-81.80637936614,176.351609712819));
#34707=CARTESIAN_POINT('Ctrl Pts',(-52.6324753305221,-81.7780304620221,
175.962270067826));
#34708=CARTESIAN_POINT('Ctrl Pts',(-52.7304634711916,-81.7085331365265,
175.194744828215));
#34709=CARTESIAN_POINT('Ctrl Pts',(-52.853204470837,-81.6638200595933,174.823815050375));
#34710=CARTESIAN_POINT('Ctrl Pts',(-53.2319768749049,-81.5596848723498,
174.151181362769));
#34711=CARTESIAN_POINT('Ctrl Pts',(-53.4843155844065,-81.5012676392086,
173.85589066183));
#34712=CARTESIAN_POINT('Ctrl Pts',(-53.7854833700705,-81.4397448717942,
173.617797875548));
#34713=CARTESIAN_POINT('Origin',(-54.1598171290174,-67.5719248685924,175.985485069079));
#34714=CARTESIAN_POINT('',(-53.5734713611743,-79.4510138924801,173.617797875548));
#34715=CARTESIAN_POINT('',(-53.626474363399,-79.9481966373084,173.617797875547));
#34716=CARTESIAN_POINT('',(-52.327900808713,-67.7672193871761,173.617797875548));
#34717=CARTESIAN_POINT('Ctrl Pts',(-53.5734713611743,-79.4510138924801,
173.617797875548));
#34718=CARTESIAN_POINT('Ctrl Pts',(-53.2839132390089,-79.5101650296565,
173.846712465284));
#34719=CARTESIAN_POINT('Ctrl Pts',(-53.0393481398622,-79.5664744087806,
174.128607631233));
#34720=CARTESIAN_POINT('Ctrl Pts',(-52.6516046998443,-79.6714116962577,
174.793961864577));
#34721=CARTESIAN_POINT('Ctrl Pts',(-52.5214919950192,-79.7180494879704,
175.176560354536));
#34722=CARTESIAN_POINT('Ctrl Pts',(-52.4204754219013,-79.7889078080589,
175.956832618298));
#34723=CARTESIAN_POINT('Ctrl Pts',(-52.4450259653416,-79.8172760758686,
176.346150271794));
#34724=CARTESIAN_POINT('Ctrl Pts',(-52.6438614285247,-79.860763390992,177.109944641201));
#34725=CARTESIAN_POINT('Ctrl Pts',(-52.8218268486073,-79.874558377363,177.475484060112));
#34726=CARTESIAN_POINT('Ctrl Pts',(-53.3007794039409,-79.8835909170627,
178.103621475286));
#34727=CARTESIAN_POINT('Ctrl Pts',(-53.5927901083991,-79.8834414234718,
178.36381593597));
#34728=CARTESIAN_POINT('Ctrl Pts',(-54.2723535909397,-79.8756787511857,
178.767453415344));
#34729=CARTESIAN_POINT('Ctrl Pts',(-54.6561974632848,-79.8675261277388,
178.901889875769));
#34730=CARTESIAN_POINT('Ctrl Pts',(-55.4383526524422,-79.8442382527869,
179.010089588121));
#34731=CARTESIAN_POINT('Ctrl Pts',(-55.8287379663228,-79.8335962998503,
178.988808533618));
#34732=CARTESIAN_POINT('Ctrl Pts',(-56.5950854101889,-79.8165806206824,
178.795955809325));
#34733=CARTESIAN_POINT('Ctrl Pts',(-56.9620644246878,-79.8102263419449,
178.620581746196));
#34734=CARTESIAN_POINT('Ctrl Pts',(-57.5931375642539,-79.8030480581929,
178.145510578597));
#34735=CARTESIAN_POINT('Ctrl Pts',(-57.8552212288729,-79.8060784772914,
177.855226475813));
#34736=CARTESIAN_POINT('Ctrl Pts',(-58.2636224073494,-79.8272209100588,
177.178831445985));
#34737=CARTESIAN_POINT('Ctrl Pts',(-58.4008851895586,-79.8453563861565,
176.796347544831));
#34738=CARTESIAN_POINT('Ctrl Pts',(-58.5150870864485,-79.8932835052345,
176.016194870104));
#34739=CARTESIAN_POINT('Ctrl Pts',(-58.4973321640642,-79.9261407476775,
175.626885529689));
#34740=CARTESIAN_POINT('Ctrl Pts',(-58.3126736753222,-80.0105058501583,
174.863007516469));
#34741=CARTESIAN_POINT('Ctrl Pts',(-58.1418868667774,-80.0614819741624,
174.497370248303));
#34742=CARTESIAN_POINT('Ctrl Pts',(-57.6760867130961,-80.171244919223,173.868929365769));
#34743=CARTESIAN_POINT('Ctrl Pts',(-57.3908129515967,-80.2326151907151,
173.608538322025));
#34744=CARTESIAN_POINT('Ctrl Pts',(-56.7252330417196,-80.3682481674656,
173.204424060083));
#34745=CARTESIAN_POINT('Ctrl Pts',(-56.3484290168544,-80.4411876425926,
173.069706610886));
#34746=CARTESIAN_POINT('Ctrl Pts',(-55.5790818340909,-80.5833147372578,
172.960907698141));
#34747=CARTESIAN_POINT('Ctrl Pts',(-55.195233725635,-80.6551869693247,172.981880472418));
#34748=CARTESIAN_POINT('Ctrl Pts',(-54.4424258627393,-80.8001173490269,
173.174105292471));
#34749=CARTESIAN_POINT('Ctrl Pts',(-54.0822429708766,-80.8712854782209,
173.349165306176));
#34750=CARTESIAN_POINT('Ctrl Pts',(-53.7553099800293,-80.9379014713065,
173.599885811165));
#34751=CARTESIAN_POINT('Ctrl Pts',(-53.7438609810889,-80.9402372872754,
173.608800758175));
#34752=CARTESIAN_POINT('Ctrl Pts',(-53.7324803678465,-80.9425621269657,
173.617797875548));
#34753=CARTESIAN_POINT('Ctrl Pts',(-53.7854833700706,-81.4397448717942,
173.617797875548));
#34754=CARTESIAN_POINT('Ctrl Pts',(-53.9889618015743,-81.3981781544653,
173.456934898128));
#34755=CARTESIAN_POINT('Ctrl Pts',(-54.2123585900196,-81.3534994634441,
173.323874911151));
#34756=CARTESIAN_POINT('Ctrl Pts',(-54.6917335852962,-81.2593823460045,
173.118281881145));
#34757=CARTESIAN_POINT('Ctrl Pts',(-54.9461396249263,-81.2102817144208,
173.047748606547));
#34758=CARTESIAN_POINT('Ctrl Pts',(-55.5874558779449,-81.0884917717835,
172.960269003438));
#34759=CARTESIAN_POINT('Ctrl Pts',(-55.9750991573887,-81.0181626840939,
172.98415968872));
#34760=CARTESIAN_POINT('Ctrl Pts',(-56.7208832908939,-80.8766330037567,
173.181471212417));
#34761=CARTESIAN_POINT('Ctrl Pts',(-57.0716022776453,-80.8068275275108,
173.353704705639));
#34762=CARTESIAN_POINT('Ctrl Pts',(-57.6860825729975,-80.6776159103853,
173.824415648272));
#34763=CARTESIAN_POINT('Ctrl Pts',(-57.9444428979215,-80.62098075888,174.117898114428));
#34764=CARTESIAN_POINT('Ctrl Pts',(-58.3350117146376,-80.5174025421943,
174.790286529534));
#34765=CARTESIAN_POINT('Ctrl Pts',(-58.4629707254976,-80.4713762772148,
175.162936279234));
#34766=CARTESIAN_POINT('Ctrl Pts',(-58.5690745277377,-80.3963014210774,
175.93701510357));
#34767=CARTESIAN_POINT('Ctrl Pts',(-58.546706106472,-80.3695014870016,176.330943217721));
#34768=CARTESIAN_POINT('Ctrl Pts',(-58.3523161121012,-80.3283656642969,
177.089978636783));
#34769=CARTESIAN_POINT('Ctrl Pts',(-58.1818671708559,-80.3141833564527,
177.447651021712));
#34770=CARTESIAN_POINT('Ctrl Pts',(-57.7141277145983,-80.3002271684866,
178.078024798891));
#34771=CARTESIAN_POINT('Ctrl Pts',(-57.4215969455131,-80.3021327782118,
178.34472730544));
#34772=CARTESIAN_POINT('Ctrl Pts',(-56.7505584155294,-80.311891303891,178.751512130253));
#34773=CARTESIAN_POINT('Ctrl Pts',(-56.3784811663972,-80.3192356354569,
178.887589492959));
#34774=CARTESIAN_POINT('Ctrl Pts',(-55.6030346372377,-80.3380289180745,
179.009816582222));
#34775=CARTESIAN_POINT('Ctrl Pts',(-55.2072753458979,-80.3508412085372,
178.994676671652));
#34776=CARTESIAN_POINT('Ctrl Pts',(-54.4437534306365,-80.370537894246,178.81366465606));
#34777=CARTESIAN_POINT('Ctrl Pts',(-54.0833029169573,-80.376674369447,178.649699500036));
#34778=CARTESIAN_POINT('Ctrl Pts',(-53.4444712725212,-80.380852101205,178.192798229079));
#34779=CARTESIAN_POINT('Ctrl Pts',(-53.1725998370387,-80.3803569578552,
177.903982650869));
#34780=CARTESIAN_POINT('Ctrl Pts',(-52.7546772649625,-80.3632874874759,
177.239578072511));
#34781=CARTESIAN_POINT('Ctrl Pts',(-52.6122887632239,-80.3462085271098,
176.870632974855));
#34782=CARTESIAN_POINT('Ctrl Pts',(-52.4758197014113,-80.2967821838551,
176.098561826864));
#34783=CARTESIAN_POINT('Ctrl Pts',(-52.4837668759432,-80.2663549462667,
175.702774135099));
#34784=CARTESIAN_POINT('Ctrl Pts',(-52.6498828822117,-80.187098197252,174.939374482983));
#34785=CARTESIAN_POINT('Ctrl Pts',(-52.8057763387706,-80.1382515106677,
174.579036605884));
#34786=CARTESIAN_POINT('Ctrl Pts',(-53.1935668659987,-80.0406506942216,
174.016094875201));
#34787=CARTESIAN_POINT('Ctrl Pts',(-53.3960518932188,-79.995267501839,173.799961873686));
#34788=CARTESIAN_POINT('Ctrl Pts',(-53.6264743633996,-79.9481966373083,
173.617797875547));
#34789=CARTESIAN_POINT('Origin',(-54.1598171290174,-67.5719248685924,175.985485069079));
#34790=CARTESIAN_POINT('',(-53.4144623545021,-77.9594656579945,173.617797875548));
#34791=CARTESIAN_POINT('',(-53.4674653567265,-78.4566484028229,173.617797875548));
#34792=CARTESIAN_POINT('',(-52.327900808713,-67.7672193871761,173.617797875548));
#34793=CARTESIAN_POINT('Ctrl Pts',(-53.4144623545021,-77.9594656579945,
173.617797875548));
#34794=CARTESIAN_POINT('Ctrl Pts',(-53.1242371104778,-78.0187530752943,
173.847239868644));
#34795=CARTESIAN_POINT('Ctrl Pts',(-52.8792207699447,-78.075183965081,174.129900821861));
#34796=CARTESIAN_POINT('Ctrl Pts',(-52.4915960091567,-78.1801824835191,
174.796353277051));
#34797=CARTESIAN_POINT('Ctrl Pts',(-52.3618006095129,-78.2267842006455,
175.179101795173));
#34798=CARTESIAN_POINT('Ctrl Pts',(-52.2614592207656,-78.2975540938532,
175.959530619911));
#34799=CARTESIAN_POINT('Ctrl Pts',(-52.286360995377,-78.3259126820135,176.348859181655));
#34800=CARTESIAN_POINT('Ctrl Pts',(-52.4859067048768,-78.3693311182812,
177.112543551467));
#34801=CARTESIAN_POINT('Ctrl Pts',(-52.6642266105073,-78.3830859016589,
177.47795432728));
#34802=CARTESIAN_POINT('Ctrl Pts',(-53.1438101229382,-78.3920335019309,
178.1056933791));
#34803=CARTESIAN_POINT('Ctrl Pts',(-53.4360969282526,-78.3918843945314,
178.365629915207));
#34804=CARTESIAN_POINT('Ctrl Pts',(-54.1161173271656,-78.384080365151,178.76864153432));
#34805=CARTESIAN_POINT('Ctrl Pts',(-54.5001333540368,-78.3759068000259,
178.902709120172));
#34806=CARTESIAN_POINT('Ctrl Pts',(-55.282466481728,-78.352580962601,179.010122429603));
#34807=CARTESIAN_POINT('Ctrl Pts',(-55.6728676995625,-78.341969340023,178.988436745572));
#34808=CARTESIAN_POINT('Ctrl Pts',(-56.43908973001,-78.3249749377774,178.794759781836));
#34809=CARTESIAN_POINT('Ctrl Pts',(-56.8059207939449,-78.3186336538946,
178.618973592585));
#34810=CARTESIAN_POINT('Ctrl Pts',(-57.4365343189338,-78.3114839603943,
178.143167246289));
#34811=CARTESIAN_POINT('Ctrl Pts',(-57.6983253719169,-78.3145799643806,
177.852566080781));
#34812=CARTESIAN_POINT('Ctrl Pts',(-58.1060087301422,-78.3358074239231,
177.175641136799));
#34813=CARTESIAN_POINT('Ctrl Pts',(-58.2428476053164,-78.3539851116537,
176.792956839626));
#34814=CARTESIAN_POINT('Ctrl Pts',(-58.3561440580827,-78.4019868309526,
176.012595030349));
#34815=CARTESIAN_POINT('Ctrl Pts',(-58.3379283501955,-78.4349301216162,
175.623271141334));
#34816=CARTESIAN_POINT('Ctrl Pts',(-58.1523242988494,-78.5194051697063,
174.859539617395));
#34817=CARTESIAN_POINT('Ctrl Pts',(-57.9810638392148,-78.5704285923116,
174.494073700727));
#34818=CARTESIAN_POINT('Ctrl Pts',(-57.5144168893062,-78.6802582557992,
173.866163980835));
#34819=CARTESIAN_POINT('Ctrl Pts',(-57.2287832373442,-78.741706536025,173.606116962053));
#34820=CARTESIAN_POINT('Ctrl Pts',(-56.5625957961499,-78.8774141099415,
173.202837211976));
#34821=CARTESIAN_POINT('Ctrl Pts',(-56.1855611619529,-78.9503747427818,
173.068611589101));
#34822=CARTESIAN_POINT('Ctrl Pts',(-55.4159710145938,-79.0925024349185,
172.960861390174));
#34823=CARTESIAN_POINT('Ctrl Pts',(-55.0321106912169,-79.1644185217348,
172.982373728683));
#34824=CARTESIAN_POINT('Ctrl Pts',(-54.2794719416634,-79.3093414425798,
173.175697571081));
#34825=CARTESIAN_POINT('Ctrl Pts',(-53.9194851988895,-79.3804849873277,
173.35130721382));
#34826=CARTESIAN_POINT('Ctrl Pts',(-53.5940174791467,-79.4468191431629,
173.601665238008));
#34827=CARTESIAN_POINT('Ctrl Pts',(-53.5837166999884,-79.4489209674498,
173.609698266689));
#34828=CARTESIAN_POINT('Ctrl Pts',(-53.5734713611743,-79.4510138924801,
173.617797875548));
#34829=CARTESIAN_POINT('Ctrl Pts',(-53.6264743633996,-79.9481966373083,
173.617797875547));
#34830=CARTESIAN_POINT('Ctrl Pts',(-53.6999737117029,-79.93318213866,173.559691844755));
#34831=CARTESIAN_POINT('Ctrl Pts',(-53.776270499172,-79.9177210304295,173.50505611858));
#34832=CARTESIAN_POINT('Ctrl Pts',(-54.1795502188484,-79.8366199055185,
173.244539735607));
#34833=CARTESIAN_POINT('Ctrl Pts',(-54.5413081342879,-79.7658574063917,
173.101336271712));
#34834=CARTESIAN_POINT('Ctrl Pts',(-55.3013069703931,-79.6207715002734,
172.963199457707));
#34835=CARTESIAN_POINT('Ctrl Pts',(-55.6925578511268,-79.5492764327622,
172.970579437118));
#34836=CARTESIAN_POINT('Ctrl Pts',(-56.4470856128977,-79.4074351507114,
173.137245239642));
#34837=CARTESIAN_POINT('Ctrl Pts',(-56.8031387705855,-79.3373110297835,
173.293926614045));
#34838=CARTESIAN_POINT('Ctrl Pts',(-57.4378982890236,-79.2055351033221,
173.738598285689));
#34839=CARTESIAN_POINT('Ctrl Pts',(-57.7099586638791,-79.1466440388984,
174.023299217339));
#34840=CARTESIAN_POINT('Ctrl Pts',(-58.1273347811811,-79.0408141444312,
174.680630840406));
#34841=CARTESIAN_POINT('Ctrl Pts',(-58.2694808619301,-78.9935235758121,
175.046227733694));
#34842=CARTESIAN_POINT('Ctrl Pts',(-58.4071426369151,-78.9147025687063,
175.816384421502));
#34843=CARTESIAN_POINT('Ctrl Pts',(-58.4000992516212,-78.8854639848545,
176.213783222893));
#34844=CARTESIAN_POINT('Ctrl Pts',(-58.2342698188388,-78.8418741891221,
176.980833984601));
#34845=CARTESIAN_POINT('Ctrl Pts',(-58.0783142710071,-78.8263922169384,
177.343338609313));
#34846=CARTESIAN_POINT('Ctrl Pts',(-57.634822831167,-78.8094892647114,177.992661649254));
#34847=CARTESIAN_POINT('Ctrl Pts',(-57.3503804359288,-78.809722498661,178.272316899594));
#34848=CARTESIAN_POINT('Ctrl Pts',(-56.693447818481,-78.8185517444044,178.70406324853));
#34849=CARTESIAN_POINT('Ctrl Pts',(-56.3280374921874,-78.8254273005829,
178.853306571911));
#34850=CARTESIAN_POINT('Ctrl Pts',(-55.5563426567283,-78.8434784329005,
179.005080249419));
#34851=CARTESIAN_POINT('Ctrl Pts',(-55.1572953278909,-78.8558300002763,
179.004377698217));
#34852=CARTESIAN_POINT('Ctrl Pts',(-54.3865591713871,-78.8768532596877,
178.849971682348));
#34853=CARTESIAN_POINT('Ctrl Pts',(-54.0218103706171,-78.8836857661521,
178.699515970368));
#34854=CARTESIAN_POINT('Ctrl Pts',(-53.3655931673347,-78.8893936985532,
178.265350298767));
#34855=CARTESIAN_POINT('Ctrl Pts',(-53.0816890567742,-78.8893726976383,
177.984174318144));
#34856=CARTESIAN_POINT('Ctrl Pts',(-52.6354814370726,-78.8751014359724,
177.324848622603));
#34857=CARTESIAN_POINT('Ctrl Pts',(-52.4789479421949,-78.8589289835916,
176.952204682775));
#34858=CARTESIAN_POINT('Ctrl Pts',(-52.3227023685931,-78.8113571019577,
176.182393342189));
#34859=CARTESIAN_POINT('Ctrl Pts',(-52.3192666697951,-78.7821382059785,
175.79371741212));
#34860=CARTESIAN_POINT('Ctrl Pts',(-52.4610116599005,-78.7059885439742,
175.023485227097));
#34861=CARTESIAN_POINT('Ctrl Pts',(-52.6100980541892,-78.6572377292065,
174.650472971694));
#34862=CARTESIAN_POINT('Ctrl Pts',(-53.0021555360266,-78.5564000261094,
174.051172062114));
#34863=CARTESIAN_POINT('Ctrl Pts',(-53.2183638889226,-78.5075350261465,
173.814728840144));
#34864=CARTESIAN_POINT('Ctrl Pts',(-53.4674653567269,-78.4566484028228,
173.617797875547));
#34865=CARTESIAN_POINT('Origin',(-54.1598171290174,-67.5719248685924,175.985485069079));
#34866=CARTESIAN_POINT('',(-53.2554533478299,-76.4679174235089,173.617797875548));
#34867=CARTESIAN_POINT('',(-53.308456350054,-76.9651001683374,173.617797875548));
#34868=CARTESIAN_POINT('',(-52.327900808713,-67.7672193871761,173.617797875548));
#34869=CARTESIAN_POINT('Ctrl Pts',(-53.2554533478299,-76.4679174235089,
173.617797875548));
#34870=CARTESIAN_POINT('Ctrl Pts',(-52.964854160848,-76.5272812301394,173.847535494952));
#34871=CARTESIAN_POINT('Ctrl Pts',(-52.7195851171509,-76.5837802128976,
174.130625928072));
#34872=CARTESIAN_POINT('Ctrl Pts',(-52.3320275568318,-76.6888129616136,
174.79769408723));
#34873=CARTESIAN_POINT('Ctrl Pts',(-52.2024100784284,-76.7353944404665,
175.180526586134));
#34874=CARTESIAN_POINT('Ctrl Pts',(-52.1024472067462,-76.8061147504361,
175.961043041675));
#34875=CARTESIAN_POINT('Ctrl Pts',(-52.1275459070151,-76.8344679741608,
176.350377721454));
#34876=CARTESIAN_POINT('Ctrl Pts',(-52.3274898508707,-76.8778477790918,
177.114000274915));
#34877=CARTESIAN_POINT('Ctrl Pts',(-52.5060084703274,-76.8915800131688,
177.479338776243));
#34878=CARTESIAN_POINT('Ctrl Pts',(-52.9859456966574,-76.9004799817596,
178.106854319571));
#34879=CARTESIAN_POINT('Ctrl Pts',(-53.27838735513,-76.9003311629783,178.366646207626));
#34880=CARTESIAN_POINT('Ctrl Pts',(-53.9586639114936,-76.8925039369739,
178.769306684473));
#34881=CARTESIAN_POINT('Ctrl Pts',(-54.342776339663,-76.8843186284663,178.90316729765));
#34882=CARTESIAN_POINT('Ctrl Pts',(-55.1252090968815,-76.8609715022402,
179.010139467056));
#34883=CARTESIAN_POINT('Ctrl Pts',(-55.5156192488589,-76.8503769782809,
178.988226784107));
#34884=CARTESIAN_POINT('Ctrl Pts',(-56.2817707281885,-76.8333945188046,
178.794087373533));
#34885=CARTESIAN_POINT('Ctrl Pts',(-56.6485185898549,-76.8270605298348,
178.618070017813));
#34886=CARTESIAN_POINT('Ctrl Pts',(-57.278874048408,-76.8199268807342,178.141851277279));
#34887=CARTESIAN_POINT('Ctrl Pts',(-57.5405009006074,-76.8230597871527,
177.85107217373));
#34888=CARTESIAN_POINT('Ctrl Pts',(-57.9477812230071,-76.8443349679731,
177.173849963172));
#34889=CARTESIAN_POINT('Ctrl Pts',(-58.0843820674067,-76.8625363398498,
176.791053398886));
#34890=CARTESIAN_POINT('Ctrl Pts',(-58.1971702400539,-76.9105799190036,
176.010574439175));
#34891=CARTESIAN_POINT('Ctrl Pts',(-58.1786958545423,-76.9435716294713,
175.621242378299));
#34892=CARTESIAN_POINT('Ctrl Pts',(-57.9925608932288,-77.028108389584,174.857593352838));
#34893=CARTESIAN_POINT('Ctrl Pts',(-57.8210345692386,-77.0791583386423,
174.492223902628));
#34894=CARTESIAN_POINT('Ctrl Pts',(-57.353912275556,-77.189025428004,173.864612676414));
#34895=CARTESIAN_POINT('Ctrl Pts',(-57.0680765066293,-77.2505176499002,
173.604758870934));
#34896=CARTESIAN_POINT('Ctrl Pts',(-56.4015480124462,-77.3862670812936,
173.201948072434));
#34897=CARTESIAN_POINT('Ctrl Pts',(-56.0243841159366,-77.4592395439619,
173.067998854454));
#34898=CARTESIAN_POINT('Ctrl Pts',(-55.2546577944142,-77.6013675130901,
172.960837842604));
#34899=CARTESIAN_POINT('Ctrl Pts',(-54.8707906180679,-77.6733083903765,
172.982653350642));
#34900=CARTESIAN_POINT('Ctrl Pts',(-54.1182472292829,-77.8182270585414,
173.176594790565));
#34901=CARTESIAN_POINT('Ctrl Pts',(-53.7583710511103,-77.8893567224248,
173.352513190678));
#34902=CARTESIAN_POINT('Ctrl Pts',(-53.4337258810389,-77.9555326246257,
173.602665888411));
#34903=CARTESIAN_POINT('Ctrl Pts',(-53.4240697378998,-77.957503054946,173.610202612074));
#34904=CARTESIAN_POINT('Ctrl Pts',(-53.4144623545021,-77.9594656579945,
173.617797875548));
#34905=CARTESIAN_POINT('Ctrl Pts',(-53.4674653567269,-78.4566484028228,
173.617797875547));
#34906=CARTESIAN_POINT('Ctrl Pts',(-53.5168179472732,-78.4465666208594,
173.578781432379));
#34907=CARTESIAN_POINT('Ctrl Pts',(-53.5674413657633,-78.4362815284313,
173.541322215379));
#34908=CARTESIAN_POINT('Ctrl Pts',(-53.9444328009459,-78.3600907305088,
173.280660874177));
#34909=CARTESIAN_POINT('Ctrl Pts',(-54.3107257198566,-78.2881872354447,
173.12410691606));
#34910=CARTESIAN_POINT('Ctrl Pts',(-55.0687611470599,-78.1430871762328,
172.968625444015));
#34911=CARTESIAN_POINT('Ctrl Pts',(-55.4521889847661,-78.0724852575809,
172.965753553128));
#34912=CARTESIAN_POINT('Ctrl Pts',(-56.2129318446134,-77.9304568434933,
173.109795658303));
#34913=CARTESIAN_POINT('Ctrl Pts',(-56.5815908099749,-77.8583042744884,
173.260915312004));
#34914=CARTESIAN_POINT('Ctrl Pts',(-57.2263953545785,-77.7252481987439,
173.692932254402));
#34915=CARTESIAN_POINT('Ctrl Pts',(-57.4994685573361,-77.6663430468716,
173.964981012495));
#34916=CARTESIAN_POINT('Ctrl Pts',(-57.9362689244949,-77.5589005834618,
174.611163636346));
#34917=CARTESIAN_POINT('Ctrl Pts',(-58.0908197218222,-77.5095766684115,
174.982285367976));
#34918=CARTESIAN_POINT('Ctrl Pts',(-58.2432661406676,-77.4289837410822,
175.75081726355));
#34919=CARTESIAN_POINT('Ctrl Pts',(-58.2452594066001,-77.3989117255198,
176.13963758963));
#34920=CARTESIAN_POINT('Ctrl Pts',(-58.1000707945399,-77.3535622345091,
176.912286950257));
#34921=CARTESIAN_POINT('Ctrl Pts',(-57.9483988300908,-77.3368870941246,
177.287600354543));
#34922=CARTESIAN_POINT('Ctrl Pts',(-57.515542273888,-77.318667441005,177.945575933969));
#34923=CARTESIAN_POINT('Ctrl Pts',(-57.2433564915632,-77.3177610601279,
178.224939813528));
#34924=CARTESIAN_POINT('Ctrl Pts',(-56.5966376496724,-77.3259246927055,
178.674424369112));
#34925=CARTESIAN_POINT('Ctrl Pts',(-56.2248079189572,-77.3327232769949,
178.835441600731));
#34926=CARTESIAN_POINT('Ctrl Pts',(-55.454377979819,-77.3504687699554,178.999741818441));
#34927=CARTESIAN_POINT('Ctrl Pts',(-55.0645262168849,-77.3620449013272,
179.006970374376));
#34928=CARTESIAN_POINT('Ctrl Pts',(-54.2888274410951,-77.384002955326,178.871418979044));
#34929=CARTESIAN_POINT('Ctrl Pts',(-53.9112133437184,-77.3914216495637,
178.72422716204));
#34930=CARTESIAN_POINT('Ctrl Pts',(-53.2477613019418,-77.3977415730732,
178.29890725331));
#34931=CARTESIAN_POINT('Ctrl Pts',(-52.9653954550316,-77.3977998128993,
178.029685296235));
#34932=CARTESIAN_POINT('Ctrl Pts',(-52.5087154904175,-77.3857903409056,
177.38775671557));
#34933=CARTESIAN_POINT('Ctrl Pts',(-52.3432748923029,-77.3705933748417,
177.01790606498));
#34934=CARTESIAN_POINT('Ctrl Pts',(-52.1694074351774,-77.3247006426295,
176.250446686407));
#34935=CARTESIAN_POINT('Ctrl Pts',(-52.1572205391053,-77.2958991705948,
175.861508827493));
#34936=CARTESIAN_POINT('Ctrl Pts',(-52.2820566190224,-77.2219359945378,
175.086965003283));
#34937=CARTESIAN_POINT('Ctrl Pts',(-52.4233078023374,-77.1740470586507,
174.70984491892));
#34938=CARTESIAN_POINT('Ctrl Pts',(-52.8142567922122,-77.0714107626084,
174.083178867424));
#34939=CARTESIAN_POINT('Ctrl Pts',(-53.0425095453552,-77.0194279689487,
173.828046178147));
#34940=CARTESIAN_POINT('Ctrl Pts',(-53.3084563500542,-76.9651001683373,
173.617797875548));
#34941=CARTESIAN_POINT('Origin',(-54.1598171290174,-67.5719248685924,175.985485069079));
#34942=CARTESIAN_POINT('',(-53.0964443411576,-74.9763691890233,173.617797875548));
#34943=CARTESIAN_POINT('',(-53.1494473433817,-75.4735519338518,173.617797875548));
#34944=CARTESIAN_POINT('',(-52.327900808713,-67.7672193871761,173.617797875548));
#34945=CARTESIAN_POINT('Ctrl Pts',(-53.0964443411576,-74.9763691890233,
173.617797875548));
#34946=CARTESIAN_POINT('Ctrl Pts',(-52.8056358972556,-75.0357757428049,
173.847700926202));
#34947=CARTESIAN_POINT('Ctrl Pts',(-52.5602255146313,-75.0923128245866,
174.131031767172));
#34948=CARTESIAN_POINT('Ctrl Pts',(-52.1727057716636,-75.1973646996916,
174.798444507892));
#34949=CARTESIAN_POINT('Ctrl Pts',(-52.0431878765506,-75.2439348478614,
175.181323966111));
#34950=CARTESIAN_POINT('Ctrl Pts',(-51.9434368386618,-75.3146274058711,
175.96188941981));
#34951=CARTESIAN_POINT('Ctrl Pts',(-51.9686457532674,-75.3429776468977,
176.351227524336));
#34952=CARTESIAN_POINT('Ctrl Pts',(-52.1688125846985,-75.3863358268145,
177.114815436015));
#34953=CARTESIAN_POINT('Ctrl Pts',(-52.3474424077776,-75.4000554379297,
177.480113440793));
#34954=CARTESIAN_POINT('Ctrl Pts',(-52.8275775842746,-75.4089287456145,
178.107503842801));
#34955=CARTESIAN_POINT('Ctrl Pts',(-53.1201059261585,-75.4087801109735,
178.367214763405));
#34956=CARTESIAN_POINT('Ctrl Pts',(-53.8005258401282,-75.4009398996325,
178.769678639605));
#34957=CARTESIAN_POINT('Ctrl Pts',(-54.1846921836614,-75.3927480180389,
178.903423366868));
#34958=CARTESIAN_POINT('Ctrl Pts',(-54.9671806584076,-75.3693889756646,
179.010148570594));
#34959=CARTESIAN_POINT('Ctrl Pts',(-55.3575958159887,-75.3588040506301,
178.988108799899));
#34960=CARTESIAN_POINT('Ctrl Pts',(-56.1237077357375,-75.3418282794223,
178.793710469574));
#34961=CARTESIAN_POINT('Ctrl Pts',(-56.4904089525644,-75.3354983760722,
178.617563704924));
#34962=CARTESIAN_POINT('Ctrl Pts',(-57.1206198606809,-75.3283737112098,
178.141114095079));
#34963=CARTESIAN_POINT('Ctrl Pts',(-57.3821547693695,-75.3315273120711,
177.850235350799));
#34964=CARTESIAN_POINT('Ctrl Pts',(-57.789209342569,-75.3528292167029,177.172846718022));
#34965=CARTESIAN_POINT('Ctrl Pts',(-57.9256768548506,-75.3710438494031,
176.789987348856));
#34966=CARTESIAN_POINT('Ctrl Pts',(-58.0381803604521,-75.4191108669956,
176.009442856234));
#34967=CARTESIAN_POINT('Ctrl Pts',(-58.0195610965447,-75.4521297317918,
175.620106217133));
#34968=CARTESIAN_POINT('Ctrl Pts',(-57.833128759881,-75.536701052086,174.856503479113));
#34969=CARTESIAN_POINT('Ctrl Pts',(-57.6614535438247,-75.5877658496395,
174.491188142736));
#34970=CARTESIAN_POINT('Ctrl Pts',(-57.1940650337145,-75.6976538911716,
173.863744191349));
#34971=CARTESIAN_POINT('Ctrl Pts',(-56.9081160393018,-75.7591707703788,
173.603998625641));
#34972=CARTESIAN_POINT('Ctrl Pts',(-56.2413965323488,-75.8949436386513,
173.201450622004));
#34973=CARTESIAN_POINT('Ctrl Pts',(-55.8641603018969,-75.9679227118515,
173.067656305598));
#34974=CARTESIAN_POINT('Ctrl Pts',(-55.0943577828536,-76.1100508177383,
172.960825424802));
#34975=CARTESIAN_POINT('Ctrl Pts',(-54.7104867697401,-76.1820056333181,
172.982810813907));
#34976=CARTESIAN_POINT('Ctrl Pts',(-53.957996923227,-76.3269218990717,173.177098349728));
#34977=CARTESIAN_POINT('Ctrl Pts',(-53.5981828107927,-76.3980437636204,
173.353189740603));
#34978=CARTESIAN_POINT('Ctrl Pts',(-53.273998317967,-76.4641310215298,173.603226863128));
#34979=CARTESIAN_POINT('Ctrl Pts',(-53.2647032314016,-76.4660278507767,
173.610485239014));
#34980=CARTESIAN_POINT('Ctrl Pts',(-53.2554533478299,-76.4679174235089,
173.617797875548));
#34981=CARTESIAN_POINT('Ctrl Pts',(-53.3084563500542,-76.9651001683373,
173.617797875548));
#34982=CARTESIAN_POINT('Ctrl Pts',(-53.3414229337293,-76.9583657314007,
173.591735640026));
#34983=CARTESIAN_POINT('Ctrl Pts',(-53.3749596317192,-76.9515399503452,
173.56636582625));
#34984=CARTESIAN_POINT('Ctrl Pts',(-53.7301077748267,-76.8795145806819,
173.309469127448));
#34985=CARTESIAN_POINT('Ctrl Pts',(-54.0938718360162,-76.8079076592926,
173.144901510774));
#34986=CARTESIAN_POINT('Ctrl Pts',(-54.8497531287336,-76.6628618909532,
172.973567856788));
#34987=CARTESIAN_POINT('Ctrl Pts',(-55.2333647594788,-76.5917591200613,
172.962870625489));
#34988=CARTESIAN_POINT('Ctrl Pts',(-55.9979356555131,-76.449669159368,173.091664639894));
#34989=CARTESIAN_POINT('Ctrl Pts',(-56.370212759963,-76.3771579986217,173.235719256923));
#34990=CARTESIAN_POINT('Ctrl Pts',(-57.0240915397078,-76.2429702970415,
173.655697855252));
#34991=CARTESIAN_POINT('Ctrl Pts',(-57.3024693488843,-76.1830364554036,
173.922678738022));
#34992=CARTESIAN_POINT('Ctrl Pts',(-57.7519471011078,-76.0745711136206,
174.561212200496));
#34993=CARTESIAN_POINT('Ctrl Pts',(-57.9135980924168,-76.0245173319119,
174.930027958775));
#34994=CARTESIAN_POINT('Ctrl Pts',(-58.0800856430789,-75.9422737661782,
175.696611382092));
#34995=CARTESIAN_POINT('Ctrl Pts',(-58.0889656779772,-75.9110228409928,
176.085642999832));
#34996=CARTESIAN_POINT('Ctrl Pts',(-57.9573177126399,-75.8645410572794,
176.861654377664));
#34997=CARTESIAN_POINT('Ctrl Pts',(-57.811917941177,-75.8472240756098,177.240175824889));
#34998=CARTESIAN_POINT('Ctrl Pts',(-57.3897215767072,-75.827724116012,177.906268510214));
#34999=CARTESIAN_POINT('Ctrl Pts',(-57.1219721450795,-75.8259187101642,
178.190421383545));
#35000=CARTESIAN_POINT('Ctrl Pts',(-56.4820695582827,-75.8336501094147,
178.651189752466));
#35001=CARTESIAN_POINT('Ctrl Pts',(-56.1123076095985,-75.8402546725227,
178.818540918871));
#35002=CARTESIAN_POINT('Ctrl Pts',(-55.3436109484019,-75.8576808596364,
178.995400987715));
#35003=CARTESIAN_POINT('Ctrl Pts',(-54.9535288706714,-75.8688741717095,
179.0088202237));
#35004=CARTESIAN_POINT('Ctrl Pts',(-54.1749194025281,-75.8914207477598,
178.885326689875));
#35005=CARTESIAN_POINT('Ctrl Pts',(-53.7945009370796,-75.8991642982313,
178.743739561927));
#35006=CARTESIAN_POINT('Ctrl Pts',(-53.1238935414248,-75.9061212888656,
178.327957775593));
#35007=CARTESIAN_POINT('Ctrl Pts',(-52.8372655166408,-75.9062451634505,
178.062729660632));
#35008=CARTESIAN_POINT('Ctrl Pts',(-52.3706877393788,-75.8955535058313,
177.426865015712));
#35009=CARTESIAN_POINT('Ctrl Pts',(-52.1996788877483,-75.8809754128322,
177.058875146964));
#35010=CARTESIAN_POINT('Ctrl Pts',(-52.0147405618912,-75.8361454299697,
176.292992512181));
#35011=CARTESIAN_POINT('Ctrl Pts',(-51.9970672433361,-75.8075585443191,
175.903887271424));
#35012=CARTESIAN_POINT('Ctrl Pts',(-52.1081627696099,-75.7369779784704,
175.148234780903));
#35013=CARTESIAN_POINT('Ctrl Pts',(-52.2331062331624,-75.6927206684859,
174.788194676274));
#35014=CARTESIAN_POINT('Ctrl Pts',(-52.6089003750333,-75.5904952622481,
174.13606474324));
#35015=CARTESIAN_POINT('Ctrl Pts',(-52.8560409607083,-75.5334891963958,
173.849754766321));
#35016=CARTESIAN_POINT('Ctrl Pts',(-53.1494473433817,-75.4735519338518,
173.617797875548));
#35017=CARTESIAN_POINT('Origin',(-54.1598171290174,-67.5719248685924,175.985485069079));
#35018=CARTESIAN_POINT('',(-52.9374353344854,-73.4848209545377,173.617797875548));
#35019=CARTESIAN_POINT('',(-52.9904383367094,-73.9820036993662,173.617797875548));
#35020=CARTESIAN_POINT('',(-52.327900808713,-67.7672193871761,173.617797875548));
#35021=CARTESIAN_POINT('Ctrl Pts',(-52.9374353344854,-73.4848209545377,
173.617797875548));
#35022=CARTESIAN_POINT('Ctrl Pts',(-52.6465099007733,-73.5442514070801,
173.847793414281));
#35023=CARTESIAN_POINT('Ctrl Pts',(-52.4010205221672,-73.6008097872557,
174.131258683427));
#35024=CARTESIAN_POINT('Ctrl Pts',(-52.0135219882289,-73.705872346413,174.798864081555));
#35025=CARTESIAN_POINT('Ctrl Pts',(-51.8840597734408,-73.7524361582106,
175.181769782186));
#35026=CARTESIAN_POINT('Ctrl Pts',(-51.7844271714147,-73.8231131991743,
175.962362617006));
#35027=CARTESIAN_POINT('Ctrl Pts',(-51.8096977087126,-73.8514617786658,
176.351702636564));
#35028=CARTESIAN_POINT('Ctrl Pts',(-52.0099891621526,-73.8948078664141,
177.115271165447));
#35029=CARTESIAN_POINT('Ctrl Pts',(-52.1886811574383,-73.9085204189799,
177.480546513429));
#35030=CARTESIAN_POINT('Ctrl Pts',(-52.6689270066302,-73.9173788192747,
178.107866931419));
#35031=CARTESIAN_POINT('Ctrl Pts',(-52.9615038196731,-73.9172302946619,
178.367532578133));
#35032=CARTESIAN_POINT('Ctrl Pts',(-53.642003885008,-73.9093828221344,178.769886508089));
#35033=CARTESIAN_POINT('Ctrl Pts',(-54.0262003616248,-73.9011872652275,
178.903566426416));
#35034=CARTESIAN_POINT('Ctrl Pts',(-54.8087199756404,-73.8778215599148,
179.010153525356));
#35035=CARTESIAN_POINT('Ctrl Pts',(-55.1991379336217,-73.8672420109574,
178.988042684565));
#35036=CARTESIAN_POINT('Ctrl Pts',(-55.9652277118067,-73.850269980588,178.793499556595));
#35037=CARTESIAN_POINT('Ctrl Pts',(-56.3319028241094,-73.8439423624653,
178.617280427587));
#35038=CARTESIAN_POINT('Ctrl Pts',(-56.9620328749772,-73.8368227222785,
178.140701715233));
#35039=CARTESIAN_POINT('Ctrl Pts',(-57.223516362575,-73.8399879066131,177.849767243461));
#35040=CARTESIAN_POINT('Ctrl Pts',(-57.6304446591832,-73.8613047578019,
177.17228554571));
#35041=CARTESIAN_POINT('Ctrl Pts',(-57.7668375880929,-73.8795268065409,
176.789391070126));
#35042=CARTESIAN_POINT('Ctrl Pts',(-57.8791818703731,-73.9276069322545,
176.008809947372));
#35043=CARTESIAN_POINT('Ctrl Pts',(-57.8604815702442,-73.9606409967141,
175.619470747061));
#35044=CARTESIAN_POINT('Ctrl Pts',(-57.673882891374,-74.0452316469215,174.855893925201));
#35045=CARTESIAN_POINT('Ctrl Pts',(-57.5021243977001,-74.0963047472366,
174.490608883617));
#35046=CARTESIAN_POINT('Ctrl Pts',(-57.0345869856321,-74.2062045053082,
173.863258525876));
#35047=CARTESIAN_POINT('Ctrl Pts',(-56.748574651833,-74.2677351909695,173.603573511167));
#35048=CARTESIAN_POINT('Ctrl Pts',(-56.0817483044874,-74.4035211664158,
173.201172545343));
#35049=CARTESIAN_POINT('Ctrl Pts',(-55.7044716343725,-74.4765039324346,
173.067464901129));
#35050=CARTESIAN_POINT('Ctrl Pts',(-54.934626516975,-74.6186321090574,172.960818720527));
#35051=CARTESIAN_POINT('Ctrl Pts',(-54.5507533582519,-74.6905947377381,
172.982899157147));
#35052=CARTESIAN_POINT('Ctrl Pts',(-53.7982935018327,-74.8355096532683,
173.177380339521));
#35053=CARTESIAN_POINT('Ctrl Pts',(-53.4385141495588,-74.9066271474933,
173.353568511));
#35054=CARTESIAN_POINT('Ctrl Pts',(-53.1145873281588,-74.9726648198379,
173.603540806818));
#35055=CARTESIAN_POINT('Ctrl Pts',(-53.105494198882,-74.9745204777121,173.610643372498));
#35056=CARTESIAN_POINT('Ctrl Pts',(-53.0964443411576,-74.9763691890233,
173.617797875548));
#35057=CARTESIAN_POINT('Ctrl Pts',(-53.1494473433817,-75.4735519338518,
173.617797875548));
#35058=CARTESIAN_POINT('Ctrl Pts',(-53.4038504347735,-75.4215822911269,
173.416675631565));
#35059=CARTESIAN_POINT('Ctrl Pts',(-53.6890542096037,-75.3648165529217,
173.259278878347));
#35060=CARTESIAN_POINT('Ctrl Pts',(-54.3016794488769,-75.2455619498074,
173.043135222439));
#35061=CARTESIAN_POINT('Ctrl Pts',(-54.6254322052276,-75.1838147802994,
172.986935943668));
#35062=CARTESIAN_POINT('Ctrl Pts',(-55.3316413974426,-75.0517503870613,
172.983856638115));
#35063=CARTESIAN_POINT('Ctrl Pts',(-55.7083574319068,-74.9829291078777,
173.0563943681));
#35064=CARTESIAN_POINT('Ctrl Pts',(-56.4238106814297,-74.8430437902404,
173.34623381907));
#35065=CARTESIAN_POINT('Ctrl Pts',(-56.7541499010389,-74.7749851769342,
173.564937836107));
#35066=CARTESIAN_POINT('Ctrl Pts',(-57.3030913686338,-74.6543682606874,
174.112287546155));
#35067=CARTESIAN_POINT('Ctrl Pts',(-57.5195038293576,-74.6026874586522,
174.432397356868));
#35068=CARTESIAN_POINT('Ctrl Pts',(-57.8237513008106,-74.5067034561762,
175.148939465042));
#35069=CARTESIAN_POINT('Ctrl Pts',(-57.9048085027795,-74.4652282828169,
175.540226350866));
#35070=CARTESIAN_POINT('Ctrl Pts',(-57.9108912239646,-74.4023961896717,
176.322079499261));
#35071=CARTESIAN_POINT('Ctrl Pts',(-57.8402282212688,-74.381365088574,176.70498371168));
#35072=CARTESIAN_POINT('Ctrl Pts',(-57.5539522654626,-74.3484013270949,
177.434334602834));
#35073=CARTESIAN_POINT('Ctrl Pts',(-57.3372981970406,-74.3386738447082,
177.772220279817));
#35074=CARTESIAN_POINT('Ctrl Pts',(-56.7934819174716,-74.3343764047435,
178.337326110435));
#35075=CARTESIAN_POINT('Ctrl Pts',(-56.474676243902,-74.339838461472,178.561989840184));
#35076=CARTESIAN_POINT('Ctrl Pts',(-55.7595098992864,-74.3526661832745,
178.883184739858));
#35077=CARTESIAN_POINT('Ctrl Pts',(-55.368510085521,-74.3615362269356,178.972859944194));
#35078=CARTESIAN_POINT('Ctrl Pts',(-54.5849379680645,-74.3827096517394,
178.995331361022));
#35079=CARTESIAN_POINT('Ctrl Pts',(-54.2001311788535,-74.3952408085493,
178.931996815635));
#35080=CARTESIAN_POINT('Ctrl Pts',(-53.4650579362335,-74.4102619637419,
178.659863551114));
#35081=CARTESIAN_POINT('Ctrl Pts',(-53.123406503473,-74.4138837139738,178.449958816363));
#35082=CARTESIAN_POINT('Ctrl Pts',(-52.5482581730315,-74.4127488661628,
177.917040578791));
#35083=CARTESIAN_POINT('Ctrl Pts',(-52.3177323071135,-74.4088585779677,
177.602070757164));
#35084=CARTESIAN_POINT('Ctrl Pts',(-51.9829683279186,-74.3812775381616,
176.89381178252));
#35085=CARTESIAN_POINT('Ctrl Pts',(-51.8855522842931,-74.3588762395479,
176.505737024407));
#35086=CARTESIAN_POINT('Ctrl Pts',(-51.8465724378342,-74.3004934140384,
175.724870075675));
#35087=CARTESIAN_POINT('Ctrl Pts',(-51.9017164538028,-74.2661673311796,
175.339801118751));
#35088=CARTESIAN_POINT('Ctrl Pts',(-52.1563832812566,-74.1758245781323,
174.604064259488));
#35089=CARTESIAN_POINT('Ctrl Pts',(-52.3570212774142,-74.1216643244169,
174.261723152778));
#35090=CARTESIAN_POINT('Ctrl Pts',(-52.7320292384492,-74.0361458916242,
173.840973054109));
#35091=CARTESIAN_POINT('Ctrl Pts',(-52.8567013290755,-74.0093235894973,
173.723525706652));
#35092=CARTESIAN_POINT('Ctrl Pts',(-52.9904383367094,-73.9820036993662,
173.617797875548));
#35093=CARTESIAN_POINT('Origin',(-54.1598171290174,-67.5719248685924,175.985485069079));
#35094=CARTESIAN_POINT('',(-52.7784263278132,-71.9932727200521,173.617797875548));
#35095=CARTESIAN_POINT('',(-52.8314293300373,-72.4904554648806,173.617797875548));
#35096=CARTESIAN_POINT('',(-52.327900808713,-67.7672193871761,173.617797875548));
#35097=CARTESIAN_POINT('Ctrl Pts',(-52.7784263278132,-71.9932727200521,
173.617797875548));
#35098=CARTESIAN_POINT('Ctrl Pts',(-52.4874355225081,-72.0527165267496,
173.847845094791));
#35099=CARTESIAN_POINT('Ctrl Pts',(-52.2419020096117,-72.1092868075074,
174.131385486844));
#35100=CARTESIAN_POINT('Ctrl Pts',(-51.854415347595,-72.2143553338943,174.799098541648));
#35101=CARTESIAN_POINT('Ctrl Pts',(-51.7249842477566,-72.2609156045222,
175.182018902505));
#35102=CARTESIAN_POINT('Ctrl Pts',(-51.6254178270345,-72.3315839743407,
175.962627033479));
#35103=CARTESIAN_POINT('Ctrl Pts',(-51.6507227993994,-72.3599316272761,
176.351968123227));
#35104=CARTESIAN_POINT('Ctrl Pts',(-51.8510838928015,-72.4032709574674,
177.115525816536));
#35105=CARTESIAN_POINT('Ctrl Pts',(-52.0298106290951,-72.4169795654191,
177.480788499263));
#35106=CARTESIAN_POINT('Ctrl Pts',(-52.5101183213077,-72.4258296351316,
178.108069805027));
#35107=CARTESIAN_POINT('Ctrl Pts',(-52.8027222218384,-72.4256811742122,
178.367710151333));
#35108=CARTESIAN_POINT('Ctrl Pts',(-53.4832670754377,-72.4178296438271,
178.770002635437));
#35109=CARTESIAN_POINT('Ctrl Pts',(-53.8674803868508,-72.4096320330776,
178.903646333472));
#35110=CARTESIAN_POINT('Ctrl Pts',(-54.6500173974771,-72.386262604351,179.010156251863));
#35111=CARTESIAN_POINT('Ctrl Pts',(-55.0404369208613,-72.3756860624331,
178.988005692624));
#35112=CARTESIAN_POINT('Ctrl Pts',(-55.8065143189993,-72.3587161228737,
178.793381641246));
#35113=CARTESIAN_POINT('Ctrl Pts',(-56.1731748362746,-72.352389782025,178.617122071665));
#35114=CARTESIAN_POINT('Ctrl Pts',(-56.8032596922529,-72.3452729501008,
178.140471210068));
#35115=CARTESIAN_POINT('Ctrl Pts',(-57.0647144411369,-72.3484446113575,
177.849505592283));
#35116=CARTESIAN_POINT('Ctrl Pts',(-57.4715721561285,-72.369769816264,177.17197188452));
#35117=CARTESIAN_POINT('Ctrl Pts',(-57.6079233964997,-72.3879960096499,
176.789057794065));
#35118=CARTESIAN_POINT('Ctrl Pts',(-57.7201786848776,-72.4360834612763,
176.00845620547));
#35119=CARTESIAN_POINT('Ctrl Pts',(-57.701433091218,-72.4691260247665,175.61911557349));
#35120=CARTESIAN_POINT('Ctrl Pts',(-57.5147414361687,-72.5537274787296,
174.855553244988));
#35121=CARTESIAN_POINT('Ctrl Pts',(-57.3429363973152,-72.6048052188926,
174.490285144426));
#35122=CARTESIAN_POINT('Ctrl Pts',(-56.8753157606339,-72.7147115247956,
173.862987108372));
#35123=CARTESIAN_POINT('Ctrl Pts',(-56.5892680221202,-72.7762499318678,
173.603335939967));
#35124=CARTESIAN_POINT('Ctrl Pts',(-55.9223819587286,-72.9120432326736,
173.201017172362));
#35125=CARTESIAN_POINT('Ctrl Pts',(-55.5450826918185,-72.9850280612433,
173.06735798104));
#35126=CARTESIAN_POINT('Ctrl Pts',(-54.7752137718068,-73.127156275602,172.960815048826));
#35127=CARTESIAN_POINT('Ctrl Pts',(-54.39133941398,-73.1991232765269,172.982948618528));
#35128=CARTESIAN_POINT('Ctrl Pts',(-53.6388963329757,-73.3440374353567,
173.177538054862));
#35129=CARTESIAN_POINT('Ctrl Pts',(-53.2791364230434,-73.4151524844253,
173.353780326124));
#35130=CARTESIAN_POINT('Ctrl Pts',(-52.9553536206288,-73.4811624409117,
173.603716331819));
#35131=CARTESIAN_POINT('Ctrl Pts',(-52.9463733724799,-73.4829950858397,
173.610731773291));
#35132=CARTESIAN_POINT('Ctrl Pts',(-52.9374353344854,-73.4848209545377,
173.617797875548));
#35133=CARTESIAN_POINT('Ctrl Pts',(-52.9904383367094,-73.9820036993662,
173.617797875548));
#35134=CARTESIAN_POINT('Ctrl Pts',(-53.1553110450625,-73.9483233863585,
173.487455241368));
#35135=CARTESIAN_POINT('Ctrl Pts',(-53.3337275237714,-73.9125044170173,
173.374987996813));
#35136=CARTESIAN_POINT('Ctrl Pts',(-53.8734962529804,-73.805818482098,173.111112646691));
#35137=CARTESIAN_POINT('Ctrl Pts',(-54.2541774238143,-73.7324815471996,
173.01171038204));
#35138=CARTESIAN_POINT('Ctrl Pts',(-55.0234181079905,-73.5877606109365,
172.96879303946));
#35139=CARTESIAN_POINT('Ctrl Pts',(-55.4044453970555,-73.5187067413993,
173.02228372683));
#35140=CARTESIAN_POINT('Ctrl Pts',(-56.132592882784,-73.3780446152237,173.275564729262));
#35141=CARTESIAN_POINT('Ctrl Pts',(-56.4717530818814,-73.3091527358298,
173.476042168944));
#35142=CARTESIAN_POINT('Ctrl Pts',(-57.0473596050972,-73.1849874493357,
173.993471152876));
#35143=CARTESIAN_POINT('Ctrl Pts',(-57.2804732945259,-73.1316967319038,
174.303002885404));
#35144=CARTESIAN_POINT('Ctrl Pts',(-57.6198344451369,-73.0325627744389,
175.002350201893));
#35145=CARTESIAN_POINT('Ctrl Pts',(-57.7201522302408,-72.9891532290938,
175.386808070376));
#35146=CARTESIAN_POINT('Ctrl Pts',(-57.7666314066635,-72.9213105141303,
176.166353229708));
#35147=CARTESIAN_POINT('Ctrl Pts',(-57.7154678118553,-72.8983119303155,
176.553704035339));
#35148=CARTESIAN_POINT('Ctrl Pts',(-57.4665697516579,-72.8619727200906,
177.295849974148));
#35149=CARTESIAN_POINT('Ctrl Pts',(-57.2685877852196,-72.850385520672,177.642568170487));
#35150=CARTESIAN_POINT('Ctrl Pts',(-56.7553577051062,-72.8421268131452,
178.235012179866));
#35151=CARTESIAN_POINT('Ctrl Pts',(-56.4473243401806,-72.846490506357,178.476861972734));
#35152=CARTESIAN_POINT('Ctrl Pts',(-55.7498624927776,-72.8580546688818,
178.833885088967));
#35153=CARTESIAN_POINT('Ctrl Pts',(-55.3660396770667,-72.8663023543203,
178.943181382324));
#35154=CARTESIAN_POINT('Ctrl Pts',(-54.5850133533515,-72.8865093358843,
179.007121977488));
#35155=CARTESIAN_POINT('Ctrl Pts',(-54.1956965410825,-72.8995083972586,
178.963761237945));
#35156=CARTESIAN_POINT('Ctrl Pts',(-53.4480085814119,-72.9165114886649,
178.729766400635));
#35157=CARTESIAN_POINT('Ctrl Pts',(-53.0977170435069,-72.9212088575917,
178.538985461051));
#35158=CARTESIAN_POINT('Ctrl Pts',(-52.4951376818609,-72.9223107963204,
178.037530682304));
#35159=CARTESIAN_POINT('Ctrl Pts',(-52.2472698728753,-72.920192371099,177.733541985202));
#35160=CARTESIAN_POINT('Ctrl Pts',(-51.8767232141554,-72.897074960845,177.043400876252));
#35161=CARTESIAN_POINT('Ctrl Pts',(-51.7597509275285,-72.876924531648,176.662840230563));
#35162=CARTESIAN_POINT('Ctrl Pts',(-51.6791019803236,-72.822305760216,175.884920756758));
#35163=CARTESIAN_POINT('Ctrl Pts',(-51.7141846959403,-72.7899769925759,
175.495274507088));
#35164=CARTESIAN_POINT('Ctrl Pts',(-51.9307601176331,-72.7043542823012,
174.746958074078));
#35165=CARTESIAN_POINT('Ctrl Pts',(-52.1122334186126,-72.6524143093864,
174.396133406655));
#35166=CARTESIAN_POINT('Ctrl Pts',(-52.496335077636,-72.5612400686153,173.915224673226));
#35167=CARTESIAN_POINT('Ctrl Pts',(-52.6559452899231,-72.5263034682156,
173.756529459893));
#35168=CARTESIAN_POINT('Ctrl Pts',(-52.8314293300374,-72.4904554648806,
173.617797875548));
#35169=CARTESIAN_POINT('Origin',(-54.1598171290174,-67.5719248685924,175.985485069079));
#35170=CARTESIAN_POINT('',(-52.6194173211409,-70.5017244855665,173.617797875548));
#35171=CARTESIAN_POINT('',(-52.6724203233655,-70.9989072303948,173.617797875547));
#35172=CARTESIAN_POINT('',(-52.327900808713,-67.7672193871761,173.617797875548));
#35173=CARTESIAN_POINT('Ctrl Pts',(-52.6194173211409,-70.5017244855665,
173.617797875548));
#35174=CARTESIAN_POINT('Ctrl Pts',(-52.3283899981591,-70.5611757521207,
173.847873964397));
#35175=CARTESIAN_POINT('Ctrl Pts',(-52.0828318333189,-70.6177526805768,
174.131456323592));
#35176=CARTESIAN_POINT('Ctrl Pts',(-51.6953518096301,-70.7228245394826,
174.799229518335));
#35177=CARTESIAN_POINT('Ctrl Pts',(-51.5659380917167,-70.7693828317876,
175.182158067545));
#35178=CARTESIAN_POINT('Ctrl Pts',(-51.4664086415161,-70.8400463575936,
175.962774742001));
#35179=CARTESIAN_POINT('Ctrl Pts',(-51.4917328503677,-70.8683934935249,
176.352116429609));
#35180=CARTESIAN_POINT('Ctrl Pts',(-51.6921328469686,-70.9117290486146,
177.115668068469));
#35181=CARTESIAN_POINT('Ctrl Pts',(-51.8708789903038,-70.9254354529018,
177.480923674582));
#35182=CARTESIAN_POINT('Ctrl Pts',(-52.3512212294813,-70.9342808688144,
178.108183129553));
#35183=CARTESIAN_POINT('Ctrl Pts',(-52.643840262403,-70.9341324441656,178.36780934192));
#35184=CARTESIAN_POINT('Ctrl Pts',(-53.3244101358798,-70.9262786468521,
178.77006749819));
#35185=CARTESIAN_POINT('Ctrl Pts',(-53.7086328505657,-70.9180798887446,
178.903690960978));
#35186=CARTESIAN_POINT('Ctrl Pts',(-54.4911795781716,-70.8947083799637,
179.010157761786));
#35187=CARTESIAN_POINT('Ctrl Pts',(-54.8815999762017,-70.8841335187636,
178.987985013315));
#35188=CARTESIAN_POINT('Ctrl Pts',(-55.6476704562077,-70.8671647473231,
178.793315752586));
#35189=CARTESIAN_POINT('Ctrl Pts',(-56.0143228178515,-70.8608391200856,
178.617033590719));
#35190=CARTESIAN_POINT('Ctrl Pts',(-56.6443824229989,-70.8537238570835,
178.140342422428));
#35191=CARTESIAN_POINT('Ctrl Pts',(-56.9058211161949,-70.8568991378029,
177.849359403895));
#35192=CARTESIAN_POINT('Ctrl Pts',(-57.3126393966221,-70.8782290098234,
177.17179664023));
#35193=CARTESIAN_POINT('Ctrl Pts',(-57.448967345067,-70.896457518701,176.788871593169));
#35194=CARTESIAN_POINT('Ctrl Pts',(-57.5611729127472,-70.9445490631288,
176.008258572745));
#35195=CARTESIAN_POINT('Ctrl Pts',(-57.5424020135795,-70.9775963761197,
175.61891714085));
#35196=CARTESIAN_POINT('Ctrl Pts',(-57.355658411896,-71.0622038660495,174.855362912306));
#35197=CARTESIAN_POINT('Ctrl Pts',(-57.1838273685927,-71.1132841982438,
174.490104279311));
#35198=CARTESIAN_POINT('Ctrl Pts',(-56.7161602346341,-71.2231941621447,
173.862835478345));
#35199=CARTESIAN_POINT('Ctrl Pts',(-56.4300927147269,-71.2847368846005,
173.603203220681));
#35200=CARTESIAN_POINT('Ctrl Pts',(-55.7631732880258,-71.420534277891,173.200930381758));
#35201=CARTESIAN_POINT('Ctrl Pts',(-55.385861398193,-71.4935202583481,173.067298263967));
#35202=CARTESIAN_POINT('Ctrl Pts',(-54.6159791817969,-71.6356484932274,
172.960813021029));
#35203=CARTESIAN_POINT('Ctrl Pts',(-54.2321041540749,-71.7076179385728,
172.98297627877));
#35204=CARTESIAN_POINT('Ctrl Pts',(-53.4796704495815,-71.8525316740027,
173.177626202615));
#35205=CARTESIAN_POINT('Ctrl Pts',(-53.1199214064205,-71.9236453561953,
173.353898701391));
#35206=CARTESIAN_POINT('Ctrl Pts',(-52.7962190670824,-71.989639827505,173.603814414118));
#35207=CARTESIAN_POINT('Ctrl Pts',(-52.7873018860386,-71.9914596147653,
173.610781167625));
#35208=CARTESIAN_POINT('Ctrl Pts',(-52.7784263278132,-71.9932727200521,
173.617797875548));
#35209=CARTESIAN_POINT('Ctrl Pts',(-52.8314293300374,-72.4904554648806,
173.617797875548));
#35210=CARTESIAN_POINT('Ctrl Pts',(-52.9562042748654,-72.4649663512528,
173.519155139882));
#35211=CARTESIAN_POINT('Ctrl Pts',(-53.0888728652022,-72.4382244869968,
173.430644439586));
#35212=CARTESIAN_POINT('Ctrl Pts',(-53.5678939714476,-72.3428470269725,
173.164685182053));
#35213=CARTESIAN_POINT('Ctrl Pts',(-53.9408870073599,-72.2705175725099,
173.045737100393));
#35214=CARTESIAN_POINT('Ctrl Pts',(-54.7068403761519,-72.1254929997893,
172.961040170675));
#35215=CARTESIAN_POINT('Ctrl Pts',(-55.0923870636032,-72.0556883697972,
172.994380514604));
#35216=CARTESIAN_POINT('Ctrl Pts',(-55.8328164429564,-71.914391705921,173.209428337053));
#35217=CARTESIAN_POINT('Ctrl Pts',(-56.1801273911734,-71.8448288729157,
173.390642971781));
#35218=CARTESIAN_POINT('Ctrl Pts',(-56.7825455499323,-71.7171656222667,
173.876277011709));
#35219=CARTESIAN_POINT('Ctrl Pts',(-57.0329394139578,-71.6617018875866,
174.174835645679));
#35220=CARTESIAN_POINT('Ctrl Pts',(-57.4076029540624,-71.5594843653007,
174.855845912787));
#35221=CARTESIAN_POINT('Ctrl Pts',(-57.5270451576265,-71.5142434180066,
175.232397895274));
#35222=CARTESIAN_POINT('Ctrl Pts',(-57.6145373411043,-71.4414046018991,
176.008453264421));
#35223=CARTESIAN_POINT('Ctrl Pts',(-57.5831660846008,-71.4159054217256,
176.400326411267));
#35224=CARTESIAN_POINT('Ctrl Pts',(-57.3718410495929,-71.3762438522241,
177.154339528067));
#35225=CARTESIAN_POINT('Ctrl Pts',(-57.1928125044782,-71.3628521244282,
177.508852862468));
#35226=CARTESIAN_POINT('Ctrl Pts',(-56.7108278926429,-71.3506558158484,
178.127690347984));
#35227=CARTESIAN_POINT('Ctrl Pts',(-56.4134978759637,-71.3534304841221,
178.386691236702));
#35228=CARTESIAN_POINT('Ctrl Pts',(-55.7341769742953,-71.3637454216852,
178.778320887476));
#35229=CARTESIAN_POINT('Ctrl Pts',(-55.3583039876754,-71.3713694275508,
178.906310809509));
#35230=CARTESIAN_POINT('Ctrl Pts',(-54.5856989608393,-71.3904835507265,
179.010054932807));
#35231=CARTESIAN_POINT('Ctrl Pts',(-54.1968324650935,-71.4032549324752,
178.98747721674));
#35232=CARTESIAN_POINT('Ctrl Pts',(-53.4366145322674,-71.422326711838,178.793849110096));
#35233=CARTESIAN_POINT('Ctrl Pts',(-53.0737837008178,-71.4281550162257,
178.6201435409));
#35234=CARTESIAN_POINT('Ctrl Pts',(-52.4459767551618,-71.4313829597214,
178.14933536471));
#35235=CARTESIAN_POINT('Ctrl Pts',(-52.1844055279917,-71.4305258825894,
177.860501800465));
#35236=CARTESIAN_POINT('Ctrl Pts',(-51.7772182332885,-71.4120470745932,
177.189773111793));
#35237=CARTESIAN_POINT('Ctrl Pts',(-51.6396120902311,-71.3938596575389,
176.811926665257));
#35238=CARTESIAN_POINT('Ctrl Pts',(-51.5205195801389,-71.3427973554989,
176.037787112913));
#35239=CARTESIAN_POINT('Ctrl Pts',(-51.5356336824963,-71.3123817412031,
175.649640414745));
#35240=CARTESIAN_POINT('Ctrl Pts',(-51.7132874414347,-71.2316383216106,
174.889256332101));
#35241=CARTESIAN_POINT('Ctrl Pts',(-51.8787843813605,-71.1811339473371,
174.525567559822));
#35242=CARTESIAN_POINT('Ctrl Pts',(-52.2699480870556,-71.0845630084185,
173.983931897263));
#35243=CARTESIAN_POINT('Ctrl Pts',(-52.459297511381,-71.0424441085624,173.78628536505));
#35244=CARTESIAN_POINT('Ctrl Pts',(-52.672420323366,-70.9989072303947,173.617797875547));
#35245=CARTESIAN_POINT('Origin',(-54.1598171290174,-67.5719248685924,175.985485069079));
#35246=CARTESIAN_POINT('',(-52.4604083144687,-69.0101762510808,173.617797875548));
#35247=CARTESIAN_POINT('',(-52.5134113166933,-69.5073589959092,173.617797875547));
#35248=CARTESIAN_POINT('',(-52.327900808713,-67.7672193871761,173.617797875548));
#35249=CARTESIAN_POINT('Ctrl Pts',(-52.4604083144687,-69.0101762510809,
173.617797875548));
#35250=CARTESIAN_POINT('Ctrl Pts',(-52.1693605954265,-69.0696316841567,
173.847890088814));
#35251=CARTESIAN_POINT('Ctrl Pts',(-51.9237886625342,-69.1262123254704,
174.131495888427));
#35252=CARTESIAN_POINT('Ctrl Pts',(-51.5363123485411,-69.2312860454002,
174.799302673213));
#35253=CARTESIAN_POINT('Ctrl Pts',(-51.4069083390629,-69.2778432327096,
175.182235795486));
#35254=CARTESIAN_POINT('Ctrl Pts',(-51.3073995380121,-69.3485040529588,
175.962857241318));
#35255=CARTESIAN_POINT('Ctrl Pts',(-51.3327344910843,-69.3768509003128,
176.352199262857));
#35256=CARTESIAN_POINT('Ctrl Pts',(-51.5331562164762,-69.4201843468438,
177.11574751968));
#35257=CARTESIAN_POINT('Ctrl Pts',(-51.7119131991822,-69.4338895202854,
177.480999172827));
#35258=CARTESIAN_POINT('Ctrl Pts',(-52.192274733854,-69.44273233687,178.108246422932));
#35259=CARTESIAN_POINT('Ctrl Pts',(-52.4849022188737,-69.4425839326948,
178.367864740911));
#35260=CARTESIAN_POINT('Ctrl Pts',(-53.1654860667179,-69.4347288691997,
178.770103723224));
#35261=CARTESIAN_POINT('Ctrl Pts',(-53.5497140330834,-69.4265294702486,
178.903715883489));
#35262=CARTESIAN_POINT('Ctrl Pts',(-54.3322661875416,-69.4031567996751,
179.010158601014));
#35263=CARTESIAN_POINT('Ctrl Pts',(-54.722687074142,-69.3925828774908,178.987973458713));
#35264=CARTESIAN_POINT('Ctrl Pts',(-55.4887536894349,-69.3756147585238,
178.793278946101));
#35265=CARTESIAN_POINT('Ctrl Pts',(-55.8554014951372,-69.369289529889,178.616984165394));
#35266=CARTESIAN_POINT('Ctrl Pts',(-56.4854469957362,-69.3621751432259,
178.140270483872));
#35267=CARTESIAN_POINT('Ctrl Pts',(-56.7468767208699,-69.3653524459278,
177.849277745933));
#35268=CARTESIAN_POINT('Ctrl Pts',(-57.1536729740576,-69.3866849248342,
177.171698753104));
#35269=CARTESIAN_POINT('Ctrl Pts',(-57.2899879121142,-69.4049147270426,
176.788767586683));
#35270=CARTESIAN_POINT('Ctrl Pts',(-57.4021657072611,-69.4530085575371,
176.008148181518));
#35271=CARTESIAN_POINT('Ctrl Pts',(-57.383380673139,-69.4860585238073,175.618806302801));
#35272=CARTESIAN_POINT('Ctrl Pts',(-57.1966080552522,-69.5706693852312,
174.855256599452));
#35273=CARTESIAN_POINT('Ctrl Pts',(-57.0247624866957,-69.6217511651833,
174.490003255593));
#35274=CARTESIAN_POINT('Ctrl Pts',(-56.5570693807535,-69.7316631722538,
173.862750785456));
#35275=CARTESIAN_POINT('Ctrl Pts',(-56.2709908112683,-69.7932083056091,
173.603129091057));
#35276=CARTESIAN_POINT('Ctrl Pts',(-55.6040527487679,-69.9290079847868,
173.200881908029));
#35277=CARTESIAN_POINT('Ctrl Pts',(-55.2267338087179,-70.0019946085126,
173.067264913663));
#35278=CARTESIAN_POINT('Ctrl Pts',(-54.4568441659993,-70.1441228546788,
172.960811895719));
#35279=CARTESIAN_POINT('Ctrl Pts',(-54.0729687641061,-70.2160936659234,
172.982991737176));
#35280=CARTESIAN_POINT('Ctrl Pts',(-53.320540298346,-70.3610071646567,173.177675449537));
#35281=CARTESIAN_POINT('Ctrl Pts',(-52.9607973264131,-70.4321200831111,
173.353964833173));
#35282=CARTESIAN_POINT('Ctrl Pts',(-52.6371399314,-70.4981059047316,173.603869205298));
#35283=CARTESIAN_POINT('Ctrl Pts',(-52.6282579780116,-70.4999185099531,
173.610808759424));
#35284=CARTESIAN_POINT('Ctrl Pts',(-52.6194173211409,-70.5017244855665,
173.617797875548));
#35285=CARTESIAN_POINT('Ctrl Pts',(-52.672420323366,-70.9989072303948,173.617797875547));
#35286=CARTESIAN_POINT('Ctrl Pts',(-52.7572963079739,-70.9815687044678,
173.550697871411));
#35287=CARTESIAN_POINT('Ctrl Pts',(-52.8458825851797,-70.9636387281008,
173.488241353861));
#35288=CARTESIAN_POINT('Ctrl Pts',(-53.2713381202172,-70.8782721564819,
173.222237068703));
#35289=CARTESIAN_POINT('Ctrl Pts',(-53.6425444100623,-70.8058346859752,
173.083175461064));
#35290=CARTESIAN_POINT('Ctrl Pts',(-54.4047250023173,-70.660714632616,172.962042479254));
#35291=CARTESIAN_POINT('Ctrl Pts',(-54.7877460202482,-70.5909436825598,
172.976234072482));
#35292=CARTESIAN_POINT('Ctrl Pts',(-55.5395694398728,-70.4491514401287,
173.153536028243));
#35293=CARTESIAN_POINT('Ctrl Pts',(-55.8998399007808,-70.3778776500482,
173.31987650022));
#35294=CARTESIAN_POINT('Ctrl Pts',(-56.5243924397598,-70.2473793664142,
173.777972980736));
#35295=CARTESIAN_POINT('Ctrl Pts',(-56.7857429943176,-70.1905084931426,
174.061223877771));
#35296=CARTESIAN_POINT('Ctrl Pts',(-57.1941771340838,-70.0854016611449,
174.723930962653));
#35297=CARTESIAN_POINT('Ctrl Pts',(-57.3328464299732,-70.0377507510437,
175.099700802466));
#35298=CARTESIAN_POINT('Ctrl Pts',(-57.4540999137606,-69.9608596798413,
175.872121592076));
#35299=CARTESIAN_POINT('Ctrl Pts',(-57.440685526587,-69.9332079842681,176.260487022286));
#35300=CARTESIAN_POINT('Ctrl Pts',(-57.265232808692,-69.8904230715712,177.025146062232));
#35301=CARTESIAN_POINT('Ctrl Pts',(-57.0996962488948,-69.8752020352117,
177.392871258399));
#35302=CARTESIAN_POINT('Ctrl Pts',(-56.643161561418,-69.8598616367307,178.032318363389));
#35303=CARTESIAN_POINT('Ctrl Pts',(-56.3609216026066,-69.8607946766598,
178.300873260204));
#35304=CARTESIAN_POINT('Ctrl Pts',(-55.699097194158,-69.8699336606263,178.724542927165));
#35305=CARTESIAN_POINT('Ctrl Pts',(-55.3229577642767,-69.8771644924136,
178.871069286089));
#35306=CARTESIAN_POINT('Ctrl Pts',(-54.5489509145704,-69.8956257066586,
179.006822433305));
#35307=CARTESIAN_POINT('Ctrl Pts',(-54.1595932969062,-69.9079035694343,
178.999913816536));
#35308=CARTESIAN_POINT('Ctrl Pts',(-53.390934444243,-69.9285028947367,178.836805075672));
#35309=CARTESIAN_POINT('Ctrl Pts',(-53.0200722271393,-69.9351719522811,
178.676926097263));
#35310=CARTESIAN_POINT('Ctrl Pts',(-52.3732877871734,-69.9400296677875,
178.229928690249));
#35311=CARTESIAN_POINT('Ctrl Pts',(-52.1007298406361,-69.9397809636524,
177.951484677003));
#35312=CARTESIAN_POINT('Ctrl Pts',(-51.6671509552613,-69.9247271768927,
177.295800718053));
#35313=CARTESIAN_POINT('Ctrl Pts',(-51.5147101621089,-69.9081124020225,
176.921947998387));
#35314=CARTESIAN_POINT('Ctrl Pts',(-51.3665292113395,-69.8597771442516,
176.151124637624));
#35315=CARTESIAN_POINT('Ctrl Pts',(-51.3671074059843,-69.8303354798373,
175.762566408402));
#35316=CARTESIAN_POINT('Ctrl Pts',(-51.5166173378049,-69.7531866990917,
174.994383443823));
#35317=CARTESIAN_POINT('Ctrl Pts',(-51.6692798777348,-69.7040476858894,
174.623318326548));
#35318=CARTESIAN_POINT('Ctrl Pts',(-52.0615192928287,-69.60408144752,174.036545486382));
#35319=CARTESIAN_POINT('Ctrl Pts',(-52.2720672179397,-69.5566609384186,
173.808596133728));
#35320=CARTESIAN_POINT('Ctrl Pts',(-52.5134113166937,-69.5073589959092,
173.617797875547));
#35321=CARTESIAN_POINT('Origin',(-54.1598171290174,-67.5719248685924,175.985485069079));
#35322=CARTESIAN_POINT('',(-52.327900808713,-67.7672193871761,173.617797875548));
#35323=CARTESIAN_POINT('',(-52.3544023100207,-68.0158107614237,173.617797875548));
#35324=CARTESIAN_POINT('',(-52.327900808713,-67.7672193871761,173.617797875548));
#35325=CARTESIAN_POINT('',(-51.2061722201484,-67.8868031488672,176.406000729814));
#35326=CARTESIAN_POINT('Origin',(-54.1598171290174,-67.5719248685924,175.985485069079));
#35327=CARTESIAN_POINT('Ctrl Pts',(-51.2061722201484,-67.8868031488672,
176.406000729814));
#35328=CARTESIAN_POINT('Ctrl Pts',(-51.2442093398032,-67.9036864730888,
176.660526215341));
#35329=CARTESIAN_POINT('Ctrl Pts',(-51.3146528258394,-67.9173738079232,
176.909358579104));
#35330=CARTESIAN_POINT('Ctrl Pts',(-51.5152351703733,-67.9375181701368,
177.37953524706));
#35331=CARTESIAN_POINT('Ctrl Pts',(-51.6435890877445,-67.944011203737,177.599420545134));
#35332=CARTESIAN_POINT('Ctrl Pts',(-52.0333006391845,-67.9511839361311,
178.108281770286));
#35333=CARTESIAN_POINT('Ctrl Pts',(-52.3259328445715,-67.951035543457,178.36789567938));
#35334=CARTESIAN_POINT('Ctrl Pts',(-53.0065244967854,-67.9431797728178,
178.770123953217));
#35335=CARTESIAN_POINT('Ctrl Pts',(-53.3907553959908,-67.9349800159672,
178.903729801116));
#35336=CARTESIAN_POINT('Ctrl Pts',(-54.1733105811054,-67.911606696553,179.010159068422));
#35337=CARTESIAN_POINT('Ctrl Pts',(-54.563731740578,-67.9010332988762,178.987967004301));
#35338=CARTESIAN_POINT('Ctrl Pts',(-55.3297961972899,-67.8840655443144,
178.793258388745));
#35339=CARTESIAN_POINT('Ctrl Pts',(-55.6964414583606,-67.8777405382994,
178.616956560589));
#35340=CARTESIAN_POINT('Ctrl Pts',(-56.3264790815166,-67.8706266410668,
178.140230305713));
#35341=CARTESIAN_POINT('Ctrl Pts',(-56.5879037980432,-67.8738050731258,
177.84923213953));
#35342=CARTESIAN_POINT('Ctrl Pts',(-56.9946877489435,-67.8951390079691,
177.171644082906));
#35343=CARTESIAN_POINT('Ctrl Pts',(-57.130995420637,-67.9133695324918,176.788709499035));
#35344=CARTESIAN_POINT('Ctrl Pts',(-57.2431577048249,-67.9614646397378,
176.008086528225));
#35345=CARTESIAN_POINT('Ctrl Pts',(-57.22436477632,-67.9945160879726,175.618744399953));
#35346=CARTESIAN_POINT('Ctrl Pts',(-57.0375759527826,-68.0791288323693,
174.855197224174));
#35347=CARTESIAN_POINT('Ctrl Pts',(-56.8657222718961,-68.1302114208706,
174.489946834556));
#35348=CARTESIAN_POINT('Ctrl Pts',(-56.3980146606145,-68.2401245690258,
173.862703485486));
#35349=CARTESIAN_POINT('Ctrl Pts',(-56.1119299198568,-68.3016710490094,
173.603087690757));
#35350=CARTESIAN_POINT('Ctrl Pts',(-55.444981449255,-68.4374720048378,173.200854837005));
#35351=CARTESIAN_POINT('Ctrl Pts',(-55.0676585718396,-68.5104589877847,
173.067246289364));
#35352=CARTESIAN_POINT('Ctrl Pts',(-54.2977647817229,-68.6525872401999,
172.960811269529));
#35353=CARTESIAN_POINT('Ctrl Pts',(-53.9138891708593,-68.7245588144605,
172.983000373254));
#35354=CARTESIAN_POINT('Ctrl Pts',(-53.161463631333,-68.8694721809371,173.17770295711));
#35355=CARTESIAN_POINT('Ctrl Pts',(-52.8017240506071,-68.9405846727686,
173.354001771142));
#35356=CARTESIAN_POINT('Ctrl Pts',(-52.4780917569963,-69.0065656635003,
173.603899807813));
#35357=CARTESIAN_POINT('Ctrl Pts',(-52.4692294783172,-69.0083742575158,
173.61082416993));
#35358=CARTESIAN_POINT('Ctrl Pts',(-52.4604083144687,-69.0101762510809,
173.617797875548));
#35359=CARTESIAN_POINT('Ctrl Pts',(-52.5134113166937,-69.5073589959092,
173.617797875547));
#35360=CARTESIAN_POINT('Ctrl Pts',(-52.5703612089117,-69.4957252318083,
173.572775269671));
#35361=CARTESIAN_POINT('Ctrl Pts',(-52.6289988502732,-69.4838216535598,
173.529829711882));
#35362=CARTESIAN_POINT('Ctrl Pts',(-53.0162333713195,-69.4056840337388,
173.267698507262));
#35363=CARTESIAN_POINT('Ctrl Pts',(-53.3836428075408,-69.3336537771499,
173.114872837393));
#35364=CARTESIAN_POINT('Ctrl Pts',(-54.1426249695377,-69.1885382308423,
172.966739412117));
#35365=CARTESIAN_POINT('Ctrl Pts',(-54.5259666435685,-69.1181436387083,
172.967504561822));
#35366=CARTESIAN_POINT('Ctrl Pts',(-55.2848741247798,-68.9761537624689,
173.118636662349));
#35367=CARTESIAN_POINT('Ctrl Pts',(-55.6518019210303,-68.9041773926925,
173.273023636635));
#35368=CARTESIAN_POINT('Ctrl Pts',(-56.292342357894,-68.7716562328909,173.710620541039));
#35369=CARTESIAN_POINT('Ctrl Pts',(-56.5629347183278,-68.7132091635555,
173.985039489163));
#35370=CARTESIAN_POINT('Ctrl Pts',(-56.993771235524,-68.6062523998265,174.63476376294));
#35371=CARTESIAN_POINT('Ctrl Pts',(-57.1449816641965,-68.557275753891,175.006921289638));
#35372=CARTESIAN_POINT('Ctrl Pts',(-57.2908442705036,-68.4774601691156,
175.776324389069));
#35373=CARTESIAN_POINT('Ctrl Pts',(-57.2895986238276,-68.4479219665201,
176.165046908302));
#35374=CARTESIAN_POINT('Ctrl Pts',(-57.1380431293144,-68.403108095657,176.936070273677));
#35375=CARTESIAN_POINT('Ctrl Pts',(-56.983436033436,-68.3867366680171,177.309835220954));
#35376=CARTESIAN_POINT('Ctrl Pts',(-56.5455811494487,-68.3691207015494,
177.963957333703));
#35377=CARTESIAN_POINT('Ctrl Pts',(-56.2712967053373,-68.3686210341301,
178.241059727161));
#35378=CARTESIAN_POINT('Ctrl Pts',(-55.6213846585,-68.3769887926366,178.685182361705));
#35379=CARTESIAN_POINT('Ctrl Pts',(-55.248611689035,-68.3838784978415,178.843189229673));
#35380=CARTESIAN_POINT('Ctrl Pts',(-54.4773946674087,-68.4017743316973,
179.001538701538));
#35381=CARTESIAN_POINT('Ctrl Pts',(-54.0876493921661,-68.4135161851992,
179.005828413077));
#35382=CARTESIAN_POINT('Ctrl Pts',(-53.3133690550624,-68.4351934355329,
178.86454982639));
#35383=CARTESIAN_POINT('Ctrl Pts',(-52.9371189732991,-68.4424571388153,
178.714706823925));
#35384=CARTESIAN_POINT('Ctrl Pts',(-52.2770947901846,-68.4484738928266,
178.284867845583));
#35385=CARTESIAN_POINT('Ctrl Pts',(-51.9967593790322,-68.4484865578345,
178.013740507156));
#35386=CARTESIAN_POINT('Ctrl Pts',(-51.5448249819886,-68.4358481303952,
177.36894097706));
#35387=CARTESIAN_POINT('Ctrl Pts',(-51.3820548446593,-68.4203568417544,
176.998229323375));
#35388=CARTESIAN_POINT('Ctrl Pts',(-51.2134814210369,-68.3739580476686,
176.230043037157));
#35389=CARTESIAN_POINT('Ctrl Pts',(-51.2039210351969,-68.3450410563414,
175.841184499056));
#35390=CARTESIAN_POINT('Ctrl Pts',(-51.3338285231955,-68.2704205523978,
175.067912287805));
#35391=CARTESIAN_POINT('Ctrl Pts',(-51.4774363099468,-68.2222707731338,
174.692005191722));
#35392=CARTESIAN_POINT('Ctrl Pts',(-51.8688199864617,-68.1201595974737,
174.073557295704));
#35393=CARTESIAN_POINT('Ctrl Pts',(-52.0935008498987,-68.0691078954907,
173.824057504042));
#35394=CARTESIAN_POINT('Ctrl Pts',(-52.354402310021,-68.0158107614237,173.617797875547));
#35395=CARTESIAN_POINT('Origin',(-54.1598171290174,-67.5719248685924,175.985485069079));
#35396=CARTESIAN_POINT('',(-55.2910412295901,-67.4513288218828,173.209554841606));
#35397=CARTESIAN_POINT('Origin',(-54.1598171290174,-67.5719248685924,175.985485069079));
#35398=CARTESIAN_POINT('',(-52.706375385453,-66.9726216402874,174.209719673931));
#35399=CARTESIAN_POINT('',(-52.327900808713,-67.7672193871761,173.617797875548));
#35400=CARTESIAN_POINT('Origin',(-54.0803126256813,-66.8261507513496,175.985485069079));
#35401=CARTESIAN_POINT('Origin',(-54.1598171290174,-67.5719248685924,175.985485069079));
#35402=CARTESIAN_POINT('Origin',(-67.1996360619082,-123.504780015625,174.720045501779));
#35403=CARTESIAN_POINT('',(-67.5442983916463,-127.490702460407,175.213634544043));
#35404=CARTESIAN_POINT('',(-67.378281909146,-127.50840092658,174.285183152721));
#35405=CARTESIAN_POINT('Ctrl Pts',(-67.5442983916463,-127.490702460407,
175.213634544043));
#35406=CARTESIAN_POINT('Ctrl Pts',(-67.5304234891054,-127.360552056844,
175.213634544043));
#35407=CARTESIAN_POINT('Ctrl Pts',(-67.4911232584415,-127.242343176682,
175.210516120998));
#35408=CARTESIAN_POINT('Ctrl Pts',(-67.3976318102772,-127.064966904856,
175.187583073578));
#35409=CARTESIAN_POINT('Ctrl Pts',(-67.3485764499634,-126.998815494605,
175.171030834297));
#35410=CARTESIAN_POINT('Ctrl Pts',(-67.2614371723049,-126.906024647463,
175.122511770945));
#35411=CARTESIAN_POINT('Ctrl Pts',(-67.2236083564389,-126.872997757826,
175.095959464675));
#35412=CARTESIAN_POINT('Ctrl Pts',(-67.1587175920526,-126.825313378244,
175.031998610409));
#35413=CARTESIAN_POINT('Ctrl Pts',(-67.1319329002808,-126.808954737066,
174.998533042655));
#35414=CARTESIAN_POINT('Ctrl Pts',(-67.0934708749846,-126.789346268891,
174.932406978357));
#35415=CARTESIAN_POINT('Ctrl Pts',(-67.0799671384498,-126.783835828759,
174.902724578504));
#35416=CARTESIAN_POINT('Ctrl Pts',(-67.0658545717287,-126.779903311541,
174.859846346238));
#35417=CARTESIAN_POINT('Ctrl Pts',(-67.0624952310764,-126.779206031814,
174.848108401062));
#35418=CARTESIAN_POINT('Ctrl Pts',(-67.0577545525741,-126.778661978635,
174.828612174569));
#35419=CARTESIAN_POINT('Ctrl Pts',(-67.0560975302196,-126.778598171298,
174.820956534739));
#35420=CARTESIAN_POINT('Ctrl Pts',(-67.053284270024,-126.778764593349,174.806117475444));
#35421=CARTESIAN_POINT('Ctrl Pts',(-67.0520995699636,-126.778972273436,
174.798946406207));
#35422=CARTESIAN_POINT('Ctrl Pts',(-67.0497682417782,-126.779748480161,
174.782376171418));
#35423=CARTESIAN_POINT('Ctrl Pts',(-67.0487395242194,-126.780404802314,
174.772964425168));
#35424=CARTESIAN_POINT('Ctrl Pts',(-67.0464880300302,-126.783095278756,
174.744041184592));
#35425=CARTESIAN_POINT('Ctrl Pts',(-67.0462281439738,-126.785837729554,
174.724538074904));
#35426=CARTESIAN_POINT('Ctrl Pts',(-67.0493621086417,-126.79773925412,174.662248799475));
#35427=CARTESIAN_POINT('Ctrl Pts',(-67.0575397367902,-126.810420103395,
174.620975896735));
#35428=CARTESIAN_POINT('Ctrl Pts',(-67.0834419506324,-126.845331488276,
174.543860152732));
#35429=CARTESIAN_POINT('Ctrl Pts',(-67.1008154234339,-126.867155779968,
174.50915449495));
#35430=CARTESIAN_POINT('Ctrl Pts',(-67.1455893123903,-126.926226076948,
174.439800207307));
#35431=CARTESIAN_POINT('Ctrl Pts',(-67.1735543698667,-126.965002079791,
174.408765925659));
#35432=CARTESIAN_POINT('Ctrl Pts',(-67.2372224196924,-127.066221558354,
174.350903316986));
#35433=CARTESIAN_POINT('Ctrl Pts',(-67.2736593363266,-127.133754028887,
174.327643511702));
#35434=CARTESIAN_POINT('Ctrl Pts',(-67.3393575884572,-127.299090717255,
174.293845322914));
#35435=CARTESIAN_POINT('Ctrl Pts',(-67.3666704557199,-127.399482298509,
174.285183152721));
#35436=CARTESIAN_POINT('Ctrl Pts',(-67.378281909146,-127.50840092658,174.285183152721));
#35437=CARTESIAN_POINT('',(-67.9083119313868,-132.480228374865,174.285183152721));
#35438=CARTESIAN_POINT('',(-67.4842879135942,-128.502766416237,174.285183152721));
#35439=CARTESIAN_POINT('',(-68.0743284138871,-132.462529908692,175.213634544043));
#35440=CARTESIAN_POINT('Ctrl Pts',(-67.9083119313868,-132.480228374865,
174.285183152721));
#35441=CARTESIAN_POINT('Ctrl Pts',(-67.9221868339278,-132.61037877843,174.285183152721));
#35442=CARTESIAN_POINT('Ctrl Pts',(-67.9114244081542,-132.733924672231,
174.297355020201));
#35443=CARTESIAN_POINT('Ctrl Pts',(-67.8699924093024,-132.925684684914,
174.344687930061));
#35444=CARTESIAN_POINT('Ctrl Pts',(-67.8443212202638,-132.999802444567,
174.374753888159));
#35445=CARTESIAN_POINT('Ctrl Pts',(-67.8002951023317,-133.106576399184,
174.446993199403));
#35446=CARTESIAN_POINT('Ctrl Pts',(-67.7816024584963,-133.145628854038,
174.483766974752));
#35447=CARTESIAN_POINT('Ctrl Pts',(-67.7540846388161,-133.203164606054,
174.564439207132));
#35448=CARTESIAN_POINT('Ctrl Pts',(-67.7444947926817,-133.223401015987,
174.604482828893));
#35449=CARTESIAN_POINT('Ctrl Pts',(-67.7361912381367,-133.247995007409,
174.679066086809));
#35450=CARTESIAN_POINT('Ctrl Pts',(-67.7352352888166,-133.255046946657,
174.711363409076));
#35451=CARTESIAN_POINT('Ctrl Pts',(-67.7379709489151,-133.260192318128,
174.756299066962));
#35452=CARTESIAN_POINT('Ctrl Pts',(-67.7391038286292,-133.261126953466,
174.768439650388));
#35453=CARTESIAN_POINT('Ctrl Pts',(-67.7416282991207,-133.261907269226,
174.78833666097));
#35454=CARTESIAN_POINT('Ctrl Pts',(-67.7427762424715,-133.262025347786,
174.796084363802));
#35455=CARTESIAN_POINT('Ctrl Pts',(-67.7453070065055,-133.261889041713,
174.810974510343));
#35456=CARTESIAN_POINT('Ctrl Pts',(-67.7466640942182,-133.26166298395,174.818114404605));
#35457=CARTESIAN_POINT('Ctrl Pts',(-67.7501112910221,-133.260767818176,
174.834482843182));
#35458=CARTESIAN_POINT('Ctrl Pts',(-67.7522957860694,-133.259988282421,
174.843685576008));
#35459=CARTESIAN_POINT('Ctrl Pts',(-67.7597044638537,-133.256748015752,
174.871676179795));
#35460=CARTESIAN_POINT('Ctrl Pts',(-67.7656627036566,-133.253398082375,
174.890148786256));
#35461=CARTESIAN_POINT('Ctrl Pts',(-67.7876797926514,-133.238815287458,
174.947889688046));
#35462=CARTESIAN_POINT('Ctrl Pts',(-67.8068751667408,-133.223216293268,
174.984212394924));
#35463=CARTESIAN_POINT('Ctrl Pts',(-67.8501756899867,-133.180927434277,
175.048813358858));
#35464=CARTESIAN_POINT('Ctrl Pts',(-67.8736483858866,-133.154748668112,
175.07613230277));
#35465=CARTESIAN_POINT('Ctrl Pts',(-67.9266051867934,-133.085259626664,
175.127812750604));
#35466=CARTESIAN_POINT('Ctrl Pts',(-67.9550417444708,-133.040470834833,
175.148647236133));
#35467=CARTESIAN_POINT('Ctrl Pts',(-68.0127093306509,-132.92631616684,175.184567232953));
#35468=CARTESIAN_POINT('Ctrl Pts',(-68.0403368828129,-132.851953995925,
175.196241474271));
#35469=CARTESIAN_POINT('Ctrl Pts',(-68.0784333077652,-132.675552101541,
175.211269198035));
#35470=CARTESIAN_POINT('Ctrl Pts',(-68.0859398673133,-132.571448536764,
175.213634544043));
#35471=CARTESIAN_POINT('Ctrl Pts',(-68.0743284138871,-132.462529908693,
175.213634544043));
#35472=CARTESIAN_POINT('',(-67.6503043960945,-128.485067950064,175.213634544043));
#35473=CARTESIAN_POINT('Origin',(-67.297435265312,-123.494353967156,176.440911705352));
#35474=CARTESIAN_POINT('',(-67.5269456805235,-127.492552375344,176.901057832219));
#35475=CARTESIAN_POINT('',(-67.5866943482154,-127.486182768194,175.959630076611));
#35476=CARTESIAN_POINT('Ctrl Pts',(-67.5269456805235,-127.492552375344,
176.901057832219));
#35477=CARTESIAN_POINT('Ctrl Pts',(-67.5130707779826,-127.362401971781,
176.901057832219));
#35478=CARTESIAN_POINT('Ctrl Pts',(-67.4752797181248,-127.244032203929,
176.891676686497));
#35479=CARTESIAN_POINT('Ctrl Pts',(-67.3893884463034,-127.065845702528,
176.851661970524));
#35480=CARTESIAN_POINT('Ctrl Pts',(-67.3454787971686,-126.999145725087,
176.825595328984));
#35481=CARTESIAN_POINT('Ctrl Pts',(-67.2721049050013,-126.904887395887,
176.760103849711));
#35482=CARTESIAN_POINT('Ctrl Pts',(-67.2415803914411,-126.871081818825,
176.726158942161));
#35483=CARTESIAN_POINT('Ctrl Pts',(-67.1936285768875,-126.821591634024,
176.649824498254));
#35484=CARTESIAN_POINT('Ctrl Pts',(-67.1755270558813,-126.804307308831,
176.611372500654));
#35485=CARTESIAN_POINT('Ctrl Pts',(-67.1538458843564,-126.782909889533,
176.538512682906));
#35486=CARTESIAN_POINT('Ctrl Pts',(-67.1477766927268,-126.776606877245,
176.506619146556));
#35487=CARTESIAN_POINT('Ctrl Pts',(-67.1442611725493,-126.771544644068,
176.461728312898));
#35488=CARTESIAN_POINT('Ctrl Pts',(-67.1437894619215,-126.770539523688,
176.449549727278));
#35489=CARTESIAN_POINT('Ctrl Pts',(-67.1438227876615,-126.769486529762,
176.429505701555));
#35490=CARTESIAN_POINT('Ctrl Pts',(-67.144034970312,-126.769223452683,176.421679822394));
#35491=CARTESIAN_POINT('Ctrl Pts',(-67.1448342594165,-126.769004752843,
176.406598273492));
#35492=CARTESIAN_POINT('Ctrl Pts',(-67.1453907133999,-126.769026814277,
176.399348394079));
#35493=CARTESIAN_POINT('Ctrl Pts',(-67.1470719186259,-126.769375258133,
176.382685188959));
#35494=CARTESIAN_POINT('Ctrl Pts',(-67.1483144553802,-126.769789449402,
176.373285479704));
#35495=CARTESIAN_POINT('Ctrl Pts',(-67.153018674885,-126.771738400295,176.34459865966));
#35496=CARTESIAN_POINT('Ctrl Pts',(-67.1574157570097,-126.773984387172,
176.325530857575));
#35497=CARTESIAN_POINT('Ctrl Pts',(-67.1753189387193,-126.784311414529,
176.265495447643));
#35498=CARTESIAN_POINT('Ctrl Pts',(-67.1931220500515,-126.79596612299,176.227046168864));
#35499=CARTESIAN_POINT('Ctrl Pts',(-67.2367380042605,-126.828989104805,
176.157449483168));
#35500=CARTESIAN_POINT('Ctrl Pts',(-67.2619379655662,-126.849979040534,
176.127332967841));
#35501=CARTESIAN_POINT('Ctrl Pts',(-67.3221104066357,-126.907407748984,
176.069150160125));
#35502=CARTESIAN_POINT('Ctrl Pts',(-67.3567758945455,-126.945469441177,
176.044688741343));
#35503=CARTESIAN_POINT('Ctrl Pts',(-67.4326940953435,-127.045382971805,
176.0010905983));
#35504=CARTESIAN_POINT('Ctrl Pts',(-67.4738260419191,-127.112414920779,
175.985464248772));
#35505=CARTESIAN_POINT('Ctrl Pts',(-67.5461859605276,-127.277041430993,
175.964087796028));
#35506=CARTESIAN_POINT('Ctrl Pts',(-67.5750828947892,-127.377264140122,
175.959630076611));
#35507=CARTESIAN_POINT('Ctrl Pts',(-67.5866943482154,-127.486182768194,
175.959630076611));
#35508=CARTESIAN_POINT('',(-68.1167243704562,-132.458010216479,175.959630076611));
#35509=CARTESIAN_POINT('',(-67.6927003526636,-128.480548257851,175.959630076611));
#35510=CARTESIAN_POINT('',(-68.0569757027642,-132.46437982363,176.901057832219));
#35511=CARTESIAN_POINT('Ctrl Pts',(-68.1167243704562,-132.458010216479,
175.959630076611));
#35512=CARTESIAN_POINT('Ctrl Pts',(-68.1305992729972,-132.588160620043,
175.959630076611));
#35513=CARTESIAN_POINT('Ctrl Pts',(-68.1176279830643,-132.711941993521,
175.96575292391));
#35514=CARTESIAN_POINT('Ctrl Pts',(-68.0667100701608,-132.904713268018,
175.996986227033));
#35515=CARTESIAN_POINT('Ctrl Pts',(-68.0348487653193,-132.979490935371,
176.01818933525));
#35516=CARTESIAN_POINT('Ctrl Pts',(-67.9752240480408,-133.087927804889,
176.07514399223));
#35517=CARTESIAN_POINT('Ctrl Pts',(-67.9484371380331,-133.127843162595,
176.105410233963));
#35518=CARTESIAN_POINT('Ctrl Pts',(-67.9026888335392,-133.187322406088,
176.175730319761));
#35519=CARTESIAN_POINT('Ctrl Pts',(-67.8839074332612,-133.2085386971,176.211814902049));
#35520=CARTESIAN_POINT('Ctrl Pts',(-67.858169412698,-133.234991319078,176.281631009657));
#35521=CARTESIAN_POINT('Ctrl Pts',(-67.8495768248006,-133.242857375017,
176.312583445894));
#35522=CARTESIAN_POINT('Ctrl Pts',(-67.8415564306939,-133.249149413727,
176.356733820306));
#35523=CARTESIAN_POINT('Ctrl Pts',(-67.8397705625796,-133.250395207083,
176.36876749803));
#35524=CARTESIAN_POINT('Ctrl Pts',(-67.8374900543234,-133.251687765679,
176.388667283164));
#35525=CARTESIAN_POINT('Ctrl Pts',(-67.8367616776014,-133.252005872494,
176.396460029218));
#35526=CARTESIAN_POINT('Ctrl Pts',(-67.8356759440695,-133.252255109224,
176.411523192025));
#35527=CARTESIAN_POINT('Ctrl Pts',(-67.8352942870893,-133.252214413261,
176.418784291187));
#35528=CARTESIAN_POINT('Ctrl Pts',(-67.834744546255,-133.251745347742,176.435520121956));
#35529=CARTESIAN_POINT('Ctrl Pts',(-67.8346739405432,-133.251206220794,
176.444995054306));
#35530=CARTESIAN_POINT('Ctrl Pts',(-67.8351989832514,-133.248699795614,
176.474017526598));
#35531=CARTESIAN_POINT('Ctrl Pts',(-67.8365798970763,-133.245837835766,
176.493456202671));
#35532=CARTESIAN_POINT('Ctrl Pts',(-67.8441792890309,-133.232792063676,
176.555128554074));
#35533=CARTESIAN_POINT('Ctrl Pts',(-67.8541317546755,-133.218178425277,
176.595359388534));
#35534=CARTESIAN_POINT('Ctrl Pts',(-67.8806857394292,-133.177674859172,
176.669460093496));
#35535=CARTESIAN_POINT('Ctrl Pts',(-67.8969028272927,-133.152269589298,
176.702235057584));
#35536=CARTESIAN_POINT('Ctrl Pts',(-67.9358269946965,-133.084276520331,
176.766778609521));
#35537=CARTESIAN_POINT('Ctrl Pts',(-67.9583514108175,-133.040118002288,
176.794910894109));
#35538=CARTESIAN_POINT('Ctrl Pts',(-68.0054646756924,-132.927088495458,
176.846406095349));
#35539=CARTESIAN_POINT('Ctrl Pts',(-68.0292925855365,-132.853131391799,
176.866202042985));
#35540=CARTESIAN_POINT('Ctrl Pts',(-68.0621780150446,-132.677285024345,
176.894333910976));
#35541=CARTESIAN_POINT('Ctrl Pts',(-68.0685871561905,-132.573298451701,
176.901057832219));
#35542=CARTESIAN_POINT('Ctrl Pts',(-68.0569757027643,-132.46437982363,176.901057832219));
#35543=CARTESIAN_POINT('',(-67.6329516849716,-128.486917865001,176.901057832219));
#35544=CARTESIAN_POINT('Origin',(-66.9828828246889,-123.527887358818,178.135310168233));
#35545=CARTESIAN_POINT('',(-67.1085457489275,-127.537156603338,178.535271359373));
#35546=CARTESIAN_POINT('',(-67.390587191423,-127.507089101279,177.635579598685));
#35547=CARTESIAN_POINT('Ctrl Pts',(-67.1085457489275,-127.537156603338,
178.535271359373));
#35548=CARTESIAN_POINT('Ctrl Pts',(-67.0946708463865,-127.407006199774,
178.535271359373));
#35549=CARTESIAN_POINT('Ctrl Pts',(-67.0598354263899,-127.288321340966,
178.520172689065));
#35550=CARTESIAN_POINT('Ctrl Pts',(-66.9853883610814,-127.108914810696,
178.465401814383));
#35551=CARTESIAN_POINT('Ctrl Pts',(-66.9487390141347,-127.041440836536,
178.431335669042));
#35552=CARTESIAN_POINT('Ctrl Pts',(-66.892769389307,-126.945327096161,178.352677900572));
#35553=CARTESIAN_POINT('Ctrl Pts',(-66.8710961252085,-126.910577916772,
178.313313146384));
#35554=CARTESIAN_POINT('Ctrl Pts',(-66.842535554338,-126.859020495843,178.229041393252));
#35555=CARTESIAN_POINT('Ctrl Pts',(-66.8340514938727,-126.840710885103,
178.187837656138));
#35556=CARTESIAN_POINT('Ctrl Pts',(-66.8302659677143,-126.81740567045,178.112478432712));
#35557=CARTESIAN_POINT('Ctrl Pts',(-66.8319414646711,-126.810277022617,
178.080227296269));
#35558=CARTESIAN_POINT('Ctrl Pts',(-66.8391939933177,-126.804066843496,
178.0359327533));
#35559=CARTESIAN_POINT('Ctrl Pts',(-66.8416308614233,-126.802751649191,
178.024021302365));
#35560=CARTESIAN_POINT('Ctrl Pts',(-66.8464298257885,-126.801190606348,
178.00459436333));
#35561=CARTESIAN_POINT('Ctrl Pts',(-66.848497409127,-126.800729731161,177.99705305649));
#35562=CARTESIAN_POINT('Ctrl Pts',(-66.8528619779962,-126.800130948679,
177.982605502784));
#35563=CARTESIAN_POINT('Ctrl Pts',(-66.855127745491,-126.799970785872,177.975698149833));
#35564=CARTESIAN_POINT('Ctrl Pts',(-66.860727011093,-126.799901538316,177.959910379297));
#35565=CARTESIAN_POINT('Ctrl Pts',(-66.8641719392271,-126.80008093995,177.951068983973));
#35566=CARTESIAN_POINT('Ctrl Pts',(-66.8755734916867,-126.801315910406,
177.92428575817));
#35567=CARTESIAN_POINT('Ctrl Pts',(-66.884388630013,-126.803090902975,177.906761415035));
#35568=CARTESIAN_POINT('Ctrl Pts',(-66.9160955160124,-126.811946363234,
177.852468910406));
#35569=CARTESIAN_POINT('Ctrl Pts',(-66.9425724814864,-126.822676380895,
177.819077787913));
#35570=CARTESIAN_POINT('Ctrl Pts',(-67.001598157425,-126.854056583422,177.761044866923));
#35571=CARTESIAN_POINT('Ctrl Pts',(-67.0333051181494,-126.87435282954,177.737267756454));
#35572=CARTESIAN_POINT('Ctrl Pts',(-67.105770211174,-126.930471059166,177.693637801963));
#35573=CARTESIAN_POINT('Ctrl Pts',(-67.1453773011662,-126.968005943563,
177.677170854792));
#35574=CARTESIAN_POINT('Ctrl Pts',(-67.2297952103285,-127.067013348492,
177.650370942981));
#35575=CARTESIAN_POINT('Ctrl Pts',(-67.2736692454281,-127.13375297251,177.643286195844));
#35576=CARTESIAN_POINT('Ctrl Pts',(-67.3495412883826,-127.298005066807,
177.635573800874));
#35577=CARTESIAN_POINT('Ctrl Pts',(-67.3789757379969,-127.398170473209,
177.635579598685));
#35578=CARTESIAN_POINT('Ctrl Pts',(-67.390587191423,-127.507089101279,177.635579598685));
#35579=CARTESIAN_POINT('',(-67.9206172136638,-132.478916549564,177.635579598685));
#35580=CARTESIAN_POINT('',(-67.4965931958712,-128.501454590936,177.635579598685));
#35581=CARTESIAN_POINT('',(-67.6385757711683,-132.508984051623,178.535271359373));
#35582=CARTESIAN_POINT('Ctrl Pts',(-67.9206172136638,-132.478916549564,
177.635579598685));
#35583=CARTESIAN_POINT('Ctrl Pts',(-67.9344921162048,-132.609066953128,
177.635579598685));
#35584=CARTESIAN_POINT('Ctrl Pts',(-67.9208156163139,-132.732923506699,
177.635297588174));
#35585=CARTESIAN_POINT('Ctrl Pts',(-67.8645186117248,-132.926268228307,
177.64861611851));
#35586=CARTESIAN_POINT('Ctrl Pts',(-67.8287561325003,-133.001461786913,
177.659724129265));
#35587=CARTESIAN_POINT('Ctrl Pts',(-67.7576233297767,-133.111125495223,
177.698084134341));
#35588=CARTESIAN_POINT('Ctrl Pts',(-67.7245259380598,-133.151713592439,
177.720083878501));
#35589=CARTESIAN_POINT('Ctrl Pts',(-67.6635403652347,-133.212817230535,
177.775965069934));
#35590=CARTESIAN_POINT('Ctrl Pts',(-67.6367766223592,-133.234884492597,
177.805993507988));
#35591=CARTESIAN_POINT('Ctrl Pts',(-67.5952451752651,-133.263020799357,
177.866985006884));
#35592=CARTESIAN_POINT('Ctrl Pts',(-67.5795578944418,-133.271643196961,
177.894793714006));
#35593=CARTESIAN_POINT('Ctrl Pts',(-67.5612808692556,-133.279028661068,
177.935592945663));
#35594=CARTESIAN_POINT('Ctrl Pts',(-67.5566865068749,-133.280573858676,
177.946820364077));
#35595=CARTESIAN_POINT('Ctrl Pts',(-67.5497399835682,-133.282363845649,
177.965566420584));
#35596=CARTESIAN_POINT('Ctrl Pts',(-67.5471790904136,-133.282877310959,
177.972951323785));
#35597=CARTESIAN_POINT('Ctrl Pts',(-67.5425407759596,-133.283505276549,
177.987312086586));
#35598=CARTESIAN_POINT('Ctrl Pts',(-67.5404420562521,-133.283647630945,
177.994272401957));
#35599=CARTESIAN_POINT('Ctrl Pts',(-67.5359240942179,-133.283601604317,
178.010402999268));
#35600=CARTESIAN_POINT('Ctrl Pts',(-67.5335991423078,-133.283302805735,
178.019599482513));
#35601=CARTESIAN_POINT('Ctrl Pts',(-67.527195024967,-133.281535075309,178.047967142713));
#35602=CARTESIAN_POINT('Ctrl Pts',(-67.5239017286705,-133.279171417488,
178.067242183202));
#35603=CARTESIAN_POINT('Ctrl Pts',(-67.5165668194536,-133.267717741678,
178.129261811322));
#35604=CARTESIAN_POINT('Ctrl Pts',(-67.5166149524489,-133.254159971309,
178.171062703501));
#35605=CARTESIAN_POINT('Ctrl Pts',(-67.524648395552,-133.215630818677,178.250356685862));
#35606=CARTESIAN_POINT('Ctrl Pts',(-67.5325223561117,-133.191114981914,
178.286682908347));
#35607=CARTESIAN_POINT('Ctrl Pts',(-67.5547606554873,-133.124900737955,
178.360338527753));
#35608=CARTESIAN_POINT('Ctrl Pts',(-67.5698080890573,-133.081539316205,
178.394133665277));
#35609=CARTESIAN_POINT('Ctrl Pts',(-67.6029673336494,-132.969997401164,
178.458211357017));
#35610=CARTESIAN_POINT('Ctrl Pts',(-67.6211733118579,-132.896639632977,
178.484978542452));
#35611=CARTESIAN_POINT('Ctrl Pts',(-67.6458808109757,-132.721665087537,
178.524579632757));
#35612=CARTESIAN_POINT('Ctrl Pts',(-67.6501872245945,-132.617902679695,
178.535271359373));
#35613=CARTESIAN_POINT('Ctrl Pts',(-67.6385757711684,-132.508984051624,
178.535271359373));
#35614=CARTESIAN_POINT('',(-67.2145517533757,-128.531522092995,178.535271359373));
#35615=CARTESIAN_POINT('Origin',(-66.2742593845362,-123.603431351777,179.704768610648));
#35616=CARTESIAN_POINT('',(-66.313414480061,-127.621922908787,180.021300575431));
#35617=CARTESIAN_POINT('',(-66.8013574739011,-127.569904925748,179.215631624547));
#35618=CARTESIAN_POINT('Ctrl Pts',(-66.3134144800609,-127.621922908787,
180.021300575431));
#35619=CARTESIAN_POINT('Ctrl Pts',(-66.2995395775199,-127.491772505223,
180.021300575431));
#35620=CARTESIAN_POINT('Ctrl Pts',(-66.2689344953941,-127.372636664135,
180.001361860373));
#35621=CARTESIAN_POINT('Ctrl Pts',(-66.2091105710828,-127.19167120934,179.935017911137));
#35622=CARTESIAN_POINT('Ctrl Pts',(-66.1814141749603,-127.123242790809,
179.894932062535));
#35623=CARTESIAN_POINT('Ctrl Pts',(-66.1454762265654,-127.024993539896,
179.807679308462));
#35624=CARTESIAN_POINT('Ctrl Pts',(-66.133686756639,-126.989190682016,179.765182444064));
#35625=CARTESIAN_POINT('Ctrl Pts',(-66.1258427747035,-126.935424734301,
179.677870949684));
#35626=CARTESIAN_POINT('Ctrl Pts',(-66.1273515327055,-126.916049822352,
179.636310084488));
#35627=CARTESIAN_POINT('Ctrl Pts',(-66.1415364136483,-126.890828842243,
179.562831059531));
#35628=CARTESIAN_POINT('Ctrl Pts',(-66.1508166497229,-126.882889478414,
179.532096641817));
#35629=CARTESIAN_POINT('Ctrl Pts',(-66.1683824296169,-126.875579837807,
179.490972627369));
#35630=CARTESIAN_POINT('Ctrl Pts',(-66.173579789141,-126.873970356674,179.480020561352));
#35631=CARTESIAN_POINT('Ctrl Pts',(-66.1828590649194,-126.871931682703,
179.462339732087));
#35632=CARTESIAN_POINT('Ctrl Pts',(-66.1866604154849,-126.871285976346,
179.455521270909));
#35633=CARTESIAN_POINT('Ctrl Pts',(-66.1943357934833,-126.870334239492,
179.442547351705));
#35634=CARTESIAN_POINT('Ctrl Pts',(-66.1981796948696,-126.870005837069,
179.436383955464));
#35635=CARTESIAN_POINT('Ctrl Pts',(-66.2073748443838,-126.869553244264,
179.422389147348));
#35636=CARTESIAN_POINT('Ctrl Pts',(-66.2128253059833,-126.869518842632,
179.414619895715));
#35637=CARTESIAN_POINT('Ctrl Pts',(-66.2302765860103,-126.870108871711,
179.391296807883));
#35638=CARTESIAN_POINT('Ctrl Pts',(-66.2430141071915,-126.871465712063,
179.376334374823));
#35639=CARTESIAN_POINT('Ctrl Pts',(-66.28675696361,-126.879038057464,179.330940058521));
#35640=CARTESIAN_POINT('Ctrl Pts',(-66.3204520613092,-126.888998574006,
179.304547662982));
#35641=CARTESIAN_POINT('Ctrl Pts',(-66.3916878833257,-126.919077093387,
179.261451169124));
#35642=CARTESIAN_POINT('Ctrl Pts',(-66.4282041912291,-126.938860630965,
179.245395302747));
#35643=CARTESIAN_POINT('Ctrl Pts',(-66.509141631801,-126.994075651739,179.218853815848));
#35644=CARTESIAN_POINT('Ctrl Pts',(-66.5516443075739,-127.031301847347,
179.211338339403));
#35645=CARTESIAN_POINT('Ctrl Pts',(-66.6403175103417,-127.129855609551,
179.202894172283));
#35646=CARTESIAN_POINT('Ctrl Pts',(-66.6848213323291,-127.196528094079,
179.204762767289));
#35647=CARTESIAN_POINT('Ctrl Pts',(-66.7608518455908,-127.360763294379,
179.211162646458));
#35648=CARTESIAN_POINT('Ctrl Pts',(-66.7897460204748,-127.460986297676,
179.215631624547));
#35649=CARTESIAN_POINT('Ctrl Pts',(-66.8013574739011,-127.569904925748,
179.215631624547));
#35650=CARTESIAN_POINT('',(-67.3313874961418,-132.541732374034,179.215631624547));
#35651=CARTESIAN_POINT('',(-66.9073634783493,-128.564270415405,179.215631624547));
#35652=CARTESIAN_POINT('',(-66.8434445023017,-132.593750357073,180.021300575431));
#35653=CARTESIAN_POINT('Ctrl Pts',(-67.3313874961418,-132.541732374034,
179.215631624547));
#35654=CARTESIAN_POINT('Ctrl Pts',(-67.3452623986828,-132.671882777597,
179.215631624547));
#35655=CARTESIAN_POINT('Ctrl Pts',(-67.3324253272744,-132.795649842484,
179.208961145653));
#35656=CARTESIAN_POINT('Ctrl Pts',(-67.2751686666225,-132.989096869839,
179.203590878629));
#35657=CARTESIAN_POINT('Ctrl Pts',(-67.2380206765098,-133.064438133162,
179.203958234714));
#35658=CARTESIAN_POINT('Ctrl Pts',(-67.1601391103383,-133.174821304745,
179.221494243823));
#35659=CARTESIAN_POINT('Ctrl Pts',(-67.1228817636348,-133.215852880954,
179.233948945246));
#35660=CARTESIAN_POINT('Ctrl Pts',(-67.0505376736116,-133.278167412868,
179.272143630587));
#35661=CARTESIAN_POINT('Ctrl Pts',(-67.0174647044214,-133.300907280607,
179.294370780736));
#35662=CARTESIAN_POINT('Ctrl Pts',(-66.9626987268264,-133.330454476737,
179.342993066701));
#35663=CARTESIAN_POINT('Ctrl Pts',(-66.9408710164934,-133.33973148515,179.36604190373));
#35664=CARTESIAN_POINT('Ctrl Pts',(-66.9134328614723,-133.348093586901,
179.401118889585));
#35665=CARTESIAN_POINT('Ctrl Pts',(-66.9063034778645,-133.349909034709,
179.410887551941));
#35666=CARTESIAN_POINT('Ctrl Pts',(-66.8951010750377,-133.352152726872,
179.427390427158));
#35667=CARTESIAN_POINT('Ctrl Pts',(-66.890857968285,-133.35284552739,179.433938303775));
#35668=CARTESIAN_POINT('Ctrl Pts',(-66.8829374526434,-133.353823397555,
179.446762071235));
#35669=CARTESIAN_POINT('Ctrl Pts',(-66.8792431416185,-133.354135852645,
179.453017094585));
#35670=CARTESIAN_POINT('Ctrl Pts',(-66.871016293415,-133.354485218061,179.467605006754));
#35671=CARTESIAN_POINT('Ctrl Pts',(-66.8665687642743,-133.354412700393,
179.475988574717));
#35672=CARTESIAN_POINT('Ctrl Pts',(-66.853592659507,-133.353345587733,179.502052797526));
#35673=CARTESIAN_POINT('Ctrl Pts',(-66.8457999170483,-133.351461600934,
179.520044007139));
#35674=CARTESIAN_POINT('Ctrl Pts',(-66.8238820298286,-133.341562568005,
179.578806556624));
#35675=CARTESIAN_POINT('Ctrl Pts',(-66.8139400097828,-133.329069814694,
179.619748190606));
#35676=CARTESIAN_POINT('Ctrl Pts',(-66.8027552546388,-133.29258945039,179.699627172334));
#35677=CARTESIAN_POINT('Ctrl Pts',(-66.8016834408603,-133.269027292937,
179.737393505205));
#35678=CARTESIAN_POINT('Ctrl Pts',(-66.8055523596816,-133.204771347669,
179.815880595208));
#35679=CARTESIAN_POINT('Ctrl Pts',(-66.8119925047541,-133.162327520377,
179.853374535115));
#35680=CARTESIAN_POINT('Ctrl Pts',(-66.8286089870249,-133.052549174321,
179.926310754825));
#35681=CARTESIAN_POINT('Ctrl Pts',(-66.8396974705112,-132.979950178623,
179.958493566535));
#35682=CARTESIAN_POINT('Ctrl Pts',(-66.8537353758802,-132.806113083157,
180.00726240773));
#35683=CARTESIAN_POINT('Ctrl Pts',(-66.8550559557278,-132.702668985143,
180.021300575431));
#35684=CARTESIAN_POINT('Ctrl Pts',(-66.8434445023018,-132.593750357073,
180.021300575431));
#35685=CARTESIAN_POINT('',(-66.4194204845091,-128.616288398444,180.021300575431));
#35686=CARTESIAN_POINT('Origin',(-65.2127475634542,-123.716595603752,181.058075812673));
#35687=CARTESIAN_POINT('',(-65.1877620130857,-127.741924982132,181.272782863852));
#35688=CARTESIAN_POINT('',(-65.8532490850691,-127.67097961421,180.607959273711));
#35689=CARTESIAN_POINT('Ctrl Pts',(-65.1877620130857,-127.741924982132,
181.272782863852));
#35690=CARTESIAN_POINT('Ctrl Pts',(-65.1738871105448,-127.611774578569,
181.272782863852));
#35691=CARTESIAN_POINT('Ctrl Pts',(-65.1485412124394,-127.492078073329,
181.24916286969));
#35692=CARTESIAN_POINT('Ctrl Pts',(-65.1056695198069,-127.309305397378,
181.175101515076));
#35693=CARTESIAN_POINT('Ctrl Pts',(-65.0880984101856,-127.23979755566,181.131325607029));
#35694=CARTESIAN_POINT('Ctrl Pts',(-65.073655379095,-127.139256802958,181.04054868027));
#35695=CARTESIAN_POINT('Ctrl Pts',(-65.0722078378599,-127.102351426386,
180.997389468952));
#35696=CARTESIAN_POINT('Ctrl Pts',(-65.0852018172639,-127.046364012776,
180.912112460012));
#35697=CARTESIAN_POINT('Ctrl Pts',(-65.096498005373,-127.025945695389,180.872609833152));
#35698=CARTESIAN_POINT('Ctrl Pts',(-65.1276836804105,-126.998912317049,
180.805281340509));
#35699=CARTESIAN_POINT('Ctrl Pts',(-65.143986746339,-126.990224272638,180.777849814166));
#35700=CARTESIAN_POINT('Ctrl Pts',(-65.1708116112281,-126.981927551713,
180.74228630648));
#35701=CARTESIAN_POINT('Ctrl Pts',(-65.1784609451284,-126.98005667373,180.732930119647));
#35702=CARTESIAN_POINT('Ctrl Pts',(-65.1916748256948,-126.977598544601,
180.718022945683));
#35703=CARTESIAN_POINT('Ctrl Pts',(-65.1969875497771,-126.97679171573,180.712323594346));
#35704=CARTESIAN_POINT('Ctrl Pts',(-65.2075268540773,-126.975534665199,
180.70157730667));
#35705=CARTESIAN_POINT('Ctrl Pts',(-65.2127259943301,-126.975061785259,
180.696516061323));
#35706=CARTESIAN_POINT('Ctrl Pts',(-65.2249858715883,-126.974282472001,
180.68512754301));
#35707=CARTESIAN_POINT('Ctrl Pts',(-65.2321284544224,-126.97406767894,180.678881955732));
#35708=CARTESIAN_POINT('Ctrl Pts',(-65.2546302684554,-126.974119287352,
180.660374458958));
#35709=CARTESIAN_POINT('Ctrl Pts',(-65.2705665445107,-126.975135119064,
180.648843498197));
#35710=CARTESIAN_POINT('Ctrl Pts',(-65.3238781506254,-126.98168737182,180.614985522884));
#35711=CARTESIAN_POINT('Ctrl Pts',(-65.3629161670252,-126.991078297533,
180.597125684394));
#35712=CARTESIAN_POINT('Ctrl Pts',(-65.4424529501596,-127.020271879,180.571470229243));
#35713=CARTESIAN_POINT('Ctrl Pts',(-65.4818014512254,-127.039753485866,
180.564068715551));
#35714=CARTESIAN_POINT('Ctrl Pts',(-65.5668985528937,-127.094525058977,
180.556158190988));
#35715=CARTESIAN_POINT('Ctrl Pts',(-65.6100825172251,-127.131678624674,
180.558030957443));
#35716=CARTESIAN_POINT('Ctrl Pts',(-65.6985192966362,-127.230257591184,
180.568433279314));
#35717=CARTESIAN_POINT('Ctrl Pts',(-65.741504002952,-127.297092023592,180.579146620513));
#35718=CARTESIAN_POINT('Ctrl Pts',(-65.8143301227709,-127.461668833645,
180.599286836105));
#35719=CARTESIAN_POINT('Ctrl Pts',(-65.841637631643,-127.562060986139,180.607959273711));
#35720=CARTESIAN_POINT('Ctrl Pts',(-65.8532490850691,-127.67097961421,180.607959273711));
#35721=CARTESIAN_POINT('',(-66.3832791073098,-132.642807062495,180.607959273711));
#35722=CARTESIAN_POINT('',(-65.9592550895172,-128.665345103867,180.607959273711));
#35723=CARTESIAN_POINT('',(-65.7177920353265,-132.713752430417,181.272782863852));
#35724=CARTESIAN_POINT('Ctrl Pts',(-66.3832791073099,-132.642807062495,
180.607959273711));
#35725=CARTESIAN_POINT('Ctrl Pts',(-66.3971540098509,-132.772957466059,
180.607959273711));
#35726=CARTESIAN_POINT('Ctrl Pts',(-66.3866522208333,-132.896475574241,
180.595287990419));
#35727=CARTESIAN_POINT('Ctrl Pts',(-66.3329111114629,-133.089547820342,
180.571541026436));
#35728=CARTESIAN_POINT('Ctrl Pts',(-66.2969737948129,-133.164760017786,
180.56114637845));
#35729=CARTESIAN_POINT('Ctrl Pts',(-66.217495000793,-133.275313464528,180.556839262484));
#35730=CARTESIAN_POINT('Ctrl Pts',(-66.1784699872881,-133.316533485828,
180.559025099194));
#35731=CARTESIAN_POINT('Ctrl Pts',(-66.0993062469322,-133.379575038029,
180.577313542163));
#35732=CARTESIAN_POINT('Ctrl Pts',(-66.0619638370107,-133.402770056673,
180.590447643233));
#35733=CARTESIAN_POINT('Ctrl Pts',(-65.9972913677529,-133.433373350998,
180.623874965741));
#35734=CARTESIAN_POINT('Ctrl Pts',(-65.9706343507697,-133.443165195765,
180.640824418047));
#35735=CARTESIAN_POINT('Ctrl Pts',(-65.9356629787224,-133.45233038878,180.668140611184));
#35736=CARTESIAN_POINT('Ctrl Pts',(-65.9264193731475,-133.454371226774,
180.675882798333));
#35737=CARTESIAN_POINT('Ctrl Pts',(-65.9116185625805,-133.456998533243,
180.689183405137));
#35738=CARTESIAN_POINT('Ctrl Pts',(-65.905941309204,-133.457844223372,180.694513716381));
#35739=CARTESIAN_POINT('Ctrl Pts',(-65.8951997217115,-133.459122838643,
180.705055217748));
#35740=CARTESIAN_POINT('Ctrl Pts',(-65.8901240207468,-133.45958255913,180.710241429858));
#35741=CARTESIAN_POINT('Ctrl Pts',(-65.8786631683877,-133.460276690995,
180.722438860454));
#35742=CARTESIAN_POINT('Ctrl Pts',(-65.8723481874574,-133.460403256164,
180.729522290637));
#35743=CARTESIAN_POINT('Ctrl Pts',(-65.8535392079069,-133.459957966925,
180.751768318165));
#35744=CARTESIAN_POINT('Ctrl Pts',(-65.8416832747013,-133.458507143405,
180.767430113195));
#35745=CARTESIAN_POINT('Ctrl Pts',(-65.8063812423218,-133.450034949769,
180.819520518261));
#35746=CARTESIAN_POINT('Ctrl Pts',(-65.7869438402254,-133.438554467622,
180.857223515098));
#35747=CARTESIAN_POINT('Ctrl Pts',(-65.7569601220642,-133.404078198369,
180.933045220123));
#35748=CARTESIAN_POINT('Ctrl Pts',(-65.7468597828011,-133.381478542051,
180.970056821388));
#35749=CARTESIAN_POINT('Ctrl Pts',(-65.7317433701701,-133.319246559955,
181.048813997606));
#35750=CARTESIAN_POINT('Ctrl Pts',(-65.7289461451197,-133.277787498032,
181.087827728394));
#35751=CARTESIAN_POINT('Ctrl Pts',(-65.7273925282462,-133.169946205937,
181.165383688096));
#35752=CARTESIAN_POINT('Ctrl Pts',(-65.7302815968463,-133.098221322645,
181.201111778045));
#35753=CARTESIAN_POINT('Ctrl Pts',(-65.7317783231141,-132.925721200658,
181.256214102347));
#35754=CARTESIAN_POINT('Ctrl Pts',(-65.7294034887527,-132.822671058489,
181.272782863852));
#35755=CARTESIAN_POINT('Ctrl Pts',(-65.7177920353265,-132.713752430418,
181.272782863852));
#35756=CARTESIAN_POINT('',(-65.2937680175338,-128.736290471789,181.272782863852));
#35757=CARTESIAN_POINT('Origin',(-63.8600385700458,-123.860803419755,182.116582478797));
#35758=CARTESIAN_POINT('',(-63.7970071778021,-127.890188739059,182.216986622987));
#35759=CARTESIAN_POINT('',(-64.6013626382522,-127.804439073161,181.731645524111));
#35760=CARTESIAN_POINT('Ctrl Pts',(-63.7970071778021,-127.890188739059,
182.216986622987));
#35761=CARTESIAN_POINT('Ctrl Pts',(-63.7831322752611,-127.760038335495,
182.216986622987));
#35762=CARTESIAN_POINT('Ctrl Pts',(-63.7637687626661,-127.639704067992,
182.191058057925));
#35763=CARTESIAN_POINT('Ctrl Pts',(-63.7391931903102,-127.454980903388,
182.113583474664));
#35764=CARTESIAN_POINT('Ctrl Pts',(-63.732331258019,-127.384331391819,182.068661603829));
#35765=CARTESIAN_POINT('Ctrl Pts',(-63.7395971786405,-127.281476319828,
181.979636129405));
#35766=CARTESIAN_POINT('Ctrl Pts',(-63.7483486653117,-127.243483658743,
181.93832282765));
#35767=CARTESIAN_POINT('Ctrl Pts',(-63.7810909518899,-127.185390943651,
181.860036293941));
#35768=CARTESIAN_POINT('Ctrl Pts',(-63.801400371884,-127.164011755529,181.824887654503));
#35769=CARTESIAN_POINT('Ctrl Pts',(-63.8476292036524,-127.13537467618,181.767622581437));
#35770=CARTESIAN_POINT('Ctrl Pts',(-63.8699650488265,-127.126043497198,
181.745088167067));
#35771=CARTESIAN_POINT('Ctrl Pts',(-63.9044567280937,-127.116929442638,
181.717151987942));
#35772=CARTESIAN_POINT('Ctrl Pts',(-63.9141070194901,-127.114845249218,
181.709935427865));
#35773=CARTESIAN_POINT('Ctrl Pts',(-63.9304811332893,-127.112050218114,
181.698668259966));
#35774=CARTESIAN_POINT('Ctrl Pts',(-63.9369950016434,-127.111115339238,
181.694419244055));
#35775=CARTESIAN_POINT('Ctrl Pts',(-63.9497849084295,-127.109618359446,
181.686525123085));
#35776=CARTESIAN_POINT('Ctrl Pts',(-63.9560376309646,-127.109033160596,
181.682860169817));
#35777=CARTESIAN_POINT('Ctrl Pts',(-63.9706529689686,-127.108002739486,
181.674739800591));
#35778=CARTESIAN_POINT('Ctrl Pts',(-63.9790759208733,-127.107651450528,
181.670380848498));
#35779=CARTESIAN_POINT('Ctrl Pts',(-64.0053355566674,-127.107302450035,
181.657764531226));
#35780=CARTESIAN_POINT('Ctrl Pts',(-64.0235610596089,-127.108074234866,
181.65033518029));
#35781=CARTESIAN_POINT('Ctrl Pts',(-64.0834180937468,-127.113928701266,
181.629981248421));
#35782=CARTESIAN_POINT('Ctrl Pts',(-64.1256133043086,-127.122983048988,
181.621691915876));
#35783=CARTESIAN_POINT('Ctrl Pts',(-64.2090594419135,-127.151759867151,
181.614968501231));
#35784=CARTESIAN_POINT('Ctrl Pts',(-64.2490983853533,-127.171167868247,
181.616651489296));
#35785=CARTESIAN_POINT('Ctrl Pts',(-64.3338007172831,-127.225981526449,
181.627831658004));
#35786=CARTESIAN_POINT('Ctrl Pts',(-64.3754120789359,-127.263302742097,
181.638983828978));
#35787=CARTESIAN_POINT('Ctrl Pts',(-64.4591344581,-127.362384295172,181.667628094705));
#35788=CARTESIAN_POINT('Ctrl Pts',(-64.4985394316644,-127.429600351007,
181.686563561648));
#35789=CARTESIAN_POINT('Ctrl Pts',(-64.5649845219845,-127.594857421434,
181.71927363754));
#35790=CARTESIAN_POINT('Ctrl Pts',(-64.589751184826,-127.69552044509,181.731645524111));
#35791=CARTESIAN_POINT('Ctrl Pts',(-64.6013626382522,-127.804439073161,
181.731645524111));
#35792=CARTESIAN_POINT('',(-65.1313926604929,-132.776266521447,181.731645524111));
#35793=CARTESIAN_POINT('',(-64.7073686427003,-128.798804562818,181.731645524111));
#35794=CARTESIAN_POINT('',(-64.3270372000429,-132.862016187344,182.216986622987));
#35795=CARTESIAN_POINT('Ctrl Pts',(-65.131392660493,-132.776266521447,181.731645524111));
#35796=CARTESIAN_POINT('Ctrl Pts',(-65.1452675630339,-132.90641692501,181.731645524111));
#35797=CARTESIAN_POINT('Ctrl Pts',(-65.1384611921918,-133.029541076926,
181.71370984535));
#35798=CARTESIAN_POINT('Ctrl Pts',(-65.0925065303848,-133.221783235699,
181.672966271636));
#35799=CARTESIAN_POINT('Ctrl Pts',(-65.0603057116076,-133.296597097505,
181.652413718737));
#35800=CARTESIAN_POINT('Ctrl Pts',(-64.9844740504155,-133.406761735521,
181.62651379162));
#35801=CARTESIAN_POINT('Ctrl Pts',(-64.946176388664,-133.447904216264,181.618303730733));
#35802=CARTESIAN_POINT('Ctrl Pts',(-64.8651281981303,-133.511146663444,
181.6156230735));
#35803=CARTESIAN_POINT('Ctrl Pts',(-64.8258042574373,-133.534552926507,
181.618900819278));
#35804=CARTESIAN_POINT('Ctrl Pts',(-64.7551290646409,-133.565796151265,
181.635190503848));
#35805=CARTESIAN_POINT('Ctrl Pts',(-64.7252345256159,-133.575933137511,
181.645055530873));
#35806=CARTESIAN_POINT('Ctrl Pts',(-64.6847956525423,-133.585681202663,
181.663023413437));
#35807=CARTESIAN_POINT('Ctrl Pts',(-64.6739814951562,-133.587889471973,
181.668289177604));
#35808=CARTESIAN_POINT('Ctrl Pts',(-64.6564488750106,-133.590808007593,
181.67761453307));
#35809=CARTESIAN_POINT('Ctrl Pts',(-64.6496688893713,-133.59177125635,181.681417500627));
#35810=CARTESIAN_POINT('Ctrl Pts',(-64.6367313098051,-133.593283979047,
181.689064102161));
#35811=CARTESIAN_POINT('Ctrl Pts',(-64.6305687016405,-133.593859571103,
181.692880099232));
#35812=CARTESIAN_POINT('Ctrl Pts',(-64.6165366757052,-133.594827807249,
181.701978177925));
#35813=CARTESIAN_POINT('Ctrl Pts',(-64.608717897936,-133.595114687207,181.707349807114));
#35814=CARTESIAN_POINT('Ctrl Pts',(-64.5851541417277,-133.595176288926,
181.724484781102));
#35815=CARTESIAN_POINT('Ctrl Pts',(-64.5699074110674,-133.594086947069,
181.73690695495));
#35816=CARTESIAN_POINT('Ctrl Pts',(-64.5231979042389,-133.586830866421,
181.779297910596));
#35817=CARTESIAN_POINT('Ctrl Pts',(-64.4953117281725,-133.576251080024,
181.811571109155));
#35818=CARTESIAN_POINT('Ctrl Pts',(-64.4480408096231,-133.543617741827,
181.878929055582));
#35819=CARTESIAN_POINT('Ctrl Pts',(-64.4293538988126,-133.521933471402,
181.913034945508));
#35820=CARTESIAN_POINT('Ctrl Pts',(-64.3957395622863,-133.461673491576,
181.98748512713));
#35821=CARTESIAN_POINT('Ctrl Pts',(-64.3836117278628,-133.421209134949,
182.025751312574));
#35822=CARTESIAN_POINT('Ctrl Pts',(-64.3633166551382,-133.315365807257,
182.103419741796));
#35823=CARTESIAN_POINT('Ctrl Pts',(-64.3574009088777,-133.244579576053,
182.140616723261));
#35824=CARTESIAN_POINT('Ctrl Pts',(-64.3452137184365,-133.073538251009,
182.19885018387));
#35825=CARTESIAN_POINT('Ctrl Pts',(-64.3386486534692,-132.970934815416,
182.216986622987));
#35826=CARTESIAN_POINT('Ctrl Pts',(-64.327037200043,-132.862016187345,182.216986622987));
#35827=CARTESIAN_POINT('',(-63.9030131822503,-128.884554228716,182.216986622987));
#35828=CARTESIAN_POINT('Origin',(-62.2947469341107,-124.027673965694,182.8187720491));
#35829=CARTESIAN_POINT('',(-62.2219755900488,-128.058097628933,182.799038162395));
#35830=CARTESIAN_POINT('',(-63.1184532233173,-127.962527123954,182.521385815309));
#35831=CARTESIAN_POINT('Ctrl Pts',(-62.2219755900488,-128.058097628933,
182.799038162395));
#35832=CARTESIAN_POINT('Ctrl Pts',(-62.2081006875078,-127.927947225369,
182.799038162395));
#35833=CARTESIAN_POINT('Ctrl Pts',(-62.1950950874127,-127.806935161917,
182.772307900389));
#35834=CARTESIAN_POINT('Ctrl Pts',(-62.1890962199225,-127.620231596466,
182.69592262965));
#35835=CARTESIAN_POINT('Ctrl Pts',(-62.1929049773309,-127.548444518085,
182.652465491875));
#35836=CARTESIAN_POINT('Ctrl Pts',(-62.220832238708,-127.443386809133,182.570365306765));
#35837=CARTESIAN_POINT('Ctrl Pts',(-62.2390471220705,-127.404385286736,
182.533298893505));
#35838=CARTESIAN_POINT('Ctrl Pts',(-62.2893003618264,-127.344425787048,
182.466552563806));
#35839=CARTESIAN_POINT('Ctrl Pts',(-62.3173249992075,-127.322224105207,
182.437800622955));
#35840=CARTESIAN_POINT('Ctrl Pts',(-62.3757650967539,-127.292285223344,
182.393927007362));
#35841=CARTESIAN_POINT('Ctrl Pts',(-62.402793067364,-127.282453832442,182.377599323219));
#35842=CARTESIAN_POINT('Ctrl Pts',(-62.442913723009,-127.272739691394,182.358914021841));
#35843=CARTESIAN_POINT('Ctrl Pts',(-62.4539976666445,-127.270502661067,
182.354256488759));
#35844=CARTESIAN_POINT('Ctrl Pts',(-62.4725739808559,-127.267472860686,
182.34728413377));
#35845=CARTESIAN_POINT('Ctrl Pts',(-62.4799089580962,-127.266450446118,
182.344732390644));
#35846=CARTESIAN_POINT('Ctrl Pts',(-62.4942053467175,-127.264792865297,
182.340149213999));
#35847=CARTESIAN_POINT('Ctrl Pts',(-62.5011487645808,-127.264134033711,
182.338093546571));
#35848=CARTESIAN_POINT('Ctrl Pts',(-62.517273405508,-127.262942710826,182.333713252777));
#35849=CARTESIAN_POINT('Ctrl Pts',(-62.52649056392,-127.262506754149,182.331494262321));
#35850=CARTESIAN_POINT('Ctrl Pts',(-62.5549969182946,-127.261918238445,
182.32550233905));
#35851=CARTESIAN_POINT('Ctrl Pts',(-62.5744690785897,-127.262557121273,
182.32260636481));
#35852=CARTESIAN_POINT('Ctrl Pts',(-62.6374678225912,-127.268076660412,
182.316939372924));
#35853=CARTESIAN_POINT('Ctrl Pts',(-62.6804510181273,-127.277047003671,
182.318702292201));
#35854=CARTESIAN_POINT('Ctrl Pts',(-62.7631877060839,-127.305899453907,
182.331301658482));
#35855=CARTESIAN_POINT('Ctrl Pts',(-62.8017352151081,-127.325466451876,
182.341971339155));
#35856=CARTESIAN_POINT('Ctrl Pts',(-62.8815112890473,-127.380805282091,
182.371592450366));
#35857=CARTESIAN_POINT('Ctrl Pts',(-62.9193875507362,-127.41852468435,182.391375902221));
#35858=CARTESIAN_POINT('Ctrl Pts',(-62.9941915365654,-127.518556997735,
182.436597411196));
#35859=CARTESIAN_POINT('Ctrl Pts',(-63.0281642013553,-127.586352173978,
182.462654543372));
#35860=CARTESIAN_POINT('Ctrl Pts',(-63.0854224683637,-127.752588621146,
182.506033488849));
#35861=CARTESIAN_POINT('Ctrl Pts',(-63.106841769891,-127.853608495882,182.521385815309));
#35862=CARTESIAN_POINT('Ctrl Pts',(-63.1184532233173,-127.962527123954,
182.521385815309));
#35863=CARTESIAN_POINT('',(-63.6484832455581,-132.93435457224,182.521385815309));
#35864=CARTESIAN_POINT('',(-63.2244592277655,-128.956892613612,182.521385815309));
#35865=CARTESIAN_POINT('',(-62.7520056122895,-133.029925077219,182.799038162395));
#35866=CARTESIAN_POINT('Ctrl Pts',(-63.6484832455581,-132.93435457224,182.521385815309));
#35867=CARTESIAN_POINT('Ctrl Pts',(-63.662358148099,-133.064504975803,182.521385815309));
#35868=CARTESIAN_POINT('Ctrl Pts',(-63.6603925669443,-133.187113067197,
182.499228097533));
#35869=CARTESIAN_POINT('Ctrl Pts',(-63.6260427289545,-133.37811807422,182.443855782497));
#35870=CARTESIAN_POINT('Ctrl Pts',(-63.5998870807864,-133.452287480453,
182.414339764355));
#35871=CARTESIAN_POINT('Ctrl Pts',(-63.532734954993,-133.561526822008,182.368352235708));
#35872=CARTESIAN_POINT('Ctrl Pts',(-63.4976173925097,-133.602330282924,
182.35022341612));
#35873=CARTESIAN_POINT('Ctrl Pts',(-63.4197294693475,-133.665235824488,
182.32672944874));
#35874=CARTESIAN_POINT('Ctrl Pts',(-63.3808270672087,-133.688597148725,
182.319960348555));
#35875=CARTESIAN_POINT('Ctrl Pts',(-63.3084017754703,-133.720026945723,
182.31816569793));
#35876=CARTESIAN_POINT('Ctrl Pts',(-63.2770496520254,-133.730319320205,
182.320372980161));
#35877=CARTESIAN_POINT('Ctrl Pts',(-63.2335267452168,-133.740396163958,
182.327948324127));
#35878=CARTESIAN_POINT('Ctrl Pts',(-63.2217769809352,-133.742704175214,
182.330431638238));
#35879=CARTESIAN_POINT('Ctrl Pts',(-63.2025379122063,-133.745804629654,
182.335239786608));
#35880=CARTESIAN_POINT('Ctrl Pts',(-63.19505069546,-133.746843273971,182.337294395826));
#35881=CARTESIAN_POINT('Ctrl Pts',(-63.1806698266776,-133.748509860941,
182.341601704837));
#35882=CARTESIAN_POINT('Ctrl Pts',(-63.1737779611485,-133.749163196705,
182.343825714991));
#35883=CARTESIAN_POINT('Ctrl Pts',(-63.1579870194791,-133.750318945019,
182.349295694518));
#35884=CARTESIAN_POINT('Ctrl Pts',(-63.1491154950279,-133.750718054807,
182.352643343149));
#35885=CARTESIAN_POINT('Ctrl Pts',(-63.1221513906236,-133.751142156361,
182.363671441191));
#35886=CARTESIAN_POINT('Ctrl Pts',(-63.1043833166242,-133.750321606548,
182.372132062266));
#35887=CARTESIAN_POINT('Ctrl Pts',(-63.0489059670074,-133.744000236518,
182.402359960234));
#35888=CARTESIAN_POINT('Ctrl Pts',(-63.0141086370849,-133.734157225295,
182.427327759524));
#35889=CARTESIAN_POINT('Ctrl Pts',(-62.9520669500268,-133.703098549704,
182.482307348343));
#35890=CARTESIAN_POINT('Ctrl Pts',(-62.9257344419335,-133.682229351028,
182.511525416577));
#35891=CARTESIAN_POINT('Ctrl Pts',(-62.8751846211686,-133.623774806967,
182.577341829662));
#35892=CARTESIAN_POINT('Ctrl Pts',(-62.8541751992229,-133.584257286906,
182.612636578157));
#35893=CARTESIAN_POINT('Ctrl Pts',(-62.8156564992323,-133.480356719631,
182.685903670104));
#35894=CARTESIAN_POINT('Ctrl Pts',(-62.8008422419721,-133.41051912915,182.722407789729));
#35895=CARTESIAN_POINT('Ctrl Pts',(-62.7746236567139,-133.240973644535,
182.780388069585));
#35896=CARTESIAN_POINT('Ctrl Pts',(-62.7636170657158,-133.13884370529,182.799038162395));
#35897=CARTESIAN_POINT('Ctrl Pts',(-62.7520056122896,-133.029925077219,
182.799038162395));
#35898=CARTESIAN_POINT('',(-62.3279815944969,-129.05246311859,182.799038162395));
#35899=CARTESIAN_POINT('Origin',(-60.6078417159259,-124.207509331988,183.123835818113));
#35900=CARTESIAN_POINT('',(-60.554202360699,-128.235893397398,182.985110762277));
#35901=CARTESIAN_POINT('',(-61.490702145304,-128.136056263704,182.931283312168));
#35902=CARTESIAN_POINT('Ctrl Pts',(-60.554202360699,-128.235893397398,182.985110762277));
#35903=CARTESIAN_POINT('Ctrl Pts',(-60.5403274581581,-128.105742993835,
182.985110762277));
#35904=CARTESIAN_POINT('Ctrl Pts',(-60.533685798788,-127.984052491785,182.959132268995));
#35905=CARTESIAN_POINT('Ctrl Pts',(-60.5454646101901,-127.79545370699,182.888275545063));
#35906=CARTESIAN_POINT('Ctrl Pts',(-60.5592854279688,-127.722599276085,
182.848808711235));
#35907=CARTESIAN_POINT('Ctrl Pts',(-60.6056256571204,-127.615578621755,
182.778405179778));
#35908=CARTESIAN_POINT('Ctrl Pts',(-60.6320183277418,-127.575705292601,
182.747739820219));
#35909=CARTESIAN_POINT('Ctrl Pts',(-60.6965274937305,-127.514226015934,
182.696412748599));
#35910=CARTESIAN_POINT('Ctrl Pts',(-60.7305209536102,-127.491388017738,
182.675728464628));
#35911=CARTESIAN_POINT('Ctrl Pts',(-60.7976307515994,-127.460524887886,
182.647796081573));
#35912=CARTESIAN_POINT('Ctrl Pts',(-60.8277375045609,-127.450365278217,
182.63862403331));
#35913=CARTESIAN_POINT('Ctrl Pts',(-60.8711221629394,-127.440303172671,
182.630275531477));
#35914=CARTESIAN_POINT('Ctrl Pts',(-60.8829891348988,-127.437982666293,
182.628447704284));
#35915=CARTESIAN_POINT('Ctrl Pts',(-60.9026816328099,-127.434833873273,
182.626175370134));
#35916=CARTESIAN_POINT('Ctrl Pts',(-60.9104099636905,-127.433769524579,
182.625469197828));
#35917=CARTESIAN_POINT('Ctrl Pts',(-60.9253811622503,-127.43204000451,182.624463323074));
#35918=CARTESIAN_POINT('Ctrl Pts',(-60.9326122477846,-127.431350505628,
182.624136409406));
#35919=CARTESIAN_POINT('Ctrl Pts',(-60.9493123186159,-127.430097838071,
182.623750757796));
#35920=CARTESIAN_POINT('Ctrl Pts',(-60.9587913645781,-127.429633962431,
182.623800688638));
#35921=CARTESIAN_POINT('Ctrl Pts',(-60.9879027632329,-127.428980944964,
182.624781388169));
#35922=CARTESIAN_POINT('Ctrl Pts',(-61.0075065601553,-127.42960579445,182.626587094122));
#35923=CARTESIAN_POINT('Ctrl Pts',(-61.0700607111023,-127.435172730178,
182.635936387187));
#35924=CARTESIAN_POINT('Ctrl Pts',(-61.1114168876027,-127.444316524536,
182.647649103826));
#35925=CARTESIAN_POINT('Ctrl Pts',(-61.1888665524268,-127.473732606759,
182.678839021662));
#35926=CARTESIAN_POINT('Ctrl Pts',(-61.2238274269927,-127.493681963924,
182.697875311885));
#35927=CARTESIAN_POINT('Ctrl Pts',(-61.2944320508974,-127.549998531986,
182.744215894284));
#35928=CARTESIAN_POINT('Ctrl Pts',(-61.3266277857702,-127.588323516354,
182.771480884706));
#35929=CARTESIAN_POINT('Ctrl Pts',(-61.3888276897839,-127.689699509069,
182.830651527203));
#35930=CARTESIAN_POINT('Ctrl Pts',(-61.4158311758153,-127.758237646329,
182.862315978803));
#35931=CARTESIAN_POINT('Ctrl Pts',(-61.461630730476,-127.925695668786,182.913842767231));
#35932=CARTESIAN_POINT('Ctrl Pts',(-61.4790906918778,-128.027137635632,
182.931283312168));
#35933=CARTESIAN_POINT('Ctrl Pts',(-61.490702145304,-128.136056263704,182.931283312168));
#35934=CARTESIAN_POINT('',(-62.0207321675448,-133.107883711989,182.931283312168));
#35935=CARTESIAN_POINT('',(-61.5967081497522,-129.130421753361,182.931283312168));
#35936=CARTESIAN_POINT('',(-61.0842323829398,-133.207720845684,182.985110762277));
#35937=CARTESIAN_POINT('Ctrl Pts',(-62.0207321675448,-133.107883711989,
182.931283312168));
#35938=CARTESIAN_POINT('Ctrl Pts',(-62.0346070700858,-133.238034115553,
182.931283312168));
#35939=CARTESIAN_POINT('Ctrl Pts',(-62.0383463210293,-133.360034033732,
182.906191281395));
#35940=CARTESIAN_POINT('Ctrl Pts',(-62.0187452529312,-133.549466723349,
182.839408262717));
#35941=CARTESIAN_POINT('Ctrl Pts',(-62.000592124765,-133.622783007485,182.802644143018));
#35942=CARTESIAN_POINT('Ctrl Pts',(-61.9466475138939,-133.730614339712,
182.739241640849));
#35943=CARTESIAN_POINT('Ctrl Pts',(-61.9169779823828,-133.770837004128,
182.712247643659));
#35944=CARTESIAN_POINT('Ctrl Pts',(-61.8471113808894,-133.832887419213,
182.669305750119));
#35945=CARTESIAN_POINT('Ctrl Pts',(-61.8110090883418,-133.85595023306,182.652883199469));
#35946=CARTESIAN_POINT('Ctrl Pts',(-61.7411880316488,-133.887102401203,
182.633108512221));
#35947=CARTESIAN_POINT('Ctrl Pts',(-61.7102429709135,-133.897351380082,
182.627529770437));
#35948=CARTESIAN_POINT('Ctrl Pts',(-61.6661987304834,-133.907483801481,
182.62427232435));
#35949=CARTESIAN_POINT('Ctrl Pts',(-61.6542026782984,-133.909818068673,
182.623828867216));
#35950=CARTESIAN_POINT('Ctrl Pts',(-61.6343816945794,-133.912980559139,
182.623840376381));
#35951=CARTESIAN_POINT('Ctrl Pts',(-61.6266238495805,-133.914048054236,
182.624027220841));
#35952=CARTESIAN_POINT('Ctrl Pts',(-61.6116362731618,-133.915779320293,
182.624744912186));
#35953=CARTESIAN_POINT('Ctrl Pts',(-61.6044151818927,-133.91646775372,182.625247684036));
#35954=CARTESIAN_POINT('Ctrl Pts',(-61.5877798041175,-133.917713524565,
182.62677166907));
#35955=CARTESIAN_POINT('Ctrl Pts',(-61.5783677649524,-133.918170256832,
182.627900783973));
#35956=CARTESIAN_POINT('Ctrl Pts',(-61.549555356689,-133.918791399926,182.632181093098));
#35957=CARTESIAN_POINT('Ctrl Pts',(-61.5302819247756,-133.918131331324,
182.636188460856));
#35958=CARTESIAN_POINT('Ctrl Pts',(-61.4691859191854,-133.912408947559,
182.65249656559));
#35959=CARTESIAN_POINT('Ctrl Pts',(-61.4294167066618,-133.903095972238,
182.668707927871));
#35960=CARTESIAN_POINT('Ctrl Pts',(-61.35597910635,-133.873252177133,182.708113945222));
#35961=CARTESIAN_POINT('Ctrl Pts',(-61.3233863095623,-133.853050367057,
182.730746143841));
#35962=CARTESIAN_POINT('Ctrl Pts',(-61.2584476730013,-133.79612976689,182.784103777694));
#35963=CARTESIAN_POINT('Ctrl Pts',(-61.2295218509685,-133.757456187967,
182.814375886748));
#35964=CARTESIAN_POINT('Ctrl Pts',(-61.1743564432734,-133.655330270948,
182.878983624352));
#35965=CARTESIAN_POINT('Ctrl Pts',(-61.1510671279891,-133.586396178273,
182.912673395392));
#35966=CARTESIAN_POINT('Ctrl Pts',(-61.1112851234711,-133.418296644768,
182.967030891378));
#35967=CARTESIAN_POINT('Ctrl Pts',(-61.0958438363661,-133.316639473756,
182.985110762277));
#35968=CARTESIAN_POINT('Ctrl Pts',(-61.0842323829398,-133.207720845684,
182.985110762277));
#35969=CARTESIAN_POINT('',(-60.6602083651472,-129.230258887056,182.985110762277));
#35970=CARTESIAN_POINT('Origin',(-58.8973597151212,-124.389858140823,183.01404458844));
#35971=CARTESIAN_POINT('',(-58.8906124077336,-128.413243200653,182.764390559475));
#35972=CARTESIAN_POINT('',(-59.8127083802321,-128.314941609559,182.937516262089));
#35973=CARTESIAN_POINT('Ctrl Pts',(-58.8906124077336,-128.413243200653,
182.764390559475));
#35974=CARTESIAN_POINT('Ctrl Pts',(-58.8767375051926,-128.28309279709,182.764390559475));
#35975=CARTESIAN_POINT('Ctrl Pts',(-58.8760959656698,-128.160762642177,
182.740673610517));
#35976=CARTESIAN_POINT('Ctrl Pts',(-58.9038202559127,-127.97046396281,182.679463368635));
#35977=CARTESIAN_POINT('Ctrl Pts',(-58.9264126401748,-127.896674424315,
182.646280507681));
#35978=CARTESIAN_POINT('Ctrl Pts',(-58.9878473693628,-127.788044595435,
182.591665227216));
#35979=CARTESIAN_POINT('Ctrl Pts',(-59.02065695454,-127.747487180319,182.569183080593));
#35980=CARTESIAN_POINT('Ctrl Pts',(-59.0953385172016,-127.684923458206,
182.536258209888));
#35981=CARTESIAN_POINT('Ctrl Pts',(-59.1332075184236,-127.661672301411,
182.524843678197));
#35982=CARTESIAN_POINT('Ctrl Pts',(-59.2049416000455,-127.630316192029,
182.514475856253));
#35983=CARTESIAN_POINT('Ctrl Pts',(-59.2363348646342,-127.620019431626,
182.512992489976));
#35984=CARTESIAN_POINT('Ctrl Pts',(-59.2804288601208,-127.609881706005,
182.515465972269));
#35985=CARTESIAN_POINT('Ctrl Pts',(-59.2923827297318,-127.607551935757,
182.516574077638));
#35986=CARTESIAN_POINT('Ctrl Pts',(-59.3120405261043,-127.604406842153,
182.519133824127));
#35987=CARTESIAN_POINT('Ctrl Pts',(-59.3197115950904,-127.603348597959,
182.52031426281));
#35988=CARTESIAN_POINT('Ctrl Pts',(-59.3344867141845,-127.601639981271,
182.52294414773));
#35989=CARTESIAN_POINT('Ctrl Pts',(-59.3415857215319,-127.600964562806,
182.524364986856));
#35990=CARTESIAN_POINT('Ctrl Pts',(-59.3578939073577,-127.599753672809,
182.527996390102));
#35991=CARTESIAN_POINT('Ctrl Pts',(-59.3670873019613,-127.599320249513,
182.530312340441));
#35992=CARTESIAN_POINT('Ctrl Pts',(-59.3951269076186,-127.59878149234,182.538208668082));
#35993=CARTESIAN_POINT('Ctrl Pts',(-59.4137396701984,-127.599511992707,
182.544611113162));
#35994=CARTESIAN_POINT('Ctrl Pts',(-59.4722887633093,-127.605505894358,
182.568433344249));
#35995=CARTESIAN_POINT('Ctrl Pts',(-59.5096974731965,-127.61507051503,182.589415157732));
#35996=CARTESIAN_POINT('Ctrl Pts',(-59.5775898039698,-127.645505472915,
182.637382982469));
#35997=CARTESIAN_POINT('Ctrl Pts',(-59.6070772861928,-127.66603833027,182.66367956225));
#35998=CARTESIAN_POINT('Ctrl Pts',(-59.6647982793581,-127.723728379444,
182.724046469628));
#35999=CARTESIAN_POINT('Ctrl Pts',(-59.6896981921335,-127.76283114719,182.757208456479));
#36000=CARTESIAN_POINT('Ctrl Pts',(-59.7363408292674,-127.86586564849,182.82688944983));
#36001=CARTESIAN_POINT('Ctrl Pts',(-59.7552432898956,-127.935267409179,
182.862320998025));
#36002=CARTESIAN_POINT('Ctrl Pts',(-59.7879781818845,-128.104118211964,
182.919001079751));
#36003=CARTESIAN_POINT('Ctrl Pts',(-59.801096926806,-128.206022981489,182.937516262089));
#36004=CARTESIAN_POINT('Ctrl Pts',(-59.8127083802321,-128.314941609559,
182.937516262089));
#36005=CARTESIAN_POINT('',(-60.3427384024728,-133.286769057844,182.937516262089));
#36006=CARTESIAN_POINT('',(-59.9187143846802,-129.309307099216,182.937516262089));
#36007=CARTESIAN_POINT('',(-59.4206424299744,-133.385070648939,182.764390559475));
#36008=CARTESIAN_POINT('Ctrl Pts',(-60.3427384024729,-133.286769057844,
182.937516262089));
#36009=CARTESIAN_POINT('Ctrl Pts',(-60.3566133050138,-133.416919461408,
182.937516262089));
#36010=CARTESIAN_POINT('Ctrl Pts',(-60.3665898863617,-133.538254438495,
182.910948175941));
#36011=CARTESIAN_POINT('Ctrl Pts',(-60.3640243893328,-133.725871022423,
182.836635639919));
#36012=CARTESIAN_POINT('Ctrl Pts',(-60.3553660531873,-133.798175098296,
182.79476001567));
#36013=CARTESIAN_POINT('Ctrl Pts',(-60.3183893640027,-133.90419753671,182.717627262946));
#36014=CARTESIAN_POINT('Ctrl Pts',(-60.2961191754112,-133.943631381737,
182.683336881151));
#36015=CARTESIAN_POINT('Ctrl Pts',(-60.2386687798237,-134.004358146321,
182.623442688217));
#36016=CARTESIAN_POINT('Ctrl Pts',(-60.2075824357135,-134.026886226554,
182.598321106052));
#36017=CARTESIAN_POINT('Ctrl Pts',(-60.144568599377,-134.057312699529,182.561715615124));
#36018=CARTESIAN_POINT('Ctrl Pts',(-60.1158715914763,-134.067322020956,
182.548675065521));
#36019=CARTESIAN_POINT('Ctrl Pts',(-60.0738990155605,-134.077233589078,
182.534774140307));
#36020=CARTESIAN_POINT('Ctrl Pts',(-60.0623603078181,-134.079519100297,
182.531429684044));
#36021=CARTESIAN_POINT('Ctrl Pts',(-60.0431157614817,-134.082620138686,
182.526643885133));
#36022=CARTESIAN_POINT('Ctrl Pts',(-60.0355396190153,-134.083668263079,
182.524952106114));
#36023=CARTESIAN_POINT('Ctrl Pts',(-60.020817176179,-134.085371264126,182.522038470182));
#36024=CARTESIAN_POINT('Ctrl Pts',(-60.0136860241933,-134.086050109424,
182.520790784457));
#36025=CARTESIAN_POINT('Ctrl Pts',(-59.9971697655067,-134.087283181378,
182.518280206525));
#36026=CARTESIAN_POINT('Ctrl Pts',(-59.9877608563466,-134.087739579966,
182.517125167646));
#36027=CARTESIAN_POINT('Ctrl Pts',(-59.9587596052638,-134.088380854966,
182.514408931845));
#36028=CARTESIAN_POINT('Ctrl Pts',(-59.9390842867924,-134.087763630156,
182.513730152639));
#36029=CARTESIAN_POINT('Ctrl Pts',(-59.8758453479046,-134.082269697397,
182.51517069637));
#36030=CARTESIAN_POINT('Ctrl Pts',(-59.8333324717794,-134.073249214946,
182.521683476191));
#36031=CARTESIAN_POINT('Ctrl Pts',(-59.7525361025255,-134.044189913774,
182.54322578758));
#36032=CARTESIAN_POINT('Ctrl Pts',(-59.715432150855,-134.024469022947,182.557956815466));
#36033=CARTESIAN_POINT('Ctrl Pts',(-59.6394875926139,-133.96872172756,182.595754718354));
#36034=CARTESIAN_POINT('Ctrl Pts',(-59.6040706303263,-133.930740147556,
182.619244883024));
#36035=CARTESIAN_POINT('Ctrl Pts',(-59.5348028806321,-133.830117634411,
182.671438499415));
#36036=CARTESIAN_POINT('Ctrl Pts',(-59.5039544998657,-133.761989388618,
182.700355994833));
#36037=CARTESIAN_POINT('Ctrl Pts',(-59.4518653082704,-133.595201883477,
182.747931646866));
#36038=CARTESIAN_POINT('Ctrl Pts',(-59.4322538834007,-133.493989277011,
182.764390559475));
#36039=CARTESIAN_POINT('Ctrl Pts',(-59.4206424299744,-133.385070648939,
182.764390559475));
#36040=CARTESIAN_POINT('',(-58.9966184121818,-129.40760869031,182.764390559475));
#36041=CARTESIAN_POINT('Origin',(-57.2627079282344,-124.564122942241,182.495779027277));
#36042=CARTESIAN_POINT('',(-57.3278875323155,-128.579840112772,182.14970500989));
#36043=CARTESIAN_POINT('',(-58.1819908264683,-128.488786995442,182.539722428676));
#36044=CARTESIAN_POINT('Ctrl Pts',(-57.3278875323155,-128.579840112772,
182.14970500989));
#36045=CARTESIAN_POINT('Ctrl Pts',(-57.3140126297744,-128.449689709208,
182.14970500989));
#36046=CARTESIAN_POINT('Ctrl Pts',(-57.3186586840651,-128.32679586147,182.129627948123));
#36047=CARTESIAN_POINT('Ctrl Pts',(-57.3595695598265,-128.135091403988,
182.081621505058));
#36048=CARTESIAN_POINT('Ctrl Pts',(-57.3891832451256,-128.060553347895,
182.056651084241));
#36049=CARTESIAN_POINT('Ctrl Pts',(-57.4615167691348,-127.950761634673,
182.020998096351));
#36050=CARTESIAN_POINT('Ctrl Pts',(-57.4986094684153,-127.909747610979,
182.008005743306));
#36051=CARTESIAN_POINT('Ctrl Pts',(-57.5787887154705,-127.846597798979,
181.995396547325));
#36052=CARTESIAN_POINT('Ctrl Pts',(-57.6182147445026,-127.823180652617,
181.993915139005));
#36053=CARTESIAN_POINT('Ctrl Pts',(-57.6902589463901,-127.791791482344,
182.001714418298));
#36054=CARTESIAN_POINT('Ctrl Pts',(-57.7210716845023,-127.781556609941,
182.008005941864));
#36055=CARTESIAN_POINT('Ctrl Pts',(-57.7632791273821,-127.771620003432,
182.021157658483));
#36056=CARTESIAN_POINT('Ctrl Pts',(-57.7746187137944,-127.769355719877,
182.025137297357));
#36057=CARTESIAN_POINT('Ctrl Pts',(-57.7930929401046,-127.766336802749,
182.032380361324));
#36058=CARTESIAN_POINT('Ctrl Pts',(-57.8002594595197,-127.76533234691,182.035378808189));
#36059=CARTESIAN_POINT('Ctrl Pts',(-57.8139790051779,-127.763736261403,
182.041491613433));
#36060=CARTESIAN_POINT('Ctrl Pts',(-57.8205338643875,-127.763118852765,
182.044577631346));
#36061=CARTESIAN_POINT('Ctrl Pts',(-57.8355056252227,-127.7620504346,182.052015045491));
#36062=CARTESIAN_POINT('Ctrl Pts',(-57.843882430576,-127.761704065173,182.056462420712));
#36063=CARTESIAN_POINT('Ctrl Pts',(-57.8692356946754,-127.761451689958,
182.070815470603));
#36064=CARTESIAN_POINT('Ctrl Pts',(-57.8857923472572,-127.762401385387,
182.081442567973));
#36065=CARTESIAN_POINT('Ctrl Pts',(-57.9370086771498,-127.769177008587,
182.118353275601));
#36066=CARTESIAN_POINT('Ctrl Pts',(-57.9683788852572,-127.779385373891,
182.147384799195));
#36067=CARTESIAN_POINT('Ctrl Pts',(-58.0229990085785,-127.81123523776,182.209342815215));
#36068=CARTESIAN_POINT('Ctrl Pts',(-58.0454444342418,-127.832518825392,
182.24137142292));
#36069=CARTESIAN_POINT('Ctrl Pts',(-58.0873183657515,-127.891898277211,
182.312256350047));
#36070=CARTESIAN_POINT('Ctrl Pts',(-58.1037311678091,-127.931905827661,
182.349388079189));
#36071=CARTESIAN_POINT('Ctrl Pts',(-58.1327674848055,-128.036817280314,
182.425529817342));
#36072=CARTESIAN_POINT('Ctrl Pts',(-58.1429078755347,-128.107153136193,
182.462669309337));
#36073=CARTESIAN_POINT('Ctrl Pts',(-58.1617314252332,-128.277486981004,
182.521208644037));
#36074=CARTESIAN_POINT('Ctrl Pts',(-58.1703793730421,-128.379868367371,
182.539722428676));
#36075=CARTESIAN_POINT('Ctrl Pts',(-58.1819908264683,-128.488786995442,
182.539722428676));
#36076=CARTESIAN_POINT('',(-58.712020848709,-133.460614443727,182.539722428676));
#36077=CARTESIAN_POINT('',(-58.2879968309164,-129.483152485099,182.539722428676));
#36078=CARTESIAN_POINT('',(-57.8579175545562,-133.551667561058,182.14970500989));
#36079=CARTESIAN_POINT('Ctrl Pts',(-58.712020848709,-133.460614443727,182.539722428676));
#36080=CARTESIAN_POINT('Ctrl Pts',(-58.72589575125,-133.590764847291,182.539722428676));
#36081=CARTESIAN_POINT('Ctrl Pts',(-58.7422796703366,-133.711416759368,
182.513222327751));
#36082=CARTESIAN_POINT('Ctrl Pts',(-58.7580465000861,-133.897078994785,
182.435699048863));
#36083=CARTESIAN_POINT('Ctrl Pts',(-58.7598234251794,-133.968270602094,
182.391145579132));
#36084=CARTESIAN_POINT('Ctrl Pts',(-58.7425889505126,-134.072188388545,
182.304765251075));
#36085=CARTESIAN_POINT('Ctrl Pts',(-58.7292393938724,-134.110671234608,
182.265171317025));
#36086=CARTESIAN_POINT('Ctrl Pts',(-58.6878785036726,-134.169682750425,
182.191805657483));
#36087=CARTESIAN_POINT('Ctrl Pts',(-58.6637324381542,-134.191470950593,
182.159445018846));
#36088=CARTESIAN_POINT('Ctrl Pts',(-58.6113331965825,-134.220765836851,
182.108136102317));
#36089=CARTESIAN_POINT('Ctrl Pts',(-58.5865945829816,-134.230353167,182.088391614236));
#36090=CARTESIAN_POINT('Ctrl Pts',(-58.549166272102,-134.239780286109,182.064655081141));
#36091=CARTESIAN_POINT('Ctrl Pts',(-58.5387619619532,-134.241944862965,
182.058603993391));
#36092=CARTESIAN_POINT('Ctrl Pts',(-58.5212187049274,-134.244864532549,
182.049299019641));
#36093=CARTESIAN_POINT('Ctrl Pts',(-58.5142660358884,-134.245846190509,
182.045826937191));
#36094=CARTESIAN_POINT('Ctrl Pts',(-58.5006651592581,-134.247429625105,
182.039451303911));
#36095=CARTESIAN_POINT('Ctrl Pts',(-58.4940378846398,-134.248054753709,
182.036525671569));
#36096=CARTESIAN_POINT('Ctrl Pts',(-58.4785973774569,-134.249173143366,
182.030126436336));
#36097=CARTESIAN_POINT('Ctrl Pts',(-58.469735061115,-134.249571271508,182.026754370336));
#36098=CARTESIAN_POINT('Ctrl Pts',(-58.4422154031119,-134.250054598787,
182.017199447361));
#36099=CARTESIAN_POINT('Ctrl Pts',(-58.4232650256236,-134.249360090425,
182.01187396937));
#36100=CARTESIAN_POINT('Ctrl Pts',(-58.361483415609,-134.243710796672,181.998363232933));
#36101=CARTESIAN_POINT('Ctrl Pts',(-58.318614546638,-134.234728265437,181.994798931204));
#36102=CARTESIAN_POINT('Ctrl Pts',(-58.2349242176556,-134.205977479706,
181.997225575798));
#36103=CARTESIAN_POINT('Ctrl Pts',(-58.1953204168388,-134.186523089499,
182.003199319155));
#36104=CARTESIAN_POINT('Ctrl Pts',(-58.1123924551955,-134.13152027157,182.023240814352));
#36105=CARTESIAN_POINT('Ctrl Pts',(-58.0722868539636,-134.094038531801,
182.03858387165));
#36106=CARTESIAN_POINT('Ctrl Pts',(-57.9922807048315,-133.994560803777,
182.07533006356));
#36107=CARTESIAN_POINT('Ctrl Pts',(-57.9552285565356,-133.927093921049,
182.097794703633));
#36108=CARTESIAN_POINT('Ctrl Pts',(-57.8928036590256,-133.761408271211,
182.135823587746));
#36109=CARTESIAN_POINT('Ctrl Pts',(-57.8695290079825,-133.660586189129,
182.14970500989));
#36110=CARTESIAN_POINT('Ctrl Pts',(-57.8579175545563,-133.551667561058,
182.14970500989));
#36111=CARTESIAN_POINT('',(-57.4338935367636,-129.57420560243,182.14970500989));
#36112=CARTESIAN_POINT('Origin',(-60.6261834003547,-128.228219737673,175.985485069079));
#36113=CARTESIAN_POINT('',(-56.8563447552978,-127.624443285184,171.250110682016));
#36114=CARTESIAN_POINT('Origin',(-60.5201773959065,-127.233854248016,175.985485069079));
#36115=CARTESIAN_POINT('',(-56.3517119863112,-128.683906947702,170.460881617506));
#36116=CARTESIAN_POINT('Origin',(-56.9623507597459,-128.618808774841,171.250110682016));
#36117=CARTESIAN_POINT('',(-56.6510041624572,-128.652000402186,170.239324614047));
#36118=CARTESIAN_POINT('Origin',(-60.6261834003547,-128.228219737673,175.985485069079));
#36119=CARTESIAN_POINT('',(-57.4553596229072,-128.566250736288,169.753983515172));
#36120=CARTESIAN_POINT('Ctrl Pts',(-57.4553596229072,-128.566250736288,
169.753983515172));
#36121=CARTESIAN_POINT('Ctrl Pts',(-57.4414847203663,-128.436100332725,
169.753983515172));
#36122=CARTESIAN_POINT('Ctrl Pts',(-57.4350444863886,-128.314388357382,
169.779912080233));
#36123=CARTESIAN_POINT('Ctrl Pts',(-57.4201248720071,-128.128635803146,
169.857386663495));
#36124=CARTESIAN_POINT('Ctrl Pts',(-57.4119384373763,-128.058127492375,
169.90230853433));
#36125=CARTESIAN_POINT('Ctrl Pts',(-57.3831521735925,-127.959115824103,
169.991334008754));
#36126=CARTESIAN_POINT('Ctrl Pts',(-57.3665878576303,-127.923821996711,
170.032647310509));
#36127=CARTESIAN_POINT('Ctrl Pts',(-57.3223344824676,-127.873937533561,
170.110933844218));
#36128=CARTESIAN_POINT('Ctrl Pts',(-57.2979744020772,-127.857320412612,
170.146082483655));
#36129=CARTESIAN_POINT('Ctrl Pts',(-57.2467473469839,-127.839072781895,
170.203347556721));
#36130=CARTESIAN_POINT('Ctrl Pts',(-57.222946314663,-127.834660102289,170.225881971091));
#36131=CARTESIAN_POINT('Ctrl Pts',(-57.1873084187118,-127.833022328976,
170.253818150217));
#36132=CARTESIAN_POINT('Ctrl Pts',(-57.1774356289432,-127.83301942644,170.261034710294));
#36133=CARTESIAN_POINT('Ctrl Pts',(-57.1608402746568,-127.833739160899,
170.272301878193));
#36134=CARTESIAN_POINT('Ctrl Pts',(-57.1542757137794,-127.834198529955,
170.276550894104));
#36135=CARTESIAN_POINT('Ctrl Pts',(-57.1414576649162,-127.835431529319,
170.284445015073));
#36136=CARTESIAN_POINT('Ctrl Pts',(-57.1352220993665,-127.836177665411,
170.288109968341));
#36137=CARTESIAN_POINT('Ctrl Pts',(-57.1207180037226,-127.838251570473,
170.296230337568));
#36138=CARTESIAN_POINT('Ctrl Pts',(-57.1124102960038,-127.839683881607,
170.300589289661));
#36139=CARTESIAN_POINT('Ctrl Pts',(-57.0866672582166,-127.844878713541,
170.313205606933));
#36140=CARTESIAN_POINT('Ctrl Pts',(-57.0690140708695,-127.849475406459,
170.320634957869));
#36141=CARTESIAN_POINT('Ctrl Pts',(-57.0117365199272,-127.867817202192,
170.340988889737));
#36142=CARTESIAN_POINT('Ctrl Pts',(-56.9723984418365,-127.8855635432,170.349278222282));
#36143=CARTESIAN_POINT('Ctrl Pts',(-56.8968943729927,-127.9312855153,170.356001636928));
#36144=CARTESIAN_POINT('Ctrl Pts',(-56.8618468314437,-127.95869823734,170.354318648863));
#36145=CARTESIAN_POINT('Ctrl Pts',(-56.7906038202443,-128.030136710975,
170.343138480155));
#36146=CARTESIAN_POINT('Ctrl Pts',(-56.7577956176336,-128.075391549363,
170.33198630918));
#36147=CARTESIAN_POINT('Ctrl Pts',(-56.6968429788158,-128.189896425913,
170.303342043454));
#36148=CARTESIAN_POINT('Ctrl Pts',(-56.6724939299533,-128.263909086473,
170.284406576511));
#36149=CARTESIAN_POINT('Ctrl Pts',(-56.6423812329264,-128.439459862121,
170.251696500619));
#36150=CARTESIAN_POINT('Ctrl Pts',(-56.6393927090308,-128.543081774113,
170.239324614047));
#36151=CARTESIAN_POINT('Ctrl Pts',(-56.6510041624572,-128.652000402186,
170.239324614047));
#36152=CARTESIAN_POINT('',(-58.1339135773921,-128.493912351392,169.44958432285));
#36153=CARTESIAN_POINT('Origin',(-60.6261834003547,-128.228219737673,175.985485069079));
#36154=CARTESIAN_POINT('',(-59.0303912106606,-128.398341846414,169.171931975764));
#36155=CARTESIAN_POINT('Ctrl Pts',(-59.0303912106606,-128.398341846414,
169.171931975764));
#36156=CARTESIAN_POINT('Ctrl Pts',(-59.0165163081196,-128.26819144285,169.171931975764));
#36157=CARTESIAN_POINT('Ctrl Pts',(-59.0037181616419,-128.147157263456,
169.198662237769));
#36158=CARTESIAN_POINT('Ctrl Pts',(-58.9702218423946,-127.963385110068,
169.27504750851));
#36159=CARTESIAN_POINT('Ctrl Pts',(-58.951364718064,-127.894014366109,169.318504646285));
#36160=CARTESIAN_POINT('Ctrl Pts',(-58.9019171135249,-127.797205334798,
169.400604831394));
#36161=CARTESIAN_POINT('Ctrl Pts',(-58.8758894008713,-127.762920368717,
169.437671244654));
#36162=CARTESIAN_POINT('Ctrl Pts',(-58.8141250725308,-127.714902690165,
169.504417574353));
#36163=CARTESIAN_POINT('Ctrl Pts',(-58.7820497747533,-127.699108062934,
169.533169515204));
#36164=CARTESIAN_POINT('Ctrl Pts',(-58.7186114538819,-127.682162234731,
169.577043130797));
#36165=CARTESIAN_POINT('Ctrl Pts',(-58.6901182961251,-127.678249767044,
169.59337081494));
#36166=CARTESIAN_POINT('Ctrl Pts',(-58.6488514237962,-127.677212080219,
169.612056116318));
#36167=CARTESIAN_POINT('Ctrl Pts',(-58.6375449817886,-127.67736201459,169.6167136494));
#36168=CARTESIAN_POINT('Ctrl Pts',(-58.618747427092,-127.678316518326,169.623686004388));
#36169=CARTESIAN_POINT('Ctrl Pts',(-58.6113617573274,-127.678863423075,
169.626237747514));
#36170=CARTESIAN_POINT('Ctrl Pts',(-58.5970372266283,-127.680257023467,
169.63082092416));
#36171=CARTESIAN_POINT('Ctrl Pts',(-58.5901109657506,-127.681076792296,
169.632876591588));
#36172=CARTESIAN_POINT('Ctrl Pts',(-58.5740975671833,-127.683311599132,
169.637256885382));
#36173=CARTESIAN_POINT('Ctrl Pts',(-58.5649956529573,-127.684828577986,
169.639475875838));
#36174=CARTESIAN_POINT('Ctrl Pts',(-58.5370058965889,-127.690262925132,
169.645467799109));
#36175=CARTESIAN_POINT('Ctrl Pts',(-58.5181060518879,-127.694992520052,
169.648363773348));
#36176=CARTESIAN_POINT('Ctrl Pts',(-58.4576867910827,-127.713669243046,
169.654030765235));
#36177=CARTESIAN_POINT('Ctrl Pts',(-58.4175607280179,-127.731499588516,
169.652267845958));
#36178=CARTESIAN_POINT('Ctrl Pts',(-58.3427661088215,-127.777145928544,
169.639668479677));
#36179=CARTESIAN_POINT('Ctrl Pts',(-58.309210001688,-127.804399653713,169.628998799003));
#36180=CARTESIAN_POINT('Ctrl Pts',(-58.2428932484799,-127.875312955333,
169.599377687793));
#36181=CARTESIAN_POINT('Ctrl Pts',(-58.2138201458332,-127.920169607111,
169.579594235938));
#36182=CARTESIAN_POINT('Ctrl Pts',(-58.1617859003498,-128.033723723348,
169.534372726963));
#36183=CARTESIAN_POINT('Ctrl Pts',(-58.142869160262,-128.1071572635,169.508315594787));
#36184=CARTESIAN_POINT('Ctrl Pts',(-58.1219432865466,-128.28172866241,169.464936649309));
#36185=CARTESIAN_POINT('Ctrl Pts',(-58.122302123966,-128.384993723323,169.44958432285));
#36186=CARTESIAN_POINT('Ctrl Pts',(-58.1339135773921,-128.493912351392,
169.44958432285));
#36187=CARTESIAN_POINT('',(-59.7616646554053,-128.320383211643,169.03968682599));
#36188=CARTESIAN_POINT('Origin',(-60.6261834003547,-128.228219737673,175.985485069079));
#36189=CARTESIAN_POINT('',(-60.6981644400103,-128.220546077948,168.985859375881));
#36190=CARTESIAN_POINT('Ctrl Pts',(-60.6981644400103,-128.220546077948,
168.985859375881));
#36191=CARTESIAN_POINT('Ctrl Pts',(-60.6842895374694,-128.090395674385,
168.985859375881));
#36192=CARTESIAN_POINT('Ctrl Pts',(-60.6651274502667,-127.970039933589,
169.011837869164));
#36193=CARTESIAN_POINT('Ctrl Pts',(-60.6138534521269,-127.788162999541,
169.082694593096));
#36194=CARTESIAN_POINT('Ctrl Pts',(-60.5849842674264,-127.719859608108,
169.122161426924));
#36195=CARTESIAN_POINT('Ctrl Pts',(-60.5171236951126,-127.625013522177,
169.192564958381));
#36196=CARTESIAN_POINT('Ctrl Pts',(-60.4829181952001,-127.591600362852,
169.22323031794));
#36197=CARTESIAN_POINT('Ctrl Pts',(-60.4068979406267,-127.545102461279,
169.27455738956));
#36198=CARTESIAN_POINT('Ctrl Pts',(-60.3688538203507,-127.529944150403,
169.295241673531));
#36199=CARTESIAN_POINT('Ctrl Pts',(-60.2967457990367,-127.513922570189,
169.323174056586));
#36200=CARTESIAN_POINT('Ctrl Pts',(-60.2651738589284,-127.51033832127,169.332346104849));
#36201=CARTESIAN_POINT('Ctrl Pts',(-60.2206429838666,-127.509648598942,
169.340694606682));
#36202=CARTESIAN_POINT('Ctrl Pts',(-60.2085535135348,-127.509882009364,
169.342522433874));
#36203=CARTESIAN_POINT('Ctrl Pts',(-60.1886397751368,-127.510955505739,
169.344794768025));
#36204=CARTESIAN_POINT('Ctrl Pts',(-60.1808607517325,-127.511544344614,
169.34550094033));
#36205=CARTESIAN_POINT('Ctrl Pts',(-60.1658614110955,-127.513009884254,
169.346506815085));
#36206=CARTESIAN_POINT('Ctrl Pts',(-60.1586474825466,-127.513860320379,
169.346833728753));
#36207=CARTESIAN_POINT('Ctrl Pts',(-60.1420586540755,-127.516156471887,
169.347219380362));
#36208=CARTESIAN_POINT('Ctrl Pts',(-60.1326948522994,-127.517701369704,
169.347169449521));
#36209=CARTESIAN_POINT('Ctrl Pts',(-60.104100051651,-127.523200218612,169.34618874999));
#36210=CARTESIAN_POINT('Ctrl Pts',(-60.0850685703232,-127.527943846876,
169.344383044037));
#36211=CARTESIAN_POINT('Ctrl Pts',(-60.0250939025714,-127.54657317328,169.335033750972));
#36212=CARTESIAN_POINT('Ctrl Pts',(-59.9865948585421,-127.564230067651,
169.323321034333));
#36213=CARTESIAN_POINT('Ctrl Pts',(-59.9170872624789,-127.609312775691,
169.292131116497));
#36214=CARTESIAN_POINT('Ctrl Pts',(-59.8871177898037,-127.636184141664,
169.273094826274));
#36215=CARTESIAN_POINT('Ctrl Pts',(-59.8299724866298,-127.706119705437,
169.226754243875));
#36216=CARTESIAN_POINT('Ctrl Pts',(-59.806579910799,-127.750370775105,169.199489253453));
#36217=CARTESIAN_POINT('Ctrl Pts',(-59.7671497471324,-127.862581212014,
169.140318610957));
#36218=CARTESIAN_POINT('Ctrl Pts',(-59.7552021858026,-127.93527179115,169.108654159356));
#36219=CARTESIAN_POINT('Ctrl Pts',(-59.7457350244345,-128.108621614768,
169.057127370928));
#36220=CARTESIAN_POINT('Ctrl Pts',(-59.750053201979,-128.211464583572,169.03968682599));
#36221=CARTESIAN_POINT('Ctrl Pts',(-59.7616646554053,-128.320383211643,
169.03968682599));
#36222=CARTESIAN_POINT('',(-61.4396584204773,-128.141497865788,169.03345387607));
#36223=CARTESIAN_POINT('Origin',(-60.6261834003547,-128.228219737673,175.985485069079));
#36224=CARTESIAN_POINT('',(-62.3617543929757,-128.043196274694,169.206579578684));
#36225=CARTESIAN_POINT('Ctrl Pts',(-62.3617543929757,-128.043196274694,
169.206579578684));
#36226=CARTESIAN_POINT('Ctrl Pts',(-62.3478794904347,-127.913045871129,
169.206579578684));
#36227=CARTESIAN_POINT('Ctrl Pts',(-62.3227172833847,-127.793329783196,
169.230296527642));
#36228=CARTESIAN_POINT('Ctrl Pts',(-62.2554978064046,-127.613152743724,
169.291506769524));
#36229=CARTESIAN_POINT('Ctrl Pts',(-62.2178570552205,-127.545784459879,
169.324689630478));
#36230=CARTESIAN_POINT('Ctrl Pts',(-62.1349019828699,-127.452547548496,
169.379304910943));
#36231=CARTESIAN_POINT('Ctrl Pts',(-62.0942795684017,-127.419818475134,
169.401787057566));
#36232=CARTESIAN_POINT('Ctrl Pts',(-62.0080869171554,-127.374405019007,
169.434711928271));
#36233=CARTESIAN_POINT('Ctrl Pts',(-61.966167255537,-127.35965986673,169.446126459962));
#36234=CARTESIAN_POINT('Ctrl Pts',(-61.8894349505906,-127.344131266045,
169.456494281906));
#36235=CARTESIAN_POINT('Ctrl Pts',(-61.856576498855,-127.340684167861,169.457977648183));
#36236=CARTESIAN_POINT('Ctrl Pts',(-61.8113362866851,-127.340070065608,
169.45550416589));
#36237=CARTESIAN_POINT('Ctrl Pts',(-61.7991599187017,-127.3403127399,169.454396060521));
#36238=CARTESIAN_POINT('Ctrl Pts',(-61.7792808818439,-127.341382536859,
169.451836314032));
#36239=CARTESIAN_POINT('Ctrl Pts',(-61.7715591203334,-127.341965271234,
169.450655875349));
#36240=CARTESIAN_POINT('Ctrl Pts',(-61.756755859161,-127.343409907493,169.448025990428));
#36241=CARTESIAN_POINT('Ctrl Pts',(-61.7496740087988,-127.344246263201,
169.446605151303));
#36242=CARTESIAN_POINT('Ctrl Pts',(-61.7334770653336,-127.346500637149,
169.442973748057));
#36243=CARTESIAN_POINT('Ctrl Pts',(-61.7243989149161,-127.348015082622,
169.440657797718));
#36244=CARTESIAN_POINT('Ctrl Pts',(-61.6968759072649,-127.353399671236,
169.432761470076));
#36245=CARTESIAN_POINT('Ctrl Pts',(-61.6788354602793,-127.358037648619,
169.426359024997));
#36246=CARTESIAN_POINT('Ctrl Pts',(-61.6228658503647,-127.3762400091,169.40253679391));
#36247=CARTESIAN_POINT('Ctrl Pts',(-61.5883142729488,-127.393476077158,
169.381554980426));
#36248=CARTESIAN_POINT('Ctrl Pts',(-61.5283640109359,-127.437539909536,
169.333587155689));
#36249=CARTESIAN_POINT('Ctrl Pts',(-61.5038679306038,-127.463827775318,
169.307290575909));
#36250=CARTESIAN_POINT('Ctrl Pts',(-61.4596062581692,-127.532389857981,
169.24692366853));
#36251=CARTESIAN_POINT('Ctrl Pts',(-61.443509504436,-127.575863144271,169.213761681679));
#36252=CARTESIAN_POINT('Ctrl Pts',(-61.4196366076484,-127.686415072594,
169.144080688328));
#36253=CARTESIAN_POINT('Ctrl Pts',(-61.4157900717221,-127.7582420283,169.108649140134));
#36254=CARTESIAN_POINT('Ctrl Pts',(-61.4193875730265,-127.930199071595,
169.051969058407));
#36255=CARTESIAN_POINT('Ctrl Pts',(-61.4280469670512,-128.032579237718,
169.03345387607));
#36256=CARTESIAN_POINT('Ctrl Pts',(-61.4396584204773,-128.141497865788,
169.03345387607));
#36257=CARTESIAN_POINT('',(-63.0703759742411,-127.967652479905,169.431247709482));
#36258=CARTESIAN_POINT('Origin',(-60.6261834003547,-128.228219737673,175.985485069079));
#36259=CARTESIAN_POINT('',(-63.9244792683939,-127.876599362575,169.821265128268));
#36260=CARTESIAN_POINT('Ctrl Pts',(-63.9244792683939,-127.876599362574,
169.821265128269));
#36261=CARTESIAN_POINT('Ctrl Pts',(-63.9106043658529,-127.746448959011,
169.821265128269));
#36262=CARTESIAN_POINT('Ctrl Pts',(-63.8801545649898,-127.627296563903,
169.841342190036));
#36263=CARTESIAN_POINT('Ctrl Pts',(-63.7997485024906,-127.448525302545,
169.889348633101));
#36264=CARTESIAN_POINT('Ctrl Pts',(-63.7550864502697,-127.3819055363,169.914319053918));
#36265=CARTESIAN_POINT('Ctrl Pts',(-63.6612325830983,-127.289830509258,
169.949972041807));
#36266=CARTESIAN_POINT('Ctrl Pts',(-63.6163270545268,-127.257558044475,
169.962964394853));
#36267=CARTESIAN_POINT('Ctrl Pts',(-63.5246367188867,-127.212730678233,
169.975573590834));
#36268=CARTESIAN_POINT('Ctrl Pts',(-63.4811600294583,-127.198151515523,
169.977054999153));
#36269=CARTESIAN_POINT('Ctrl Pts',(-63.4041176042462,-127.182655975731,
169.969255719861));
#36270=CARTESIAN_POINT('Ctrl Pts',(-63.3718396789871,-127.179146989545,
169.962964196295));
#36271=CARTESIAN_POINT('Ctrl Pts',(-63.3284860194241,-127.178331768181,
169.949812479676));
#36272=CARTESIAN_POINT('Ctrl Pts',(-63.3169239346392,-127.17850895578,169.945832840802));
#36273=CARTESIAN_POINT('Ctrl Pts',(-63.2982284678402,-127.179452576264,
169.938589776834));
#36274=CARTESIAN_POINT('Ctrl Pts',(-63.2910112559024,-127.179981522283,
169.935591329969));
#36275=CARTESIAN_POINT('Ctrl Pts',(-63.2772635681678,-127.181313627362,
169.929478524726));
#36276=CARTESIAN_POINT('Ctrl Pts',(-63.2707258659438,-127.182091973242,
169.926392506813));
#36277=CARTESIAN_POINT('Ctrl Pts',(-63.2558653474691,-127.184203875358,
169.918955092668));
#36278=CARTESIAN_POINT('Ctrl Pts',(-63.2476037863023,-127.185631266962,
169.914507717447));
#36279=CARTESIAN_POINT('Ctrl Pts',(-63.2227671202083,-127.190729473619,
169.900154667556));
#36280=CARTESIAN_POINT('Ctrl Pts',(-63.2067827832207,-127.195148255939,
169.889527570186));
#36281=CARTESIAN_POINT('Ctrl Pts',(-63.1581459365239,-127.212568894871,
169.852616862557));
#36282=CARTESIAN_POINT('Ctrl Pts',(-63.1296328608877,-127.229161218297,
169.823585338963));
#36283=CARTESIAN_POINT('Ctrl Pts',(-63.0829548063272,-127.271810144691,
169.761627322943));
#36284=CARTESIAN_POINT('Ctrl Pts',(-63.0655007825547,-127.297347280196,
169.729598715239));
#36285=CARTESIAN_POINT('Ctrl Pts',(-63.0370861717759,-127.364219960214,
169.658713788112));
#36286=CARTESIAN_POINT('Ctrl Pts',(-63.0294765287605,-127.4067884638,169.621582058969));
#36287=CARTESIAN_POINT('Ctrl Pts',(-63.0232099521103,-127.515463440772,
169.545440320815));
#36288=CARTESIAN_POINT('Ctrl Pts',(-63.0281254860832,-127.586356301289,
169.508300828821));
#36289=CARTESIAN_POINT('Ctrl Pts',(-63.0456343296776,-127.756830302552,
169.449761494122));
#36290=CARTESIAN_POINT('Ctrl Pts',(-63.0587645208149,-127.858733851834,
169.431247709482));
#36291=CARTESIAN_POINT('Ctrl Pts',(-63.0703759742411,-127.967652479905,
169.431247709482));
#36292=CARTESIAN_POINT('',(-64.5590459398891,-127.80895031592,170.209949994551));
#36293=CARTESIAN_POINT('Origin',(-60.6261834003547,-128.228219737673,175.985485069079));
#36294=CARTESIAN_POINT('',(-65.2955191767793,-127.730437348568,170.794192734786));
#36295=CARTESIAN_POINT('Ctrl Pts',(-65.2955191767793,-127.730437348568,
170.794192734786));
#36296=CARTESIAN_POINT('Ctrl Pts',(-65.2816442742383,-127.600286945004,
170.794192734786));
#36297=CARTESIAN_POINT('Ctrl Pts',(-65.2469267013282,-127.481589522909,
170.80946310351));
#36298=CARTESIAN_POINT('Ctrl Pts',(-65.1568593030527,-127.303848224493,
170.841475787782));
#36299=CARTESIAN_POINT('Ctrl Pts',(-65.1073342677368,-127.237746884734,
170.856782578368));
#36300=CARTESIAN_POINT('Ctrl Pts',(-65.0074107092975,-127.146318927332,
170.87140125162));
#36301=CARTESIAN_POINT('Ctrl Pts',(-64.9606047860984,-127.114249057312,
170.874148742754));
#36302=CARTESIAN_POINT('Ctrl Pts',(-64.8684109837781,-127.069475363982,
170.865709463374));
#36303=CARTESIAN_POINT('Ctrl Pts',(-64.8257862688682,-127.054805375097,
170.857171654254));
#36304=CARTESIAN_POINT('Ctrl Pts',(-64.7527659098192,-127.03888105618,170.831658539489));
#36305=CARTESIAN_POINT('Ctrl Pts',(-64.722901811052,-127.035114739964,170.817957766561));
#36306=CARTESIAN_POINT('Ctrl Pts',(-64.6839209542326,-127.033833348613,
170.794892145581));
#36307=CARTESIAN_POINT('Ctrl Pts',(-64.673638633589,-127.033874104805,170.788272255348));
#36308=CARTESIAN_POINT('Ctrl Pts',(-64.6572068205804,-127.034576404671,
170.776766814454));
#36309=CARTESIAN_POINT('Ctrl Pts',(-64.6509121233055,-127.035007004464,
170.772124618239));
#36310=CARTESIAN_POINT('Ctrl Pts',(-64.639018156889,-127.036141490465,170.762884146693));
#36311=CARTESIAN_POINT('Ctrl Pts',(-64.6334050488427,-127.03682126843,170.758312298135));
#36312=CARTESIAN_POINT('Ctrl Pts',(-64.620747827179,-127.038698284386,170.74750110857));
#36313=CARTESIAN_POINT('Ctrl Pts',(-64.6137863359549,-127.039987079847,
170.741180773749));
#36314=CARTESIAN_POINT('Ctrl Pts',(-64.5930944395732,-127.044643426362,
170.721205148696));
#36315=CARTESIAN_POINT('Ctrl Pts',(-64.5801117945996,-127.04874220826,170.706971007307));
#36316=CARTESIAN_POINT('Ctrl Pts',(-64.5417092629567,-127.065071800833,
170.659116939299));
#36317=CARTESIAN_POINT('Ctrl Pts',(-64.5209747884925,-127.080834873406,
170.623722912221));
#36318=CARTESIAN_POINT('Ctrl Pts',(-64.4905124823315,-127.121755092684,
170.5513754796));
#36319=CARTESIAN_POINT('Ctrl Pts',(-64.4812599206048,-127.146417897543,
170.515476230233));
#36320=CARTESIAN_POINT('Ctrl Pts',(-64.4707348287764,-127.211383435322,
170.438192857666));
#36321=CARTESIAN_POINT('Ctrl Pts',(-64.4723103450735,-127.25297273956,170.399249347361));
#36322=CARTESIAN_POINT('Ctrl Pts',(-64.48467592649,-127.359661404002,170.321071945463));
#36323=CARTESIAN_POINT('Ctrl Pts',(-64.4985053552031,-127.429603983786,
170.284382921946));
#36324=CARTESIAN_POINT('Ctrl Pts',(-64.5299637440578,-127.598590870331,
170.227386427625));
#36325=CARTESIAN_POINT('Ctrl Pts',(-64.5474344864629,-127.700031687849,
170.209949994551));
#36326=CARTESIAN_POINT('Ctrl Pts',(-64.5590459398891,-127.80895031592,170.209949994551));
#36327=CARTESIAN_POINT('',(-65.819152230113,-127.674614566746,171.324305384935));
#36328=CARTESIAN_POINT('Origin',(-60.6261834003547,-128.228219737673,175.985485069079));
#36329=CARTESIAN_POINT('',(-66.3951942621838,-127.613204637651,172.068819382192));
#36330=CARTESIAN_POINT('Ctrl Pts',(-66.3951942621838,-127.613204637651,
172.068819382192));
#36331=CARTESIAN_POINT('Ctrl Pts',(-66.3813193596428,-127.483054234087,
172.068819382192));
#36332=CARTESIAN_POINT('Ctrl Pts',(-66.3436018638514,-127.364676623814,
172.078395599549));
#36333=CARTESIAN_POINT('Ctrl Pts',(-66.2479598612561,-127.187529615458,
172.092554064181));
#36334=CARTESIAN_POINT('Ctrl Pts',(-66.1960127796873,-127.121686482012,
172.097307649504));
#36335=CARTESIAN_POINT('Ctrl Pts',(-66.095201381932,-127.030353174215,172.090042423964));
#36336=CARTESIAN_POINT('Ctrl Pts',(-66.0489882276089,-126.998220111072,
172.082385378989));
#36337=CARTESIAN_POINT('Ctrl Pts',(-65.9613144359736,-126.952964554406,
172.053388084489));
#36338=CARTESIAN_POINT('Ctrl Pts',(-65.9219011842493,-126.937952202089,
172.035327244364));
#36339=CARTESIAN_POINT('Ctrl Pts',(-65.8570013299288,-126.921162183116,
171.993583023619));
#36340=CARTESIAN_POINT('Ctrl Pts',(-65.8312440748459,-126.916958049926,
171.973269240452));
#36341=CARTESIAN_POINT('Ctrl Pts',(-65.7988681395039,-126.914972529819,
171.941630205162));
#36342=CARTESIAN_POINT('Ctrl Pts',(-65.7904566887047,-126.914813838786,
171.932754787527));
#36343=CARTESIAN_POINT('Ctrl Pts',(-65.7772370578837,-126.915173698571,
171.917655624111));
#36344=CARTESIAN_POINT('Ctrl Pts',(-65.7722292271653,-126.915467109792,
171.911639466116));
#36345=CARTESIAN_POINT('Ctrl Pts',(-65.7628793984067,-126.916330373721,
171.899808350887));
#36346=CARTESIAN_POINT('Ctrl Pts',(-65.7585175965269,-126.916876754089,
171.894016370906));
#36347=CARTESIAN_POINT('Ctrl Pts',(-65.748802495888,-126.918440120287,171.880459712958));
#36348=CARTESIAN_POINT('Ctrl Pts',(-65.7435489999587,-126.91954683204,171.872633733424));
#36349=CARTESIAN_POINT('Ctrl Pts',(-65.728219422495,-126.923631519533,171.848196443929));
#36350=CARTESIAN_POINT('Ctrl Pts',(-65.7190096041221,-126.927328092909,
171.83118249508));
#36351=CARTESIAN_POINT('Ctrl Pts',(-65.6931481581786,-126.942320721961,
171.775166171184));
#36352=CARTESIAN_POINT('Ctrl Pts',(-65.6814803202524,-126.957117230505,
171.735466612822));
#36353=CARTESIAN_POINT('Ctrl Pts',(-65.6692349030829,-126.996095407713,
171.656934333413));
#36354=CARTESIAN_POINT('Ctrl Pts',(-65.6688665697256,-127.019811094472,
171.619250776266));
#36355=CARTESIAN_POINT('Ctrl Pts',(-65.6772337803267,-127.082762586595,
171.54006038696));
#36356=CARTESIAN_POINT('Ctrl Pts',(-65.6881586964586,-127.123355182348,
171.501568350758));
#36357=CARTESIAN_POINT('Ctrl Pts',(-65.7190994405689,-127.228063610348,
171.425898671551));
#36358=CARTESIAN_POINT('Ctrl Pts',(-65.7414765457023,-127.297094950719,
171.391792349199));
#36359=CARTESIAN_POINT('Ctrl Pts',(-65.7861119859214,-127.464677075554,
171.339651124332));
#36360=CARTESIAN_POINT('Ctrl Pts',(-65.8075407766868,-127.565695938674,
171.324305384935));
#36361=CARTESIAN_POINT('Ctrl Pts',(-65.819152230113,-127.674614566746,171.324305384935));
#36362=CARTESIAN_POINT('',(-66.7774620476251,-127.572452337832,172.709551595863));
#36363=CARTESIAN_POINT('Origin',(-60.6261834003547,-128.228219737673,175.985485069079));
#36364=CARTESIAN_POINT('',(-67.1595954058001,-127.531714368858,173.57106840282));
#36365=CARTESIAN_POINT('Ctrl Pts',(-67.1595954058001,-127.531714368858,
173.57106840282));
#36366=CARTESIAN_POINT('Ctrl Pts',(-67.1457205032591,-127.401563965294,
173.57106840282));
#36367=CARTESIAN_POINT('Ctrl Pts',(-67.1064452783649,-127.28335241935,173.574393933864));
#36368=CARTESIAN_POINT('Ctrl Pts',(-67.0096393786517,-127.106329490205,
173.569875340355));
#36369=CARTESIAN_POINT('Ctrl Pts',(-66.9578519481981,-127.040469336883,
173.563799459316));
#36370=CARTESIAN_POINT('Ctrl Pts',(-66.8613861610659,-126.948672757959,
173.535072563485));
#36371=CARTESIAN_POINT('Ctrl Pts',(-66.8182244895502,-126.916214386363,
173.517455982022));
#36372=CARTESIAN_POINT('Ctrl Pts',(-66.7398314993754,-126.869969434257,
173.469585889759));
#36373=CARTESIAN_POINT('Ctrl Pts',(-66.705802560936,-126.854383078172,173.443051649007));
#36374=CARTESIAN_POINT('Ctrl Pts',(-66.652649715689,-126.836340749551,173.387502344657));
#36375=CARTESIAN_POINT('Ctrl Pts',(-66.6324536466569,-126.831543756775,
173.361756114491));
#36376=CARTESIAN_POINT('Ctrl Pts',(-66.6085308974996,-126.828657070545,
173.32338241062));
#36377=CARTESIAN_POINT('Ctrl Pts',(-66.6024726940923,-126.828247507619,
173.312767272596));
#36378=CARTESIAN_POINT('Ctrl Pts',(-66.5932270935042,-126.828183709231,
173.294951895151));
#36379=CARTESIAN_POINT('Ctrl Pts',(-66.5897956932282,-126.828309062434,
173.287911412611));
#36380=CARTESIAN_POINT('Ctrl Pts',(-66.5835325624315,-126.828843263739,
173.274177235112));
#36381=CARTESIAN_POINT('Ctrl Pts',(-66.5806760573395,-126.829229169412,
173.26750173253));
#36382=CARTESIAN_POINT('Ctrl Pts',(-66.5744709165635,-126.83041835044,173.251987469885));
#36383=CARTESIAN_POINT('Ctrl Pts',(-66.5712340788036,-126.831310072958,
173.243110663121));
#36384=CARTESIAN_POINT('Ctrl Pts',(-66.5621727309781,-126.834726525295,
173.215631915624));
#36385=CARTESIAN_POINT('Ctrl Pts',(-66.5572876108246,-126.837962056948,
173.196826948178));
#36386=CARTESIAN_POINT('Ctrl Pts',(-66.5455451789095,-126.851449504777,
173.135903833527));
#36387=CARTESIAN_POINT('Ctrl Pts',(-66.5437050929278,-126.865198309306,
173.094205937912));
#36388=CARTESIAN_POINT('Ctrl Pts',(-66.5506190059696,-126.902133973911,
173.01405282234));
#36389=CARTESIAN_POINT('Ctrl Pts',(-66.559301348245,-126.924884798181,172.976774988782));
#36390=CARTESIAN_POINT('Ctrl Pts',(-66.5864656928081,-126.985832390242,
172.900279840317));
#36391=CARTESIAN_POINT('Ctrl Pts',(-66.6063608961624,-127.025468693448,
172.864476295449));
#36392=CARTESIAN_POINT('Ctrl Pts',(-66.6547402866562,-127.128318045238,
172.79571198564));
#36393=CARTESIAN_POINT('Ctrl Pts',(-66.6848020900059,-127.196530145439,
172.766170499937));
#36394=CARTESIAN_POINT('Ctrl Pts',(-66.741076285365,-127.36287150122,172.721914802988));
#36395=CARTESIAN_POINT('Ctrl Pts',(-66.7658505941991,-127.463533709763,
172.709551595863));
#36396=CARTESIAN_POINT('Ctrl Pts',(-66.7774620476251,-127.572452337832,
172.709551595863));
#36397=CARTESIAN_POINT('Origin',(-60.6261834003547,-128.228219737673,175.985485069079));
#36398=CARTESIAN_POINT('Origin',(-60.6261834003547,-128.228219737673,175.985485069079));
#36399=CARTESIAN_POINT('Origin',(-60.6261834003547,-128.228219737673,175.985485069079));
#36400=CARTESIAN_POINT('Origin',(-60.6261834003547,-128.228219737673,175.985485069079));
#36401=CARTESIAN_POINT('Origin',(-60.6261834003547,-128.228219737673,175.985485069079));
#36402=CARTESIAN_POINT('Origin',(-60.6261834003547,-128.228219737673,175.985485069079));
#36403=CARTESIAN_POINT('Origin',(-60.6261834003547,-128.228219737673,175.985485069079));
#36404=CARTESIAN_POINT('Origin',(-60.6261834003547,-128.228219737673,175.985485069079));
#36405=CARTESIAN_POINT('Origin',(-60.6261834003547,-128.228219737673,175.985485069079));
#36406=CARTESIAN_POINT('Origin',(-60.6261834003547,-128.228219737673,175.985485069079));
#36407=CARTESIAN_POINT('',(-56.6933208608202,-128.647489159427,181.761020143608));
#36408=CARTESIAN_POINT('Origin',(-60.6261834003547,-128.228219737673,175.985485069079));
#36409=CARTESIAN_POINT('',(-55.9568476239301,-128.726002126779,181.176777403373));
#36410=CARTESIAN_POINT('Ctrl Pts',(-55.9568476239301,-128.726002126779,
181.176777403373));
#36411=CARTESIAN_POINT('Ctrl Pts',(-55.9429727213892,-128.595851723216,
181.176777403373));
#36412=CARTESIAN_POINT('Ctrl Pts',(-55.9518865477261,-128.472502902465,
181.161507034649));
#36413=CARTESIAN_POINT('Ctrl Pts',(-56.0024587592649,-128.279768482043,
181.129494350376));
#36414=CARTESIAN_POINT('Ctrl Pts',(-56.0369354276589,-128.204711999462,
181.11418755979));
#36415=CARTESIAN_POINT('Ctrl Pts',(-56.1153386429352,-128.094273216599,
181.099568886539));
#36416=CARTESIAN_POINT('Ctrl Pts',(-56.1543317368433,-128.053056598142,
181.096821395405));
#36417=CARTESIAN_POINT('Ctrl Pts',(-56.2350144505794,-127.989853113231,
181.105260674785));
#36418=CARTESIAN_POINT('Ctrl Pts',(-56.2735885050927,-127.966526793044,
181.113798483904));
#36419=CARTESIAN_POINT('Ctrl Pts',(-56.3416106408167,-127.935566401895,
181.13931159867));
#36420=CARTESIAN_POINT('Ctrl Pts',(-56.3700095524372,-127.925588859522,
181.153012371598));
#36421=CARTESIAN_POINT('Ctrl Pts',(-56.4078441925729,-127.916118423,181.176077992577));
#36422=CARTESIAN_POINT('Ctrl Pts',(-56.4179040148444,-127.913990570853,
181.182697882811));
#36423=CARTESIAN_POINT('Ctrl Pts',(-56.4341145873676,-127.911212974341,
181.194203323706));
#36424=CARTESIAN_POINT('Ctrl Pts',(-56.4403585921181,-127.910306864729,
181.198845519921));
#36425=CARTESIAN_POINT('Ctrl Pts',(-56.4522244164565,-127.908908398299,
181.208085991466));
#36426=CARTESIAN_POINT('Ctrl Pts',(-56.4578546814881,-127.908389557577,
181.212657840024));
#36427=CARTESIAN_POINT('Ctrl Pts',(-56.4706231455126,-127.907556025573,
181.223469029589));
#36428=CARTESIAN_POINT('Ctrl Pts',(-56.4776998809229,-127.907348252287,
181.22978936441));
#36429=CARTESIAN_POINT('Ctrl Pts',(-56.4989083753106,-127.907537737214,
181.249764989463));
#36430=CARTESIAN_POINT('Ctrl Pts',(-56.5124633358786,-127.908807433066,
181.263999130852));
#36431=CARTESIAN_POINT('Ctrl Pts',(-56.5534453507174,-127.916674102625,
181.31185319886));
#36432=CARTESIAN_POINT('Ctrl Pts',(-56.5770369576528,-127.927711718782,
181.347247225938));
#36433=CARTESIAN_POINT('Ctrl Pts',(-56.6154413325744,-127.961290289766,
181.419594658559));
#36434=CARTESIAN_POINT('Ctrl Pts',(-56.6296852961918,-127.983448208045,
181.455493907926));
#36435=CARTESIAN_POINT('Ctrl Pts',(-56.6536697087511,-128.044734802102,
181.532777280493));
#36436=CARTESIAN_POINT('Ctrl Pts',(-56.6608973514961,-128.0857215519,181.571720790798));
#36437=CARTESIAN_POINT('Ctrl Pts',(-56.671301510426,-128.192619317084,181.649898192696));
#36438=CARTESIAN_POINT('Ctrl Pts',(-56.6725280064147,-128.263905453695,
181.686587216213));
#36439=CARTESIAN_POINT('Ctrl Pts',(-56.6774020108528,-128.435726413225,
181.743583710534));
#36440=CARTESIAN_POINT('Ctrl Pts',(-56.681709407394,-128.538570531355,181.761020143608));
#36441=CARTESIAN_POINT('Ctrl Pts',(-56.6933208608202,-128.647489159427,
181.761020143608));
#36442=CARTESIAN_POINT('',(-55.4332145705962,-128.781824908601,180.646664753224));
#36443=CARTESIAN_POINT('Origin',(-60.6261834003547,-128.228219737673,175.985485069079));
#36444=CARTESIAN_POINT('',(-54.8571725385255,-128.843234837696,179.902150755967));
#36445=CARTESIAN_POINT('Ctrl Pts',(-54.8571725385255,-128.843234837696,
179.902150755967));
#36446=CARTESIAN_POINT('Ctrl Pts',(-54.8432976359846,-128.713084434133,
179.902150755967));
#36447=CARTESIAN_POINT('Ctrl Pts',(-54.8552113852029,-128.58941580156,179.89257453861));
#36448=CARTESIAN_POINT('Ctrl Pts',(-54.9113582010602,-128.396087091074,
179.878416073978));
#36449=CARTESIAN_POINT('Ctrl Pts',(-54.9482569157069,-128.320772402181,
179.873662488655));
#36450=CARTESIAN_POINT('Ctrl Pts',(-55.0275479703008,-128.210238969717,
179.880927714194));
#36451=CARTESIAN_POINT('Ctrl Pts',(-55.0659482953328,-128.169085544381,
179.88858475917));
#36452=CARTESIAN_POINT('Ctrl Pts',(-55.1421109983837,-128.106363922807,
179.917582053669));
#36453=CARTESIAN_POINT('Ctrl Pts',(-55.1774735897115,-128.083379966052,
179.935642893795));
#36454=CARTESIAN_POINT('Ctrl Pts',(-55.2373752207072,-128.053285274958,
179.97738711454));
#36455=CARTESIAN_POINT('Ctrl Pts',(-55.2616672886433,-128.04374554956,179.997700897707));
#36456=CARTESIAN_POINT('Ctrl Pts',(-55.292897007302,-128.034979241794,180.029339932996));
#36457=CARTESIAN_POINT('Ctrl Pts',(-55.3010859597289,-128.033050836872,
180.038215350631));
#36458=CARTESIAN_POINT('Ctrl Pts',(-55.3140843500635,-128.030615680441,
180.053314514049));
#36459=CARTESIAN_POINT('Ctrl Pts',(-55.3190414882579,-128.029846759401,
180.059330672043));
#36460=CARTESIAN_POINT('Ctrl Pts',(-55.3283631749389,-128.028719515043,
180.071161787272));
#36461=CARTESIAN_POINT('Ctrl Pts',(-55.332742133804,-128.028334071918,180.076953767253));
#36462=CARTESIAN_POINT('Ctrl Pts',(-55.3425684768033,-128.027814189671,
180.0905104252));
#36463=CARTESIAN_POINT('Ctrl Pts',(-55.3479372169186,-128.027788500095,
180.098336404735));
#36464=CARTESIAN_POINT('Ctrl Pts',(-55.3637833923889,-128.028549644043,
180.12277369423));
#36465=CARTESIAN_POINT('Ctrl Pts',(-55.3735655263562,-128.030221548417,
180.139787643079));
#36466=CARTESIAN_POINT('Ctrl Pts',(-55.4020064554956,-128.039425181497,
180.195803966976));
#36467=CARTESIAN_POINT('Ctrl Pts',(-55.416531425893,-128.051429361683,180.235503525337));
#36468=CARTESIAN_POINT('Ctrl Pts',(-55.4367189118229,-128.086949974739,
180.314035804746));
#36469=CARTESIAN_POINT('Ctrl Pts',(-55.4420786470709,-128.110055011116,
180.351719361893));
#36470=CARTESIAN_POINT('Ctrl Pts',(-55.4471707572007,-128.17335565083,180.430909751199));
#36471=CARTESIAN_POINT('Ctrl Pts',(-55.4450490001109,-128.215339109112,
180.469401787402));
#36472=CARTESIAN_POINT('Ctrl Pts',(-55.4368779963468,-128.324217110737,
180.545071466608));
#36473=CARTESIAN_POINT('Ctrl Pts',(-55.4295568159153,-128.396414486761,
180.57917778896));
#36474=CARTESIAN_POINT('Ctrl Pts',(-55.4212537689891,-128.569640208002,
180.631319013827));
#36475=CARTESIAN_POINT('Ctrl Pts',(-55.4216031171701,-128.672906280531,
180.646664753224));
#36476=CARTESIAN_POINT('Ctrl Pts',(-55.4332145705962,-128.781824908601,
180.646664753224));
#36477=CARTESIAN_POINT('',(-54.4749047530841,-128.883987137515,179.261418542296));
#36478=CARTESIAN_POINT('Origin',(-60.6261834003547,-128.228219737673,175.985485069079));
#36479=CARTESIAN_POINT('',(-54.0927713949092,-128.924725106489,178.399901735339));
#36480=CARTESIAN_POINT('Ctrl Pts',(-54.0927713949092,-128.924725106489,
178.399901735339));
#36481=CARTESIAN_POINT('Ctrl Pts',(-54.0788964923682,-128.794574702925,
178.399901735339));
#36482=CARTESIAN_POINT('Ctrl Pts',(-54.0923679706893,-128.670740006023,
178.396576204295));
#36483=CARTESIAN_POINT('Ctrl Pts',(-54.1496786836653,-128.477287216329,
178.401094797804));
#36484=CARTESIAN_POINT('Ctrl Pts',(-54.1864177471969,-128.401989547312,
178.407170678843));
#36485=CARTESIAN_POINT('Ctrl Pts',(-54.2613631911669,-128.291919385972,
178.435897574673));
#36486=CARTESIAN_POINT('Ctrl Pts',(-54.2967120333915,-128.251091269091,
178.453514156137));
#36487=CARTESIAN_POINT('Ctrl Pts',(-54.3635939349819,-128.189359042956,
178.5013842484));
#36488=CARTESIAN_POINT('Ctrl Pts',(-54.3935722130247,-128.166949089969,
178.527918489152));
#36489=CARTESIAN_POINT('Ctrl Pts',(-54.4417268349467,-128.138106708523,
178.583467793501));
#36490=CARTESIAN_POINT('Ctrl Pts',(-54.4604577168323,-128.129159842712,
178.609214023668));
#36491=CARTESIAN_POINT('Ctrl Pts',(-54.4832342493068,-128.121294701068,
178.647587727539));
#36492=CARTESIAN_POINT('Ctrl Pts',(-54.4890699543414,-128.119617168039,
178.658202865563));
#36493=CARTESIAN_POINT('Ctrl Pts',(-54.4980943144427,-128.117605669782,
178.676018243009));
#36494=CARTESIAN_POINT('Ctrl Pts',(-54.5014750221949,-128.117004806759,
178.683058725548));
#36495=CARTESIAN_POINT('Ctrl Pts',(-54.5077100109139,-128.116206625025,
178.696792903046));
#36496=CARTESIAN_POINT('Ctrl Pts',(-54.5105836729911,-128.115981656595,
178.703468405629));
#36497=CARTESIAN_POINT('Ctrl Pts',(-54.5169000561279,-128.115835959519,
178.718982668274));
#36498=CARTESIAN_POINT('Ctrl Pts',(-54.520252138074,-128.116025259176,178.727859475038));
#36499=CARTESIAN_POINT('Ctrl Pts',(-54.5298300839057,-128.117454638282,
178.755338222534));
#36500=CARTESIAN_POINT('Ctrl Pts',(-54.5352875196535,-128.119587584378,
178.77414318998));
#36501=CARTESIAN_POINT('Ctrl Pts',(-54.5496094347646,-128.130296398681,
178.835066304632));
#36502=CARTESIAN_POINT('Ctrl Pts',(-54.5543066532175,-128.143348282882,
178.876764200246));
#36503=CARTESIAN_POINT('Ctrl Pts',(-54.5553348089362,-128.18091140854,178.956917315818));
#36504=CARTESIAN_POINT('Ctrl Pts',(-54.5516438685516,-128.204981307407,
178.994195149376));
#36505=CARTESIAN_POINT('Ctrl Pts',(-54.5379388447194,-128.270285847182,
179.070690297841));
#36506=CARTESIAN_POINT('Ctrl Pts',(-54.5268468004073,-128.313225598012,
179.10649384271));
#36507=CARTESIAN_POINT('Ctrl Pts',(-54.5012371502593,-128.423962675849,
179.17525815252));
#36508=CARTESIAN_POINT('Ctrl Pts',(-54.4862312716116,-128.496979292044,
179.204799638222));
#36509=CARTESIAN_POINT('Ctrl Pts',(-54.4662894695462,-128.671445782337,
179.249055335171));
#36510=CARTESIAN_POINT('Ctrl Pts',(-54.4632932996579,-128.775068509443,
179.261418542296));
#36511=CARTESIAN_POINT('Ctrl Pts',(-54.4749047530841,-128.883987137515,
179.261418542296));
#36512=CARTESIAN_POINT('',(-53.8740848915632,-128.948038548767,177.685786985438));
#36513=CARTESIAN_POINT('Origin',(-60.6261834003547,-128.228219737673,175.985485069079));
#36514=CARTESIAN_POINT('',(-53.708068409063,-128.96573701494,176.757335594116));
#36515=CARTESIAN_POINT('Ctrl Pts',(-53.708068409063,-128.96573701494,176.757335594116));
#36516=CARTESIAN_POINT('Ctrl Pts',(-53.694193506522,-128.835586611376,176.757335594116));
#36517=CARTESIAN_POINT('Ctrl Pts',(-53.7076899906135,-128.711749248692,
176.760454017161));
#36518=CARTESIAN_POINT('Ctrl Pts',(-53.7616862520391,-128.518649801677,
176.783387064581));
#36519=CARTESIAN_POINT('Ctrl Pts',(-53.7956932454308,-128.443643389589,
176.799939303861));
#36520=CARTESIAN_POINT('Ctrl Pts',(-53.8613121799281,-128.334567496468,
176.848458367214));
#36521=CARTESIAN_POINT('Ctrl Pts',(-53.891328166503,-128.294307897628,176.875010673484));
#36522=CARTESIAN_POINT('Ctrl Pts',(-53.9447078423048,-128.234015098969,
176.93897152775));
#36523=CARTESIAN_POINT('Ctrl Pts',(-53.9674418736801,-128.212377431075,
176.972437095504));
#36524=CARTESIAN_POINT('Ctrl Pts',(-54.0009056756515,-128.185101189184,
177.038563159802));
#36525=CARTESIAN_POINT('Ctrl Pts',(-54.0129442250395,-128.176867770727,
177.068245559654));
#36526=CARTESIAN_POINT('Ctrl Pts',(-54.0259105750774,-128.170048460072,
177.111123791921));
#36527=CARTESIAN_POINT('Ctrl Pts',(-54.0290474173572,-128.168658643843,
177.122861737096));
#36528=CARTESIAN_POINT('Ctrl Pts',(-54.0335668553725,-128.167127400378,
177.14235796359));
#36529=CARTESIAN_POINT('Ctrl Pts',(-54.0351731852033,-128.166715697895,
177.15001360342));
#36530=CARTESIAN_POINT('Ctrl Pts',(-54.0379583033214,-128.166285295416,
177.164852662714));
#36531=CARTESIAN_POINT('Ctrl Pts',(-54.039160160367,-128.166238552571,177.17202373195));
#36532=CARTESIAN_POINT('Ctrl Pts',(-54.0416027309134,-128.166505829798,
177.188593966742));
#36533=CARTESIAN_POINT('Ctrl Pts',(-54.0427466926584,-128.166930529821,
177.198005712992));
#36534=CARTESIAN_POINT('Ctrl Pts',(-54.0455147848535,-128.16908588482,177.226928953567));
#36535=CARTESIAN_POINT('Ctrl Pts',(-54.0463469865043,-128.171711911772,
177.246432063255));
#36536=CARTESIAN_POINT('Ctrl Pts',(-54.0457925050324,-128.184006649338,
177.308721338684));
#36537=CARTESIAN_POINT('Ctrl Pts',(-54.040472009355,-128.198126488793,177.349994241424));
#36538=CARTESIAN_POINT('Ctrl Pts',(-54.0225118642734,-128.237713894175,
177.427109985427));
#36539=CARTESIAN_POINT('Ctrl Pts',(-54.0101297933627,-128.26271032562,177.461815643209));
#36540=CARTESIAN_POINT('Ctrl Pts',(-53.9788152251371,-128.329892160475,
177.531169930852));
#36541=CARTESIAN_POINT('Ctrl Pts',(-53.9596533267027,-128.373692211668,
177.5622042125));
#36542=CARTESIAN_POINT('Ctrl Pts',(-53.9187550172226,-128.486059162732,
177.620066821173));
#36543=CARTESIAN_POINT('Ctrl Pts',(-53.8973740252904,-128.559755408594,
177.643326626457));
#36544=CARTESIAN_POINT('Ctrl Pts',(-53.8680081664537,-128.7352265663,177.677124815244));
#36545=CARTESIAN_POINT('Ctrl Pts',(-53.8624734381369,-128.839119920695,
177.685786985438));
#36546=CARTESIAN_POINT('Ctrl Pts',(-53.8740848915633,-128.948038548767,
177.685786985438));
#36547=CARTESIAN_POINT('',(-53.6656724524939,-128.970256707153,176.011340061548));
#36548=CARTESIAN_POINT('Origin',(-60.6261834003547,-128.228219737673,175.985485069079));
#36549=CARTESIAN_POINT('',(-53.7254211201858,-128.963887100003,175.06991230594));
#36550=CARTESIAN_POINT('Ctrl Pts',(-53.7254211201858,-128.963887100003,
175.06991230594));
#36551=CARTESIAN_POINT('Ctrl Pts',(-53.7115462176449,-128.833736696439,
175.06991230594));
#36552=CARTESIAN_POINT('Ctrl Pts',(-53.72353353093,-128.710060221445,175.079293451662));
#36553=CARTESIAN_POINT('Ctrl Pts',(-53.7699296160128,-128.517771004004,
175.119308167634));
#36554=CARTESIAN_POINT('Ctrl Pts',(-53.7987908982256,-128.443313159106,
175.145374809174));
#36555=CARTESIAN_POINT('Ctrl Pts',(-53.8506444472315,-128.335704748044,
175.210866288448));
#36556=CARTESIAN_POINT('Ctrl Pts',(-53.8733561315008,-128.296223836628,
175.244811195998));
#36557=CARTESIAN_POINT('Ctrl Pts',(-53.9097968574698,-128.237736843189,
175.321145639904));
#36558=CARTESIAN_POINT('Ctrl Pts',(-53.9238477180795,-128.21702485931,175.359597637505));
#36559=CARTESIAN_POINT('Ctrl Pts',(-53.9405306662796,-128.191537568542,
175.432457455253));
#36560=CARTESIAN_POINT('Ctrl Pts',(-53.9451346707625,-128.184096722242,
175.464350991603));
#36561=CARTESIAN_POINT('Ctrl Pts',(-53.9475039742569,-128.178407127546,
175.509241825261));
#36562=CARTESIAN_POINT('Ctrl Pts',(-53.9477531865121,-128.17732515197,175.521420410881));
#36563=CARTESIAN_POINT('Ctrl Pts',(-53.947498620285,-128.176302849251,175.541464436604));
#36564=CARTESIAN_POINT('Ctrl Pts',(-53.9472357451108,-128.17609041651,175.549290315765));
#36565=CARTESIAN_POINT('Ctrl Pts',(-53.9464083139291,-128.176045135921,
175.564371864667));
#36566=CARTESIAN_POINT('Ctrl Pts',(-53.9458690169309,-128.17618401173,175.57162174408));
#36567=CARTESIAN_POINT('Ctrl Pts',(-53.9442990540655,-128.176879051825,
175.5882849492));
#36568=CARTESIAN_POINT('Ctrl Pts',(-53.9431717614975,-128.177545882733,
175.597684658454));
#36569=CARTESIAN_POINT('Ctrl Pts',(-53.9389841399988,-128.180442763281,
175.626371478498));
#36570=CARTESIAN_POINT('Ctrl Pts',(-53.9351593734685,-128.183565254154,
175.645439280584));
#36571=CARTESIAN_POINT('Ctrl Pts',(-53.9198356749549,-128.197434488929,
175.705474690515));
#36572=CARTESIAN_POINT('Ctrl Pts',(-53.9048896960938,-128.212580469198,
175.743923969295));
#36573=CARTESIAN_POINT('Ctrl Pts',(-53.8692158106455,-128.254056277646,
175.81352065499));
#36574=CARTESIAN_POINT('Ctrl Pts',(-53.8490072512308,-128.279887065054,
175.843637170317));
#36575=CARTESIAN_POINT('Ctrl Pts',(-53.802294130892,-128.348710488441,175.901819978033));
#36576=CARTESIAN_POINT('Ctrl Pts',(-53.7764318020244,-128.393224850283,
175.926281396815));
#36577=CARTESIAN_POINT('Ctrl Pts',(-53.7232833415724,-128.50689774928,175.969879539858));
#36578=CARTESIAN_POINT('Ctrl Pts',(-53.6972073196987,-128.581094516701,
175.985505889386));
#36579=CARTESIAN_POINT('Ctrl Pts',(-53.6611797943829,-128.757275852562,
176.006882342131));
#36580=CARTESIAN_POINT('Ctrl Pts',(-53.6540609990676,-128.861338079082,
176.011340061548));
#36581=CARTESIAN_POINT('Ctrl Pts',(-53.6656724524939,-128.970256707153,
176.011340061548));
#36582=CARTESIAN_POINT('',(-53.8617796092863,-128.949350374068,174.335390539474));
#36583=CARTESIAN_POINT('Origin',(-60.6261834003547,-128.228219737673,175.985485069079));
#36584=CARTESIAN_POINT('',(-54.1438210517818,-128.919282872009,173.435698778786));
#36585=CARTESIAN_POINT('Ctrl Pts',(-54.1438210517818,-128.919282872009,
173.435698778786));
#36586=CARTESIAN_POINT('Ctrl Pts',(-54.1299461492408,-128.789132468445,
173.435698778786));
#36587=CARTESIAN_POINT('Ctrl Pts',(-54.1389778226646,-128.665771084407,
173.450797449094));
#36588=CARTESIAN_POINT('Ctrl Pts',(-54.1739297012356,-128.474701895836,
173.505568323775));
#36589=CARTESIAN_POINT('Ctrl Pts',(-54.1955306812605,-128.401018047657,
173.539634469117));
#36590=CARTESIAN_POINT('Ctrl Pts',(-54.2299799629259,-128.29526504777,173.618292237587));
#36591=CARTESIAN_POINT('Ctrl Pts',(-54.2438403977334,-128.256727738681,
173.657656991775));
#36592=CARTESIAN_POINT('Ctrl Pts',(-54.2608898800193,-128.20030798137,173.741928744907));
#36593=CARTESIAN_POINT('Ctrl Pts',(-54.2653232800882,-128.180621283037,
173.783132482021));
#36594=CARTESIAN_POINT('Ctrl Pts',(-54.2641105829218,-128.157041787624,
173.858491705446));
#36595=CARTESIAN_POINT('Ctrl Pts',(-54.2609698988183,-128.150426576869,
173.890742841889));
#36596=CARTESIAN_POINT('Ctrl Pts',(-54.2525711534886,-128.145884928118,
173.935037384859));
#36597=CARTESIAN_POINT('Ctrl Pts',(-54.2499117870103,-128.145113026467,
173.946948835794));
#36598=CARTESIAN_POINT('Ctrl Pts',(-54.244891582158,-128.144598772664,173.966375774829));
#36599=CARTESIAN_POINT('Ctrl Pts',(-54.242773306296,-128.144584138032,173.973917081669));
#36600=CARTESIAN_POINT('Ctrl Pts',(-54.2383805953492,-128.144918940085,
173.988364635376));
#36601=CARTESIAN_POINT('Ctrl Pts',(-54.2361319848394,-128.145240040135,
173.995271988326));
#36602=CARTESIAN_POINT('Ctrl Pts',(-54.2306439615985,-128.146352771642,
174.011059758862));
#36603=CARTESIAN_POINT('Ctrl Pts',(-54.2273142776506,-128.147254392184,
174.019901154185));
#36604=CARTESIAN_POINT('Ctrl Pts',(-54.2164293231972,-128.150865253171,
174.046684379989));
#36605=CARTESIAN_POINT('Ctrl Pts',(-54.2081865004653,-128.154458738351,
174.064208723124));
#36606=CARTESIAN_POINT('Ctrl Pts',(-54.1790590976617,-128.169799540224,
174.118501227753));
#36607=CARTESIAN_POINT('Ctrl Pts',(-54.1554392646589,-128.185870211294,
174.151892350246));
#36608=CARTESIAN_POINT('Ctrl Pts',(-54.1043556574809,-128.228988799029,
174.209925271236));
#36609=CARTESIAN_POINT('Ctrl Pts',(-54.0776400986473,-128.255513276048,
174.233702381705));
#36610=CARTESIAN_POINT('Ctrl Pts',(-54.0186343263536,-128.325647178259,
174.277332336196));
#36611=CARTESIAN_POINT('Ctrl Pts',(-53.9878303954035,-128.370688347897,
174.293799283367));
#36612=CARTESIAN_POINT('Ctrl Pts',(-53.926182226586,-128.485267372592,174.320599195178));
#36613=CARTESIAN_POINT('Ctrl Pts',(-53.8973641161886,-128.559756464969,
174.327683942315));
#36614=CARTESIAN_POINT('Ctrl Pts',(-53.8578244665285,-128.73631221675,174.335396337284));
#36615=CARTESIAN_POINT('Ctrl Pts',(-53.8501681558601,-128.840431745997,
174.335390539474));
#36616=CARTESIAN_POINT('Ctrl Pts',(-53.8617796092863,-128.949350374068,
174.335390539474));
#36617=CARTESIAN_POINT('',(-54.4510093268082,-128.886534549599,172.755338513612));
#36618=CARTESIAN_POINT('Origin',(-60.6261834003547,-128.228219737673,175.985485069079));
#36619=CARTESIAN_POINT('',(-54.9389523206484,-128.83451656656,171.949669562728));
#36620=CARTESIAN_POINT('Ctrl Pts',(-54.9389523206484,-128.83451656656,171.949669562728));
#36621=CARTESIAN_POINT('Ctrl Pts',(-54.9250774181075,-128.704366162997,
171.949669562728));
#36622=CARTESIAN_POINT('Ctrl Pts',(-54.9298787536602,-128.581455761238,
171.969608277785));
#36623=CARTESIAN_POINT('Ctrl Pts',(-54.9502074912346,-128.391945497192,
172.035952227023));
#36624=CARTESIAN_POINT('Ctrl Pts',(-54.9628555204352,-128.319216093385,
172.076038075624));
#36625=CARTESIAN_POINT('Ctrl Pts',(-54.9772731256675,-128.215598604036,
172.163290829697));
#36626=CARTESIAN_POINT('Ctrl Pts',(-54.9812497663029,-128.178114973438,
172.205787694094));
#36627=CARTESIAN_POINT('Ctrl Pts',(-54.9775826596539,-128.123903742912,
172.293099188475));
#36628=CARTESIAN_POINT('Ctrl Pts',(-54.9720232412554,-128.105282345789,
172.334660053671));
#36629=CARTESIAN_POINT('Ctrl Pts',(-54.9528401369879,-128.083618615832,
172.408139078627));
#36630=CARTESIAN_POINT('Ctrl Pts',(-54.9420947137666,-128.077814121073,
172.438873496341));
#36631=CARTESIAN_POINT('Ctrl Pts',(-54.9233827171895,-128.074371933806,
172.479997510789));
#36632=CARTESIAN_POINT('Ctrl Pts',(-54.9179628592929,-128.073894318983,
172.490949576807));
#36633=CARTESIAN_POINT('Ctrl Pts',(-54.9084623430268,-128.073857696309,
172.508630406072));
#36634=CARTESIAN_POINT('Ctrl Pts',(-54.9046102999379,-128.074027892847,
172.51544886725));
#36635=CARTESIAN_POINT('Ctrl Pts',(-54.8969067798621,-128.074715649273,
172.528422786454));
#36636=CARTESIAN_POINT('Ctrl Pts',(-54.8930800354609,-128.075204988938,
172.534586182696));
#36637=CARTESIAN_POINT('Ctrl Pts',(-54.8839961283079,-128.076701065694,
172.54858099081));
#36638=CARTESIAN_POINT('Ctrl Pts',(-54.8786609108948,-128.077816489503,
172.556350242443));
#36639=CARTESIAN_POINT('Ctrl Pts',(-54.8617262288735,-128.082072291865,
172.579673330276));
#36640=CARTESIAN_POINT('Ctrl Pts',(-54.8495610232867,-128.086083929263,
172.594635763336));
#36641=CARTESIAN_POINT('Ctrl Pts',(-54.808397650064,-128.102707845994,172.640030079638));
#36642=CARTESIAN_POINT('Ctrl Pts',(-54.7775596848358,-128.119548018182,
172.666422475177));
#36643=CARTESIAN_POINT('Ctrl Pts',(-54.7142659315802,-128.163968289064,
172.709518969035));
#36644=CARTESIAN_POINT('Ctrl Pts',(-54.6827410255676,-128.191005474623,
172.725574835412));
#36645=CARTESIAN_POINT('Ctrl Pts',(-54.6152629057264,-128.262042585685,
172.752116322311));
#36646=CARTESIAN_POINT('Ctrl Pts',(-54.5815633889956,-128.307392444113,
172.759631798755));
#36647=CARTESIAN_POINT('Ctrl Pts',(-54.5156599265751,-128.422425111535,
172.768075965875));
#36648=CARTESIAN_POINT('Ctrl Pts',(-54.4862120292892,-128.496981343401,
172.76620737087));
#36649=CARTESIAN_POINT('Ctrl Pts',(-54.4465139093197,-128.673553989176,
172.759807491701));
#36650=CARTESIAN_POINT('Ctrl Pts',(-54.439397873382,-128.777615921527,172.755338513612));
#36651=CARTESIAN_POINT('Ctrl Pts',(-54.4510093268082,-128.886534549599,
172.755338513612));
#36652=CARTESIAN_POINT('',(-55.3991177156403,-128.785459861137,171.363010864448));
#36653=CARTESIAN_POINT('Origin',(-60.6261834003547,-128.228219737673,175.985485069079));
#36654=CARTESIAN_POINT('',(-56.0646047876237,-128.714514493215,170.698187274307));
#36655=CARTESIAN_POINT('Ctrl Pts',(-56.0646047876237,-128.714514493215,
170.698187274307));
#36656=CARTESIAN_POINT('Ctrl Pts',(-56.0507298850827,-128.584364089651,
170.698187274307));
#36657=CARTESIAN_POINT('Ctrl Pts',(-56.0502720366154,-128.462014352045,
170.721807268469));
#36658=CARTESIAN_POINT('Ctrl Pts',(-56.05364854251,-128.274311309154,170.795868623082));
#36659=CARTESIAN_POINT('Ctrl Pts',(-56.0561712852096,-128.202661328533,
170.839644531129));
#36660=CARTESIAN_POINT('Ctrl Pts',(-56.049093973138,-128.101335340974,170.930421457889));
#36661=CARTESIAN_POINT('Ctrl Pts',(-56.042728685082,-128.064954229068,170.973580669207));
#36662=CARTESIAN_POINT('Ctrl Pts',(-56.0182236170934,-128.012964464437,
171.058857678147));
#36663=CARTESIAN_POINT('Ctrl Pts',(-56.0028767685879,-127.995386472752,
171.098360305007));
#36664=CARTESIAN_POINT('Ctrl Pts',(-55.9666928702255,-127.975535141026,
171.16568879765));
#36665=CARTESIAN_POINT('Ctrl Pts',(-55.9489246171503,-127.970479326848,
171.193120323993));
#36666=CARTESIAN_POINT('Ctrl Pts',(-55.9209535355779,-127.968024219901,
171.228683831679));
#36667=CARTESIAN_POINT('Ctrl Pts',(-55.9130817033051,-127.967808001928,
171.238040018512));
#36668=CARTESIAN_POINT('Ctrl Pts',(-55.8996465822519,-127.968190834411,
171.252947192476));
#36669=CARTESIAN_POINT('Ctrl Pts',(-55.894283165646,-127.968522153463,171.258646543812));
#36670=CARTESIAN_POINT('Ctrl Pts',(-55.8837157192689,-127.969515223566,
171.269392831488));
#36671=CARTESIAN_POINT('Ctrl Pts',(-55.878533736002,-127.970149040748,171.274454076834));
#36672=CARTESIAN_POINT('Ctrl Pts',(-55.8663851011032,-127.971971837957,
171.285842595149));
#36673=CARTESIAN_POINT('Ctrl Pts',(-55.8593577624554,-127.973267653194,
171.292088182427));
#36674=CARTESIAN_POINT('Ctrl Pts',(-55.8373725464286,-127.978061876224,
171.310595679201));
#36675=CARTESIAN_POINT('Ctrl Pts',(-55.8220085859679,-127.982414522262,
171.322126639961));
#36676=CARTESIAN_POINT('Ctrl Pts',(-55.771276463049,-128.000058531638,171.355984615275));
#36677=CARTESIAN_POINT('Ctrl Pts',(-55.7350955791204,-128.017468294655,
171.373844453765));
#36678=CARTESIAN_POINT('Ctrl Pts',(-55.6635008647466,-128.06277350345,171.399499908916));
#36679=CARTESIAN_POINT('Ctrl Pts',(-55.6291437655714,-128.090112619721,
171.406901422608));
#36680=CARTESIAN_POINT('Ctrl Pts',(-55.5575059846342,-128.161593178447,
171.414811947171));
#36681=CARTESIAN_POINT('Ctrl Pts',(-55.5231251793449,-128.207015666787,
171.412939180716));
#36682=CARTESIAN_POINT('Ctrl Pts',(-55.4574581402791,-128.3220231299,171.402536858845));
#36683=CARTESIAN_POINT('Ctrl Pts',(-55.4295293586655,-128.396417413887,
171.391823517646));
#36684=CARTESIAN_POINT('Ctrl Pts',(-55.39303563214,-128.572648449912,171.371683302053));
#36685=CARTESIAN_POINT('Ctrl Pts',(-55.3875062622141,-128.676541233066,
171.363010864448));
#36686=CARTESIAN_POINT('Ctrl Pts',(-55.3991177156403,-128.785459861137,
171.363010864448));
#36687=CARTESIAN_POINT('Origin',(-60.6261834003547,-128.228219737673,175.985485069079));
#36688=CARTESIAN_POINT('Origin',(-61.1562134225954,-133.200047185959,175.985485069079));
#36689=CARTESIAN_POINT('',(-64.9260520676523,-133.803823638448,180.720859456143));
#36690=CARTESIAN_POINT('Origin',(-61.2622194270436,-134.194412675616,175.985485069079));
#36691=CARTESIAN_POINT('',(-65.4306848366389,-132.74435997593,181.510088520653));
#36692=CARTESIAN_POINT('Origin',(-64.8200460632041,-132.809458148791,180.720859456143));
#36693=CARTESIAN_POINT('Origin',(-61.1562134225954,-133.200047185959,175.985485069079));
#36694=CARTESIAN_POINT('Origin',(-61.1562134225954,-133.200047185959,175.985485069079));
#36695=CARTESIAN_POINT('Origin',(-61.1562134225954,-133.200047185959,175.985485069079));
#36696=CARTESIAN_POINT('Origin',(-61.1562134225954,-133.200047185959,175.985485069079));
#36697=CARTESIAN_POINT('Origin',(-61.1562134225954,-133.200047185959,175.985485069079));
#36698=CARTESIAN_POINT('',(-67.6896254280408,-132.503541817143,173.57106840282));
#36699=CARTESIAN_POINT('Origin',(-61.1562134225954,-133.200047185959,175.985485069079));
#36700=CARTESIAN_POINT('',(-67.3074920698659,-132.544279786117,172.709551595863));
#36701=CARTESIAN_POINT('Ctrl Pts',(-67.3074920698659,-132.544279786117,
172.709551595863));
#36702=CARTESIAN_POINT('Ctrl Pts',(-67.3213669724068,-132.67443018968,172.709551595863));
#36703=CARTESIAN_POINT('Ctrl Pts',(-67.314188693838,-132.797593989444,172.727065098828));
#36704=CARTESIAN_POINT('Ctrl Pts',(-67.2857981445578,-132.987963696479,
172.787746798755));
#36705=CARTESIAN_POINT('Ctrl Pts',(-67.2682462657113,-133.061215883421,
172.824928282536));
#36706=CARTESIAN_POINT('Ctrl Pts',(-67.2430027271334,-133.165987489591,
172.908253961851));
#36707=CARTESIAN_POINT('Ctrl Pts',(-67.2337177246049,-133.204037027031,
172.94939811266));
#36708=CARTESIAN_POINT('Ctrl Pts',(-67.2263641167085,-133.259423139356,
173.035734114708));
#36709=CARTESIAN_POINT('Ctrl Pts',(-67.2266408565468,-133.278607705306,
173.077409586198));
#36710=CARTESIAN_POINT('Ctrl Pts',(-67.2363995797138,-133.301276137252,
173.152425486572));
#36711=CARTESIAN_POINT('Ctrl Pts',(-67.2431784009463,-133.307503498284,
173.184190691894));
#36712=CARTESIAN_POINT('Ctrl Pts',(-67.2565444356024,-133.311515600807,
173.227300136152));
#36713=CARTESIAN_POINT('Ctrl Pts',(-67.2605366896921,-133.312145407734,
173.2388420587));
#36714=CARTESIAN_POINT('Ctrl Pts',(-67.2677258547293,-133.31242843589,173.257579952797));
#36715=CARTESIAN_POINT('Ctrl Pts',(-67.2706848768904,-133.312353441349,
173.264832344081));
#36716=CARTESIAN_POINT('Ctrl Pts',(-67.2766858774409,-133.31184718488,173.278684113163));
#36717=CARTESIAN_POINT('Ctrl Pts',(-67.2797023422905,-133.311444226428,
173.285287857823));
#36718=CARTESIAN_POINT('Ctrl Pts',(-67.286942905684,-133.310144662432,173.300337630055));
#36719=CARTESIAN_POINT('Ctrl Pts',(-67.291252197792,-133.309138609115,173.308733333975));
#36720=CARTESIAN_POINT('Ctrl Pts',(-67.3050989338295,-133.305212002425,
173.334065357106));
#36721=CARTESIAN_POINT('Ctrl Pts',(-67.3152715979195,-133.301412783262,
173.350498333212));
#36722=CARTESIAN_POINT('Ctrl Pts',(-67.3503518756773,-133.285437365149,
173.400952094059));
#36723=CARTESIAN_POINT('Ctrl Pts',(-67.3775915697648,-133.268980792704,
173.431255729657));
#36724=CARTESIAN_POINT('Ctrl Pts',(-67.4348913803985,-133.22519951615,173.482602579355));
#36725=CARTESIAN_POINT('Ctrl Pts',(-67.4641104955011,-133.198408143308,
173.50287782537));
#36726=CARTESIAN_POINT('Ctrl Pts',(-67.527631169734,-133.127792922386,173.538691689326));
#36727=CARTESIAN_POINT('Ctrl Pts',(-67.5600714357955,-133.082577308493,
173.551017551226));
#36728=CARTESIAN_POINT('Ctrl Pts',(-67.6242802655126,-132.967725300239,
173.569274803976));
#36729=CARTESIAN_POINT('Ctrl Pts',(-67.6536643492743,-132.893175871321,
173.572148874503));
#36730=CARTESIAN_POINT('Ctrl Pts',(-67.6937019906102,-132.716567030299,
173.57319909736));
#36731=CARTESIAN_POINT('Ctrl Pts',(-67.701236881467,-132.612460445214,173.57106840282));
#36732=CARTESIAN_POINT('Ctrl Pts',(-67.6896254280408,-132.503541817143,
173.57106840282));
#36733=CARTESIAN_POINT('',(-66.9252242844245,-132.585032085936,172.068819382192));
#36734=CARTESIAN_POINT('Origin',(-61.1562134225954,-133.200047185959,175.985485069079));
#36735=CARTESIAN_POINT('',(-66.3491822523538,-132.646442015031,171.324305384935));
#36736=CARTESIAN_POINT('Ctrl Pts',(-66.3491822523538,-132.646442015031,
171.324305384935));
#36737=CARTESIAN_POINT('Ctrl Pts',(-66.3630571548947,-132.776592418594,
171.324305384935));
#36738=CARTESIAN_POINT('Ctrl Pts',(-66.3606300089676,-132.899249715877,
171.346142702252));
#36739=CARTESIAN_POINT('Ctrl Pts',(-66.348078523136,-133.087930872927,171.416646592413));
#36740=CARTESIAN_POINT('Ctrl Pts',(-66.3401032840752,-133.160162126088,
171.458782749188));
#36741=CARTESIAN_POINT('Ctrl Pts',(-66.3357347296167,-133.262708319488,
171.548352210971));
#36742=CARTESIAN_POINT('Ctrl Pts',(-66.3366240056125,-133.299673210864,
171.591475588748));
#36743=CARTESIAN_POINT('Ctrl Pts',(-66.3501964657754,-133.352828464529,
171.678457825844));
#36744=CARTESIAN_POINT('Ctrl Pts',(-66.3604414133021,-133.370950352943,
171.719343120144));
#36745=CARTESIAN_POINT('Ctrl Pts',(-66.3878405119482,-133.39173820301,171.790432011517));
#36746=CARTESIAN_POINT('Ctrl Pts',(-66.4020027189591,-133.397178445789,
171.819819021622));
#36747=CARTESIAN_POINT('Ctrl Pts',(-66.4252556497954,-133.400136539126,
171.85859688805));
#36748=CARTESIAN_POINT('Ctrl Pts',(-66.4318817283628,-133.400485562767,
171.868869375135));
#36749=CARTESIAN_POINT('Ctrl Pts',(-66.4433242086511,-133.400315159102,
171.88535917445));
#36750=CARTESIAN_POINT('Ctrl Pts',(-66.4479238150429,-133.400065267322,
171.891694771565));
#36751=CARTESIAN_POINT('Ctrl Pts',(-66.4570471135294,-133.399226153033,
171.903703148721));
#36752=CARTESIAN_POINT('Ctrl Pts',(-66.4615471509932,-133.398665035829,
171.909386958144));
#36753=CARTESIAN_POINT('Ctrl Pts',(-66.4721570532479,-133.3970062778,171.922243425969));
#36754=CARTESIAN_POINT('Ctrl Pts',(-66.4783373532359,-133.395800762543,
171.929344173189));
#36755=CARTESIAN_POINT('Ctrl Pts',(-66.4978024141607,-133.391275204884,
171.95054541056));
#36756=CARTESIAN_POINT('Ctrl Pts',(-66.5115816738262,-133.387091498538,
171.963983731472));
#36757=CARTESIAN_POINT('Ctrl Pts',(-66.5576114470216,-133.369948791058,
172.004218162185));
#36758=CARTESIAN_POINT('Ctrl Pts',(-66.5912293660221,-133.352812257225,
172.026741589352));
#36759=CARTESIAN_POINT('Ctrl Pts',(-66.6589676252424,-133.307918172314,
172.061850232547));
#36760=CARTESIAN_POINT('Ctrl Pts',(-66.692090009718,-133.280710684879,172.073903457065));
#36761=CARTESIAN_POINT('Ctrl Pts',(-66.7620918631791,-133.209404526951,
172.091769365546));
#36762=CARTESIAN_POINT('Ctrl Pts',(-66.7963947234741,-133.163990348069,
172.094870269528));
#36763=CARTESIAN_POINT('Ctrl Pts',(-66.8627515656631,-133.048909347335,
172.094403733039));
#36764=CARTESIAN_POINT('Ctrl Pts',(-66.891746987074,-132.974401352419,172.088310602244));
#36765=CARTESIAN_POINT('Ctrl Pts',(-66.9303432492909,-132.797946172042,
172.075322289057));
#36766=CARTESIAN_POINT('Ctrl Pts',(-66.9368357378507,-132.693950714007,
172.068819382192));
#36767=CARTESIAN_POINT('Ctrl Pts',(-66.9252242844245,-132.585032085936,
172.068819382192));
#36768=CARTESIAN_POINT('',(-65.82554919902,-132.702264796853,170.794192734786));
#36769=CARTESIAN_POINT('Origin',(-61.1562134225954,-133.200047185959,175.985485069079));
#36770=CARTESIAN_POINT('',(-65.0890759621299,-132.780777764206,170.209949994551));
#36771=CARTESIAN_POINT('Ctrl Pts',(-65.0890759621299,-132.780777764206,
170.209949994551));
#36772=CARTESIAN_POINT('Ctrl Pts',(-65.1029508646709,-132.910928167769,
170.209949994551));
#36773=CARTESIAN_POINT('Ctrl Pts',(-65.1061657182635,-133.03298399021,170.234842020713));
#36774=CARTESIAN_POINT('Ctrl Pts',(-65.1113304009609,-133.219776485334,
170.311070671283));
#36775=CARTESIAN_POINT('Ctrl Pts',(-65.1138325717848,-133.290890776603,
170.355712700779));
#36776=CARTESIAN_POINT('Ctrl Pts',(-65.1312182280125,-133.391117825806,
170.446320493482));
#36777=CARTESIAN_POINT('Ctrl Pts',(-65.142457127664,-133.426979378156,170.488916924258));
#36778=CARTESIAN_POINT('Ctrl Pts',(-65.1765013651493,-133.477952203588,
170.571490304949));
#36779=CARTESIAN_POINT('Ctrl Pts',(-65.1962368260823,-133.495062339868,
170.609209317368));
#36780=CARTESIAN_POINT('Ctrl Pts',(-65.2398292034717,-133.514123878235,
170.67223977177));
#36781=CARTESIAN_POINT('Ctrl Pts',(-65.2605943159424,-133.51886020718,170.697540720449));
#36782=CARTESIAN_POINT('Ctrl Pts',(-65.2924160741141,-133.520904806275,
170.729733380401));
#36783=CARTESIAN_POINT('Ctrl Pts',(-65.3012973589557,-133.521013409861,
170.738139432412));
#36784=CARTESIAN_POINT('Ctrl Pts',(-65.3163345879792,-133.520459781964,
170.751422809749));
#36785=CARTESIAN_POINT('Ctrl Pts',(-65.3223089392296,-133.520063333198,
170.75647341082));
#36786=CARTESIAN_POINT('Ctrl Pts',(-65.3340251404624,-133.518947798153,
170.765940512815));
#36787=CARTESIAN_POINT('Ctrl Pts',(-65.3397467261682,-133.518256455745,
170.770374064657));
#36788=CARTESIAN_POINT('Ctrl Pts',(-65.3531061258319,-133.516304582923,
170.780290056899));
#36789=CARTESIAN_POINT('Ctrl Pts',(-65.3607949083432,-133.514938253351,
170.785683177801));
#36790=CARTESIAN_POINT('Ctrl Pts',(-65.3847320441665,-133.509935942631,
170.801521490557));
#36791=CARTESIAN_POINT('Ctrl Pts',(-65.4013004684702,-133.5054548927,170.81118416991));
#36792=CARTESIAN_POINT('Ctrl Pts',(-65.4555296989026,-133.487438068299,
170.838860991624));
#36793=CARTESIAN_POINT('Ctrl Pts',(-65.4934890684829,-133.46983870683,170.852295230642));
#36794=CARTESIAN_POINT('Ctrl Pts',(-65.5674982927985,-133.424276095143,
170.869125280607));
#36795=CARTESIAN_POINT('Ctrl Pts',(-65.602453952989,-133.396873168269,170.87225599403));
#36796=CARTESIAN_POINT('Ctrl Pts',(-65.6744776290023,-133.32535147055,170.871135645376));
#36797=CARTESIAN_POINT('Ctrl Pts',(-65.7083937221736,-133.279978523627,
170.86483137817));
#36798=CARTESIAN_POINT('Ctrl Pts',(-65.7723805110916,-133.165150186405,
170.845668165849));
#36799=CARTESIAN_POINT('Ctrl Pts',(-65.7988646638445,-133.090909909506,
170.830961944344));
#36800=CARTESIAN_POINT('Ctrl Pts',(-65.832720719157,-132.914960066854,170.804689928667));
#36801=CARTESIAN_POINT('Ctrl Pts',(-65.8371606524461,-132.811183424923,
170.794192734786));
#36802=CARTESIAN_POINT('Ctrl Pts',(-65.82554919902,-132.702264796853,170.794192734786));
#36803=CARTESIAN_POINT('',(-64.4545092906346,-132.84842681086,169.821265128268));
#36804=CARTESIAN_POINT('Origin',(-61.1562134225954,-133.200047185959,175.985485069079));
#36805=CARTESIAN_POINT('',(-63.6004059964818,-132.93947992819,169.431247709482));
#36806=CARTESIAN_POINT('Ctrl Pts',(-63.6004059964818,-132.93947992819,169.431247709482));
#36807=CARTESIAN_POINT('Ctrl Pts',(-63.6142808990228,-133.069630331754,
169.431247709482));
#36808=CARTESIAN_POINT('Ctrl Pts',(-63.623700726509,-133.191024662523,169.457747810408));
#36809=CARTESIAN_POINT('Ctrl Pts',(-63.6474290834969,-133.375838145946,
169.535271089296));
#36810=CARTESIAN_POINT('Ctrl Pts',(-63.6607005253255,-133.445804360977,
169.579824559026));
#36811=CARTESIAN_POINT('Ctrl Pts',(-63.6994553431546,-133.543753314789,
169.666204887084));
#36812=CARTESIAN_POINT('Ctrl Pts',(-63.7206177290859,-133.578556957203,
169.705798821133));
#36813=CARTESIAN_POINT('Ctrl Pts',(-63.7734897078701,-133.627522619627,
169.779164480675));
#36814=CARTESIAN_POINT('Ctrl Pts',(-63.8016864337849,-133.643730728531,
169.811525119313));
#36815=CARTESIAN_POINT('Ctrl Pts',(-63.8590838986816,-133.661320552339,
169.862834035842));
#36816=CARTESIAN_POINT('Ctrl Pts',(-63.8852876994291,-133.665477080778,
169.882578523923));
#36817=CARTESIAN_POINT('Ctrl Pts',(-63.9238622269919,-133.666801789542,
169.906315057018));
#36818=CARTESIAN_POINT('Ctrl Pts',(-63.9344890355132,-133.666724308642,
169.912366144767));
#36819=CARTESIAN_POINT('Ctrl Pts',(-63.9522535330249,-133.665879935704,
169.921671118517));
#36820=CARTESIAN_POINT('Ctrl Pts',(-63.9592568945881,-133.665373787563,
169.925143200968));
#36821=CARTESIAN_POINT('Ctrl Pts',(-63.9728859132973,-133.664054333396,
169.931518834248));
#36822=CARTESIAN_POINT('Ctrl Pts',(-63.9794960309314,-133.663268267548,
169.93444446659));
#36823=CARTESIAN_POINT('Ctrl Pts',(-63.9948252957511,-133.66110639394,169.940843701822));
#36824=CARTESIAN_POINT('Ctrl Pts',(-64.0035723679062,-133.659627243622,
169.944215767822));
#36825=CARTESIAN_POINT('Ctrl Pts',(-64.0305754279041,-133.654298084902,
169.953770690797));
#36826=CARTESIAN_POINT('Ctrl Pts',(-64.0489534897979,-133.649624115514,
169.959096168788));
#36827=CARTESIAN_POINT('Ctrl Pts',(-64.1081556166164,-133.631077147135,
169.972606905226));
#36828=CARTESIAN_POINT('Ctrl Pts',(-64.1481673531163,-133.61325898964,169.976171206955));
#36829=CARTESIAN_POINT('Ctrl Pts',(-64.223915613338,-133.567510985108,169.973744562361));
#36830=CARTESIAN_POINT('Ctrl Pts',(-64.258528012264,-133.540144652178,169.967770819004));
#36831=CARTESIAN_POINT('Ctrl Pts',(-64.3279966531765,-133.468895338271,
169.947729323807));
#36832=CARTESIAN_POINT('Ctrl Pts',(-64.3592990953663,-133.423801024004,
169.93238626651));
#36833=CARTESIAN_POINT('Ctrl Pts',(-64.4165355041514,-133.309692322405,
169.8956400746));
#36834=CARTESIAN_POINT('Ctrl Pts',(-64.438531727746,-133.235930488738,169.873175434526));
#36835=CARTESIAN_POINT('Ctrl Pts',(-64.4646242319639,-133.060808292499,
169.835146550413));
#36836=CARTESIAN_POINT('Ctrl Pts',(-64.4661207440609,-132.957345438932,
169.821265128269));
#36837=CARTESIAN_POINT('Ctrl Pts',(-64.4545092906346,-132.84842681086,169.821265128269));
#36838=CARTESIAN_POINT('',(-62.8917844152165,-133.015023722979,169.206579578684));
#36839=CARTESIAN_POINT('Origin',(-61.1562134225954,-133.200047185959,175.985485069079));
#36840=CARTESIAN_POINT('',(-61.969688442718,-133.113325314073,169.03345387607));
#36841=CARTESIAN_POINT('Ctrl Pts',(-61.969688442718,-133.113325314073,169.03345387607));
#36842=CARTESIAN_POINT('Ctrl Pts',(-61.983563345259,-133.243475717636,169.03345387607));
#36843=CARTESIAN_POINT('Ctrl Pts',(-61.9993905104838,-133.364186983395,
169.060021962217));
#36844=CARTESIAN_POINT('Ctrl Pts',(-62.0414511942499,-133.547046118307,
169.134334498239));
#36845=CARTESIAN_POINT('Ctrl Pts',(-62.0651578973172,-133.615899864773,
169.176210122489));
#36846=CARTESIAN_POINT('Ctrl Pts',(-62.1236549296646,-133.711744166623,
169.253342875213));
#36847=CARTESIAN_POINT('Ctrl Pts',(-62.1537379475471,-133.745596810073,
169.287633257008));
#36848=CARTESIAN_POINT('Ctrl Pts',(-62.2226994317192,-133.79284722373,169.347527449942));
#36849=CARTESIAN_POINT('Ctrl Pts',(-62.2578364362259,-133.808315452569,
169.372649032107));
#36850=CARTESIAN_POINT('Ctrl Pts',(-62.3258484958873,-133.824773689661,
169.409254523035));
#36851=CARTESIAN_POINT('Ctrl Pts',(-62.3560106909347,-133.828508226822,
169.422295072638));
#36852=CARTESIAN_POINT('Ctrl Pts',(-62.3991294835324,-133.829348486573,
169.436195997852));
#36853=CARTESIAN_POINT('Ctrl Pts',(-62.4108906896479,-133.82915007131,169.439540454114));
#36854=CARTESIAN_POINT('Ctrl Pts',(-62.4303564764721,-133.828124329566,
169.444326253026));
#36855=CARTESIAN_POINT('Ctrl Pts',(-62.4379833114621,-133.827551714992,
169.446018032044));
#36856=CARTESIAN_POINT('Ctrl Pts',(-62.4527338963768,-133.826112694374,
169.448931667977));
#36857=CARTESIAN_POINT('Ctrl Pts',(-62.4598478913784,-133.825272911833,
169.450179353702));
#36858=CARTESIAN_POINT('Ctrl Pts',(-62.4762529077012,-133.822996355928,
169.452689931634));
#36859=CARTESIAN_POINT('Ctrl Pts',(-62.4855465726741,-133.821458935164,
169.453844970513));
#36860=CARTESIAN_POINT('Ctrl Pts',(-62.5140312257525,-133.815971828722,
169.456561206314));
#36861=CARTESIAN_POINT('Ctrl Pts',(-62.5331342286297,-133.811220575783,
169.45723998552));
#36862=CARTESIAN_POINT('Ctrl Pts',(-62.5937936843215,-133.79251824641,169.455799441789));
#36863=CARTESIAN_POINT('Ctrl Pts',(-62.6334494279754,-133.774738040131,
169.449286661968));
#36864=CARTESIAN_POINT('Ctrl Pts',(-62.7063037284689,-133.72929855104,169.427744350578));
#36865=CARTESIAN_POINT('Ctrl Pts',(-62.7384162782486,-133.70219871873,169.413013322693));
#36866=CARTESIAN_POINT('Ctrl Pts',(-62.800901515759,-133.631693882281,169.375215419805));
#36867=CARTESIAN_POINT('Ctrl Pts',(-62.8275153190044,-133.58709940825,169.351725255135));
#36868=CARTESIAN_POINT('Ctrl Pts',(-62.8740133283526,-133.474135491771,
169.299531638744));
#36869=CARTESIAN_POINT('Ctrl Pts',(-62.8898057844172,-133.40103502117,169.270614143326));
#36870=CARTESIAN_POINT('Ctrl Pts',(-62.9055625827193,-133.227014680234,
169.223038491293));
#36871=CARTESIAN_POINT('Ctrl Pts',(-62.9033958686428,-133.123942351051,
169.206579578684));
#36872=CARTESIAN_POINT('Ctrl Pts',(-62.8917844152165,-133.015023722979,
169.206579578684));
#36873=CARTESIAN_POINT('',(-61.2281944622511,-133.192373526234,168.985859375881));
#36874=CARTESIAN_POINT('Origin',(-61.1562134225954,-133.200047185959,175.985485069079));
#36875=CARTESIAN_POINT('',(-60.2916946776461,-133.292210659929,169.03968682599));
#36876=CARTESIAN_POINT('Ctrl Pts',(-60.2916946776461,-133.292210659929,
169.03968682599));
#36877=CARTESIAN_POINT('Ctrl Pts',(-60.3055695801871,-133.422361063493,
169.03968682599));
#36878=CARTESIAN_POINT('Ctrl Pts',(-60.3276340758163,-133.54240738816,169.064778856764));
#36879=CARTESIAN_POINT('Ctrl Pts',(-60.386730330652,-133.723450417383,169.131561875442));
#36880=CARTESIAN_POINT('Ctrl Pts',(-60.4199318257402,-133.791291955586,
169.168325995141));
#36881=CARTESIAN_POINT('Ctrl Pts',(-60.4953967797734,-133.885327363622,
169.23172849731));
#36882=CARTESIAN_POINT('Ctrl Pts',(-60.5328791405755,-133.918391187683,
169.2587224945));
#36883=CARTESIAN_POINT('Ctrl Pts',(-60.6142568306537,-133.964317950839,
169.301664388039));
#36884=CARTESIAN_POINT('Ctrl Pts',(-60.6544097835976,-133.979251446064,
169.31808693869));
#36885=CARTESIAN_POINT('Ctrl Pts',(-60.7292290636159,-133.994983987987,
169.337861625938));
#36886=CARTESIAN_POINT('Ctrl Pts',(-60.7616393114978,-133.998478867696,
169.343440367722));
#36887=CARTESIAN_POINT('Ctrl Pts',(-60.8068297686094,-133.99909827417,169.346697813809));
#36888=CARTESIAN_POINT('Ctrl Pts',(-60.8190483191676,-133.998851102934,
169.347141270942));
#36889=CARTESIAN_POINT('Ctrl Pts',(-60.8390905433741,-133.997763909113,
169.347129761778));
#36890=CARTESIAN_POINT('Ctrl Pts',(-60.8468990808967,-133.997171923836,
169.346942917318));
#36891=CARTESIAN_POINT('Ctrl Pts',(-60.8619147993941,-133.995704638207,
169.346225225972));
#36892=CARTESIAN_POINT('Ctrl Pts',(-60.8691187336791,-133.994855267537,
169.345722454122));
#36893=CARTESIAN_POINT('Ctrl Pts',(-60.8856428690902,-133.992566012741,
169.344198469089));
#36894=CARTESIAN_POINT('Ctrl Pts',(-60.8949396640679,-133.991028258298,
169.343069354186));
#36895=CARTESIAN_POINT('Ctrl Pts',(-60.9232354743277,-133.985561283762,
169.338789045061));
#36896=CARTESIAN_POINT('Ctrl Pts',(-60.9419365906471,-133.980852874615,
169.334781677302));
#36897=CARTESIAN_POINT('Ctrl Pts',(-61.0004531130408,-133.962378996248,
169.318473572569));
#36898=CARTESIAN_POINT('Ctrl Pts',(-61.0373651930932,-133.944891282839,
169.302262210288));
#36899=CARTESIAN_POINT('Ctrl Pts',(-61.1028607246446,-133.90023628768,169.262856192937));
#36900=CARTESIAN_POINT('Ctrl Pts',(-61.1304621195415,-133.873617374619,
169.240223994317));
#36901=CARTESIAN_POINT('Ctrl Pts',(-61.1819414353715,-133.804285842951,
169.186866360465));
#36902=CARTESIAN_POINT('Ctrl Pts',(-61.2020640983622,-133.760383367837,
169.156594251411));
#36903=CARTESIAN_POINT('Ctrl Pts',(-61.2344597657111,-133.648922855231,
169.091986513806));
#36904=CARTESIAN_POINT('Ctrl Pts',(-61.2426931562934,-133.576628231511,
169.058296742767));
#36905=CARTESIAN_POINT('Ctrl Pts',(-61.2461427675187,-133.403919918941,
169.00393924678));
#36906=CARTESIAN_POINT('Ctrl Pts',(-61.2398059156773,-133.301292154304,
168.985859375881));
#36907=CARTESIAN_POINT('Ctrl Pts',(-61.2281944622511,-133.192373526234,
168.985859375881));
#36908=CARTESIAN_POINT('',(-59.5604212329013,-133.370169294699,169.171931975764));
#36909=CARTESIAN_POINT('Origin',(-61.1562134225954,-133.200047185959,175.985485069079));
#36910=CARTESIAN_POINT('',(-58.6639435996328,-133.465739799678,169.44958432285));
#36911=CARTESIAN_POINT('Ctrl Pts',(-58.6639435996328,-133.465739799678,
169.44958432285));
#36912=CARTESIAN_POINT('Ctrl Pts',(-58.6778185021737,-133.59589020324,169.44958432285));
#36913=CARTESIAN_POINT('Ctrl Pts',(-58.7055878299011,-133.715328354692,
169.471742040625));
#36914=CARTESIAN_POINT('Ctrl Pts',(-58.7794328546285,-133.894799066511,
169.527114355661));
#36915=CARTESIAN_POINT('Ctrl Pts',(-58.8206368697185,-133.961787482618,
169.556630373804));
#36916=CARTESIAN_POINT('Ctrl Pts',(-58.9093093386745,-134.054414881325,
169.602617902451));
#36917=CARTESIAN_POINT('Ctrl Pts',(-58.952239730449,-134.086897908887,169.620746722039));
#36918=CARTESIAN_POINT('Ctrl Pts',(-59.0416387421954,-134.131969545564,
169.644240689419));
#36919=CARTESIAN_POINT('Ctrl Pts',(-59.0845918047307,-134.146604530399,
169.651009789604));
#36920=CARTESIAN_POINT('Ctrl Pts',(-59.162015319794,-134.162059443467,169.652804440229));
#36921=CARTESIAN_POINT('Ctrl Pts',(-59.1948326303858,-134.165510927573,
169.650597157998));
#36922=CARTESIAN_POINT('Ctrl Pts',(-59.2395017538799,-134.166185911693,
169.643021814031));
#36923=CARTESIAN_POINT('Ctrl Pts',(-59.2514740165327,-134.165964996393,
169.64053849992));
#36924=CARTESIAN_POINT('Ctrl Pts',(-59.2709343257464,-134.164939838598,
169.635730351551));
#36925=CARTESIAN_POINT('Ctrl Pts',(-59.2784722350168,-134.164376704101,
169.633675742333));
#36926=CARTESIAN_POINT('Ctrl Pts',(-59.2928812458769,-134.162974097559,
169.629368433322));
#36927=CARTESIAN_POINT('Ctrl Pts',(-59.2997559544205,-134.162159824553,
169.627144423168));
#36928=CARTESIAN_POINT('Ctrl Pts',(-59.3154356537289,-134.159960592287,
169.621674443641));
#36929=CARTESIAN_POINT('Ctrl Pts',(-59.3241919339931,-134.158480460323,
169.61832679501));
#36930=CARTESIAN_POINT('Ctrl Pts',(-59.3506394403934,-134.153210527328,
169.607298696968));
#36931=CARTESIAN_POINT('Ctrl Pts',(-59.3678351987989,-134.148662599391,
169.598838075892));
#36932=CARTESIAN_POINT('Ctrl Pts',(-59.4207330652189,-134.130787707288,
169.568610177924));
#36933=CARTESIAN_POINT('Ctrl Pts',(-59.4526732626702,-134.113830029781,
169.543642378634));
#36934=CARTESIAN_POINT('Ctrl Pts',(-59.5067728809681,-134.07038991511,169.488662789815));
#36935=CARTESIAN_POINT('Ctrl Pts',(-59.5281139871706,-134.044438390648,
169.459444721581));
#36936=CARTESIAN_POINT('Ctrl Pts',(-59.5652044872045,-133.976640802874,
169.393628308496));
#36937=CARTESIAN_POINT('Ctrl Pts',(-59.5774107501079,-133.933582268898,
169.358333560002));
#36938=CARTESIAN_POINT('Ctrl Pts',(-59.5931597097522,-133.823896406549,
169.285066468054));
#36939=CARTESIAN_POINT('Ctrl Pts',(-59.5929180423105,-133.752505280635,
169.248562348429));
#36940=CARTESIAN_POINT('Ctrl Pts',(-59.5828042342757,-133.581242919175,
169.190582068574));
#36941=CARTESIAN_POINT('Ctrl Pts',(-59.5720326863276,-133.479087922771,
169.171931975764));
#36942=CARTESIAN_POINT('Ctrl Pts',(-59.5604212329013,-133.370169294699,
169.171931975764));
#36943=CARTESIAN_POINT('',(-57.985389645148,-133.538078184573,169.753983515172));
#36944=CARTESIAN_POINT('Origin',(-61.1562134225954,-133.200047185959,175.985485069079));
#36945=CARTESIAN_POINT('',(-57.1810341846979,-133.623827850471,170.239324614047));
#36946=CARTESIAN_POINT('Ctrl Pts',(-57.1810341846979,-133.623827850471,
170.239324614047));
#36947=CARTESIAN_POINT('Ctrl Pts',(-57.1949090872389,-133.753978254034,
170.239324614047));
#36948=CARTESIAN_POINT('Ctrl Pts',(-57.2275192046538,-133.872900344965,
170.257260292809));
#36949=CARTESIAN_POINT('Ctrl Pts',(-57.312969053198,-134.051133905033,170.298003866522));
#36950=CARTESIAN_POINT('Ctrl Pts',(-57.3602182388967,-134.117477865566,
170.318556419421));
#36951=CARTESIAN_POINT('Ctrl Pts',(-57.4575702432519,-134.209179967813,
170.344456346538));
#36952=CARTESIAN_POINT('Ctrl Pts',(-57.5036807342943,-134.241323975547,
170.352666407426));
#36953=CARTESIAN_POINT('Ctrl Pts',(-57.5962400134122,-134.286058706608,
170.355347064658));
#36954=CARTESIAN_POINT('Ctrl Pts',(-57.6396146145018,-134.300648752617,
170.352069318881));
#36955=CARTESIAN_POINT('Ctrl Pts',(-57.7152880306234,-134.316290237925,
170.335779634311));
#36956=CARTESIAN_POINT('Ctrl Pts',(-57.7466477567951,-134.319897110267,
170.325914607286));
#36957=CARTESIAN_POINT('Ctrl Pts',(-57.7882328465512,-134.320900872989,
170.307946724722));
#36958=CARTESIAN_POINT('Ctrl Pts',(-57.7992695023101,-134.320779699634,
170.302680960555));
#36959=CARTESIAN_POINT('Ctrl Pts',(-57.8170233629453,-134.319936460658,
170.293355605087));
#36960=CARTESIAN_POINT('Ctrl Pts',(-57.823854041107,-134.319448721722,170.289552637531));
#36961=CARTESIAN_POINT('Ctrl Pts',(-57.8368197627493,-134.318199979453,
170.281906035998));
#36962=CARTESIAN_POINT('Ctrl Pts',(-57.8429652139283,-134.317463450155,
170.278090038927));
#36963=CARTESIAN_POINT('Ctrl Pts',(-57.856885997503,-134.315451730057,170.268991960234));
#36964=CARTESIAN_POINT('Ctrl Pts',(-57.8645895310856,-134.314083827922,
170.263620331045));
#36965=CARTESIAN_POINT('Ctrl Pts',(-57.8876366892889,-134.309176394762,
170.246485357057));
#36966=CARTESIAN_POINT('Ctrl Pts',(-57.902311104355,-134.30489725887,170.234063183208));
#36967=CARTESIAN_POINT('Ctrl Pts',(-57.9464411279872,-134.287957077386,
170.191672227563));
#36968=CARTESIAN_POINT('Ctrl Pts',(-57.9714701715824,-134.271736175052,
170.159399029004));
#36969=CARTESIAN_POINT('Ctrl Pts',(-58.0107990213713,-134.229870722986,
170.092041082576));
#36970=CARTESIAN_POINT('Ctrl Pts',(-58.024494530291,-134.204734270274,170.05793519265));
#36971=CARTESIAN_POINT('Ctrl Pts',(-58.0446495460863,-134.138742118264,
169.983485011029));
#36972=CARTESIAN_POINT('Ctrl Pts',(-58.0479742214678,-134.096630420855,
169.945218825585));
#36973=CARTESIAN_POINT('Ctrl Pts',(-58.045499553846,-133.988887318923,169.867550396363));
#36974=CARTESIAN_POINT('Ctrl Pts',(-58.0363593754047,-133.918444833732,
169.830353414898));
#36975=CARTESIAN_POINT('Ctrl Pts',(-58.0122141725528,-133.748678312699,
169.772119954288));
#36976=CARTESIAN_POINT('Ctrl Pts',(-57.997001098574,-133.646996812643,169.753983515172));
#36977=CARTESIAN_POINT('Ctrl Pts',(-57.985389645148,-133.538078184573,169.753983515172));
#36978=CARTESIAN_POINT('',(-56.5946348098644,-133.6863419415,170.698187274307));
#36979=CARTESIAN_POINT('Origin',(-61.1562134225954,-133.200047185959,175.985485069079));
#36980=CARTESIAN_POINT('',(-55.929147737881,-133.757287309423,171.363010864448));
#36981=CARTESIAN_POINT('Ctrl Pts',(-55.929147737881,-133.757287309423,171.363010864448));
#36982=CARTESIAN_POINT('Ctrl Pts',(-55.9430226404219,-133.887437712986,
171.363010864448));
#36983=CARTESIAN_POINT('Ctrl Pts',(-55.979328176012,-134.00596584765,171.375682147739));
#36984=CARTESIAN_POINT('Ctrl Pts',(-56.0725644721205,-134.183369320388,
171.399429111723));
#36985=CARTESIAN_POINT('Ctrl Pts',(-56.1235501556925,-134.249314945284,
171.409823759709));
#36986=CARTESIAN_POINT('Ctrl Pts',(-56.2245492928744,-134.340628238806,
171.414130875675));
#36987=CARTESIAN_POINT('Ctrl Pts',(-56.2713871356702,-134.372694705983,
171.411945038965));
#36988=CARTESIAN_POINT('Ctrl Pts',(-56.3620619646102,-134.417630332023,
171.393656595996));
#36989=CARTESIAN_POINT('Ctrl Pts',(-56.4034550349283,-134.432431622451,
171.380522494926));
#36990=CARTESIAN_POINT('Ctrl Pts',(-56.4731257275112,-134.448713038192,
171.347095172418));
#36991=CARTESIAN_POINT('Ctrl Pts',(-56.5012479316411,-134.452665052013,
171.330145720112));
#36992=CARTESIAN_POINT('Ctrl Pts',(-56.5373655203723,-134.454251686872,
171.302829526974));
#36993=CARTESIAN_POINT('Ctrl Pts',(-56.5468316243193,-134.454297944833,
171.295087339825));
#36994=CARTESIAN_POINT('Ctrl Pts',(-56.5618536753716,-134.45374593501,171.281786733023));
#36995=CARTESIAN_POINT('Ctrl Pts',(-56.5675816212726,-134.453375754699,
171.276456421779));
#36996=CARTESIAN_POINT('Ctrl Pts',(-56.5783513508432,-134.452361119857,
171.26591492041));
#36997=CARTESIAN_POINT('Ctrl Pts',(-56.5834098948226,-134.451740462127,
171.260728708301));
#36998=CARTESIAN_POINT('Ctrl Pts',(-56.5947595048212,-134.45000284631,171.248531277705));
#36999=CARTESIAN_POINT('Ctrl Pts',(-56.6009592415656,-134.448795258966,
171.241447847521));
#37000=CARTESIAN_POINT('Ctrl Pts',(-56.6192516231093,-134.444394716763,
171.219201819994));
#37001=CARTESIAN_POINT('Ctrl Pts',(-56.6305352407206,-134.440477062534,
171.203540024964));
#37002=CARTESIAN_POINT('Ctrl Pts',(-56.6632577899041,-134.424752994038,
171.151449619898));
#37003=CARTESIAN_POINT('Ctrl Pts',(-56.6798380595294,-134.409432787455,
171.113746623061));
#37004=CARTESIAN_POINT('Ctrl Pts',(-56.7018797089301,-134.369410266444,
171.037924918036));
#37005=CARTESIAN_POINT('Ctrl Pts',(-56.7069886463024,-134.345189199625,
171.00091331677));
#37006=CARTESIAN_POINT('Ctrl Pts',(-56.7086457382025,-134.281169049884,
170.922156140553));
#37007=CARTESIAN_POINT('Ctrl Pts',(-56.7026398042108,-134.240052057771,
170.883142409765));
#37008=CARTESIAN_POINT('Ctrl Pts',(-56.6814236807383,-134.134306920244,
170.805586450063));
#37009=CARTESIAN_POINT('Ctrl Pts',(-56.6634786874364,-134.064803087141,
170.769858360114));
#37010=CARTESIAN_POINT('Ctrl Pts',(-56.6256495678753,-133.896495363049,
170.714756035812));
#37011=CARTESIAN_POINT('Ctrl Pts',(-56.6062462632905,-133.795260569571,
170.698187274307));
#37012=CARTESIAN_POINT('Ctrl Pts',(-56.5946348098644,-133.6863419415,170.698187274307));
#37013=CARTESIAN_POINT('',(-55.4689823428891,-133.806344014845,171.949669562728));
#37014=CARTESIAN_POINT('Origin',(-61.1562134225954,-133.200047185959,175.985485069079));
#37015=CARTESIAN_POINT('',(-54.981039349049,-133.858361997884,172.755338513612));
#37016=CARTESIAN_POINT('Ctrl Pts',(-54.981039349049,-133.858361997884,172.755338513612));
#37017=CARTESIAN_POINT('Ctrl Pts',(-54.9949142515899,-133.988512401447,
172.755338513612));
#37018=CARTESIAN_POINT('Ctrl Pts',(-55.0335550695708,-134.106791579407,
172.762008992506));
#37019=CARTESIAN_POINT('Ctrl Pts',(-55.1303069169609,-134.283820270891,
172.767379259529));
#37020=CARTESIAN_POINT('Ctrl Pts',(-55.1825032739958,-134.349636829908,
172.767011903445));
#37021=CARTESIAN_POINT('Ctrl Pts',(-55.2819051833289,-134.441120398589,
172.749475894336));
#37022=CARTESIAN_POINT('Ctrl Pts',(-55.3269753593235,-134.473375310857,
172.737021192913));
#37023=CARTESIAN_POINT('Ctrl Pts',(-55.4108305379313,-134.519037957184,
172.698826507572));
#37024=CARTESIAN_POINT('Ctrl Pts',(-55.4479541675179,-134.534294398517,
172.676599357423));
#37025=CARTESIAN_POINT('Ctrl Pts',(-55.507718368438,-134.551631912454,172.627977071457));
#37026=CARTESIAN_POINT('Ctrl Pts',(-55.5310112659176,-134.556098762628,
172.604928234429));
#37027=CARTESIAN_POINT('Ctrl Pts',(-55.5595956376216,-134.55848848875,172.569851248574));
#37028=CARTESIAN_POINT('Ctrl Pts',(-55.566947519602,-134.558760136898,172.560082586218));
#37029=CARTESIAN_POINT('Ctrl Pts',(-55.5783711629161,-134.55859174138,172.543579711001));
#37030=CARTESIAN_POINT('Ctrl Pts',(-55.5826649621923,-134.558374450681,
172.537031834384));
#37031=CARTESIAN_POINT('Ctrl Pts',(-55.590613619911,-134.557660560946,172.524208066924));
#37032=CARTESIAN_POINT('Ctrl Pts',(-55.5942907739505,-134.557187168612,
172.517953043574));
#37033=CARTESIAN_POINT('Ctrl Pts',(-55.6024063797937,-134.555794319245,
172.503365131405));
#37034=CARTESIAN_POINT('Ctrl Pts',(-55.6067386647482,-134.554785814737,
172.494981563442));
#37035=CARTESIAN_POINT('Ctrl Pts',(-55.6191981715094,-134.551007095955,
172.468917340633));
#37036=CARTESIAN_POINT('Ctrl Pts',(-55.6264185983737,-134.547522605005,
172.45092613102));
#37037=CARTESIAN_POINT('Ctrl Pts',(-55.6457570023975,-134.533225375801,
172.392163581535));
#37038=CARTESIAN_POINT('Ctrl Pts',(-55.652841889972,-134.518917440383,172.351221947552));
#37039=CARTESIAN_POINT('Ctrl Pts',(-55.6560845763555,-134.480899014423,
172.271342965824));
#37040=CARTESIAN_POINT('Ctrl Pts',(-55.6521649882432,-134.45764044874,172.233576632953));
#37041=CARTESIAN_POINT('Ctrl Pts',(-55.634836748691,-134.395644262171,172.15508954295));
#37042=CARTESIAN_POINT('Ctrl Pts',(-55.6195934445764,-134.355512035427,
172.117595603043));
#37043=CARTESIAN_POINT('Ctrl Pts',(-55.5802072219595,-134.25170395186,172.044659383334));
#37044=CARTESIAN_POINT('Ctrl Pts',(-55.5540628137713,-134.183074231163,
172.012476571624));
#37045=CARTESIAN_POINT('Ctrl Pts',(-55.5036925151093,-134.016103480551,
171.963707730429));
#37046=CARTESIAN_POINT('Ctrl Pts',(-55.4805937963153,-133.915262642916,
171.949669562728));
#37047=CARTESIAN_POINT('Ctrl Pts',(-55.4689823428892,-133.806344014845,
171.949669562728));
#37048=CARTESIAN_POINT('',(-54.6738510740226,-133.891110320294,173.435698778786));
#37049=CARTESIAN_POINT('Origin',(-61.1562134225954,-133.200047185959,175.985485069079));
#37050=CARTESIAN_POINT('',(-54.391809631527,-133.921177822353,174.335390539474));
#37051=CARTESIAN_POINT('Ctrl Pts',(-54.3918096315271,-133.921177822353,
174.335390539474));
#37052=CARTESIAN_POINT('Ctrl Pts',(-54.405684534068,-134.051328225917,174.335390539474));
#37053=CARTESIAN_POINT('Ctrl Pts',(-54.4451647805315,-134.169517915192,
174.335672549985));
#37054=CARTESIAN_POINT('Ctrl Pts',(-54.5409569718588,-134.346648912425,
174.322354019649));
#37055=CARTESIAN_POINT('Ctrl Pts',(-54.5917678180055,-134.412613176158,
174.311246008893));
#37056=CARTESIAN_POINT('Ctrl Pts',(-54.6844209638907,-134.50481620811,174.272886003818));
#37057=CARTESIAN_POINT('Ctrl Pts',(-54.7253311848986,-134.537514599372,
174.250886259657));
#37058=CARTESIAN_POINT('Ctrl Pts',(-54.797827846308,-134.584388139517,174.195005068225));
#37059=CARTESIAN_POINT('Ctrl Pts',(-54.82864224958,-134.600317186527,174.164976630171));
#37060=CARTESIAN_POINT('Ctrl Pts',(-54.8751719199992,-134.619065589833,
174.103985131274));
#37061=CARTESIAN_POINT('Ctrl Pts',(-54.8923243879691,-134.624187050817,
174.076176424152));
#37062=CARTESIAN_POINT('Ctrl Pts',(-54.9117476298381,-134.627553414584,
174.035377192497));
#37063=CARTESIAN_POINT('Ctrl Pts',(-54.9165644905915,-134.628095312931,
174.024149774082));
#37064=CARTESIAN_POINT('Ctrl Pts',(-54.9237322543856,-134.628380622603,
174.005403717575));
#37065=CARTESIAN_POINT('Ctrl Pts',(-54.9263438400637,-134.628342667112,
173.998018814374));
#37066=CARTESIAN_POINT('Ctrl Pts',(-54.9310102965949,-134.627978681951,
173.983658051573));
#37067=CARTESIAN_POINT('Ctrl Pts',(-54.9330918593172,-134.627675390312,
173.976697736202));
#37068=CARTESIAN_POINT('Ctrl Pts',(-54.9374985789908,-134.626677932989,
173.960567138891));
#37069=CARTESIAN_POINT('Ctrl Pts',(-54.9397082867146,-134.625895709395,
173.951370655646));
#37070=CARTESIAN_POINT('Ctrl Pts',(-54.9455958060493,-134.62281760838,173.923002995446));
#37071=CARTESIAN_POINT('Ctrl Pts',(-54.9483167867514,-134.61981278845,173.903727954957));
#37072=CARTESIAN_POINT('Ctrl Pts',(-54.9530722127725,-134.607070202129,
173.841708326837));
#37073=CARTESIAN_POINT('Ctrl Pts',(-54.950166947306,-134.593827283768,173.799907434658));
#37074=CARTESIAN_POINT('Ctrl Pts',(-54.9341914354423,-134.557857646137,
173.720613452297));
#37075=CARTESIAN_POINT('Ctrl Pts',(-54.9213260729919,-134.535552759763,
173.684287229812));
#37076=CARTESIAN_POINT('Ctrl Pts',(-54.8856284528856,-134.475514871886,
173.610631610406));
#37077=CARTESIAN_POINT('Ctrl Pts',(-54.8617778602733,-134.4363002396,173.576836472882));
#37078=CARTESIAN_POINT('Ctrl Pts',(-54.8058488753351,-134.334255725016,
173.512758781142));
#37079=CARTESIAN_POINT('Ctrl Pts',(-54.7725869724248,-134.266384776808,
173.485991595707));
#37080=CARTESIAN_POINT('Ctrl Pts',(-54.7115470800142,-134.100551476174,
173.446390505402));
#37081=CARTESIAN_POINT('Ctrl Pts',(-54.6854625274489,-134.000028948366,
173.435698778786));
#37082=CARTESIAN_POINT('Ctrl Pts',(-54.6738510740226,-133.891110320294,
173.435698778786));
#37083=CARTESIAN_POINT('',(-54.2554511424266,-133.935714548288,175.06991230594));
#37084=CARTESIAN_POINT('Origin',(-61.1562134225954,-133.200047185959,175.985485069079));
#37085=CARTESIAN_POINT('',(-54.1957024747346,-133.942084155439,176.011340061548));
#37086=CARTESIAN_POINT('Ctrl Pts',(-54.1957024747346,-133.942084155439,
176.011340061548));
#37087=CARTESIAN_POINT('Ctrl Pts',(-54.2095773772757,-134.072234559003,
176.011340061548));
#37088=CARTESIAN_POINT('Ctrl Pts',(-54.2483524137813,-134.190499428371,
176.005217214248));
#37089=CARTESIAN_POINT('Ctrl Pts',(-54.3387655134225,-134.368203872713,
175.973983911125));
#37090=CARTESIAN_POINT('Ctrl Pts',(-54.385675185186,-134.434584027699,175.952780802909));
#37091=CARTESIAN_POINT('Ctrl Pts',(-54.4668202456265,-134.528013898444,
175.895826145928));
#37092=CARTESIAN_POINT('Ctrl Pts',(-54.5014199849252,-134.561385029216,
175.865559904196));
#37093=CARTESIAN_POINT('Ctrl Pts',(-54.5586793780035,-134.609882963964,
175.795239818398));
#37094=CARTESIAN_POINT('Ctrl Pts',(-54.581511438678,-134.626662982024,175.75915523611));
#37095=CARTESIAN_POINT('Ctrl Pts',(-54.6122476825661,-134.647095070112,
175.689339128502));
#37096=CARTESIAN_POINT('Ctrl Pts',(-54.6223054576102,-134.652972872761,
175.658386692264));
#37097=CARTESIAN_POINT('Ctrl Pts',(-54.6314720683999,-134.657432661924,
175.614236317853));
#37098=CARTESIAN_POINT('Ctrl Pts',(-54.6334804348868,-134.658273964524,
175.602202640129));
#37099=CARTESIAN_POINT('Ctrl Pts',(-54.6359821836304,-134.659056702573,
175.582302854994));
#37100=CARTESIAN_POINT('Ctrl Pts',(-54.6367612528759,-134.659214105577,
175.57451010894));
#37101=CARTESIAN_POINT('Ctrl Pts',(-54.6378751284851,-134.659228849277,
175.559446946134));
#37102=CARTESIAN_POINT('Ctrl Pts',(-54.63823962848,-134.659108607996,175.552185846972));
#37103=CARTESIAN_POINT('Ctrl Pts',(-54.6386781269537,-134.658534189564,
175.535450016203));
#37104=CARTESIAN_POINT('Ctrl Pts',(-54.6386334884793,-134.657992294335,
175.525975083853));
#37105=CARTESIAN_POINT('Ctrl Pts',(-54.6375918477649,-134.655652888075,
175.496952611561));
#37106=CARTESIAN_POINT('Ctrl Pts',(-54.6356386183457,-134.653146370172,
175.477513935488));
#37107=CARTESIAN_POINT('Ctrl Pts',(-54.6254597431951,-134.64199588013,175.415841584085));
#37108=CARTESIAN_POINT('Ctrl Pts',(-54.6126501450793,-134.629808829799,
175.375610749624));
#37109=CARTESIAN_POINT('Ctrl Pts',(-54.578154091565,-134.595813605642,175.301510044663));
#37110=CARTESIAN_POINT('Ctrl Pts',(-54.5569456018108,-134.574398152378,
175.268735080574));
#37111=CARTESIAN_POINT('Ctrl Pts',(-54.5045621136761,-134.516139089509,
175.204191528638));
#37112=CARTESIAN_POINT('Ctrl Pts',(-54.4732345385129,-134.477721553516,
175.17605924405));
#37113=CARTESIAN_POINT('Ctrl Pts',(-54.4033515332927,-134.37716463072,175.124564042811));
#37114=CARTESIAN_POINT('Ctrl Pts',(-54.3644676987464,-134.309893017983,
175.104768095174));
#37115=CARTESIAN_POINT('Ctrl Pts',(-54.2952498759444,-134.144931539363,
175.076636227182));
#37116=CARTESIAN_POINT('Ctrl Pts',(-54.2670625958527,-134.044633176358,
175.06991230594));
#37117=CARTESIAN_POINT('Ctrl Pts',(-54.2554511424266,-133.935714548288,
175.06991230594));
#37118=CARTESIAN_POINT('',(-54.2380984313038,-133.937564463225,176.757335594116));
#37119=CARTESIAN_POINT('Origin',(-61.1562134225954,-133.200047185959,175.985485069079));
#37120=CARTESIAN_POINT('',(-54.404114913804,-133.919865997052,177.685786985438));
#37121=CARTESIAN_POINT('Ctrl Pts',(-54.404114913804,-133.919865997052,177.685786985438));
#37122=CARTESIAN_POINT('Ctrl Pts',(-54.4179898163449,-134.050016400615,
177.685786985438));
#37123=CARTESIAN_POINT('Ctrl Pts',(-54.454555988691,-134.16851674966,177.673615117958));
#37124=CARTESIAN_POINT('Ctrl Pts',(-54.5354831742812,-134.347232455816,
177.626282208097));
#37125=CARTESIAN_POINT('Ctrl Pts',(-54.5762027302419,-134.414272518502,
177.596216249999));
#37126=CARTESIAN_POINT('Ctrl Pts',(-54.6417491913354,-134.50936530415,177.523976938756));
#37127=CARTESIAN_POINT('Ctrl Pts',(-54.6682546644619,-134.543599337773,
177.487203163407));
#37128=CARTESIAN_POINT('Ctrl Pts',(-54.7072835727268,-134.594040763998,
177.406530931027));
#37129=CARTESIAN_POINT('Ctrl Pts',(-54.7209240792575,-134.611800663137,
177.366487309265));
#37130=CARTESIAN_POINT('Ctrl Pts',(-54.7342258571274,-134.634091381781,
177.291904051349));
#37131=CARTESIAN_POINT('Ctrl Pts',(-54.7366469935942,-134.640783301122,
177.259606729083));
#37132=CARTESIAN_POINT('Ctrl Pts',(-54.7350575501788,-134.646389757523,
177.214671071197));
#37133=CARTESIAN_POINT('Ctrl Pts',(-54.7341471688373,-134.647542218141,
177.202530487771));
#37134=CARTESIAN_POINT('Ctrl Pts',(-54.7318439388331,-134.648837199026,
177.18263347719));
#37135=CARTESIAN_POINT('Ctrl Pts',(-54.7307466880059,-134.649194630286,
177.174885774357));
#37136=CARTESIAN_POINT('Ctrl Pts',(-54.728244066049,-134.649594916787,177.159995627815));
#37137=CARTESIAN_POINT('Ctrl Pts',(-54.7268698213509,-134.649660037307,
177.152855733553));
#37138=CARTESIAN_POINT('Ctrl Pts',(-54.7233113821865,-134.64951171913,177.136487294976));
#37139=CARTESIAN_POINT('Ctrl Pts',(-54.721011642953,-134.649210232709,177.127284562151));
#37140=CARTESIAN_POINT('Ctrl Pts',(-54.7130863671627,-134.647604667936,
177.099293958364));
#37141=CARTESIAN_POINT('Ctrl Pts',(-54.7065558117654,-134.645586123563,
177.080821351903));
#37142=CARTESIAN_POINT('Ctrl Pts',(-54.6819592395746,-134.635972656349,
177.023080450112));
#37143=CARTESIAN_POINT('Ctrl Pts',(-54.659906733014,-134.624770961809,176.986757743235));
#37144=CARTESIAN_POINT('Ctrl Pts',(-54.6086641410077,-134.592561030537,
176.922156779301));
#37145=CARTESIAN_POINT('Ctrl Pts',(-54.5802000432173,-134.571919073564,
176.894837835389));
#37146=CARTESIAN_POINT('Ctrl Pts',(-54.5137839215791,-134.515155983177,
176.843157387555));
#37147=CARTESIAN_POINT('Ctrl Pts',(-54.4765442048596,-134.477368720972,
176.822322902026));
#37148=CARTESIAN_POINT('Ctrl Pts',(-54.3961068783355,-134.377936959341,
176.786402905207));
#37149=CARTESIAN_POINT('Ctrl Pts',(-54.3534234014711,-134.311070413862,
176.774728663888));
#37150=CARTESIAN_POINT('Ctrl Pts',(-54.2789945832238,-134.146664462167,
176.759700940123));
#37151=CARTESIAN_POINT('Ctrl Pts',(-54.2497098847298,-134.046483091295,
176.757335594116));
#37152=CARTESIAN_POINT('Ctrl Pts',(-54.2380984313037,-133.937564463225,
176.757335594116));
#37153=CARTESIAN_POINT('',(-54.62280141715,-133.896552554774,178.399901735339));
#37154=CARTESIAN_POINT('Origin',(-61.1562134225954,-133.200047185959,175.985485069079));
#37155=CARTESIAN_POINT('',(-55.0049347753249,-133.8558145858,179.261418542296));
#37156=CARTESIAN_POINT('Ctrl Pts',(-55.0049347753249,-133.8558145858,179.261418542296));
#37157=CARTESIAN_POINT('Ctrl Pts',(-55.0188096778659,-133.985964989364,
179.261418542296));
#37158=CARTESIAN_POINT('Ctrl Pts',(-55.0517917030077,-134.104847432446,
179.243905039331));
#37159=CARTESIAN_POINT('Ctrl Pts',(-55.119677439025,-134.284953444254,179.183223339405));
#37160=CARTESIAN_POINT('Ctrl Pts',(-55.1522776847934,-134.352859079651,
179.146041855624));
#37161=CARTESIAN_POINT('Ctrl Pts',(-55.1990415665339,-134.449954213742,
179.062716176308));
#37162=CARTESIAN_POINT('Ctrl Pts',(-55.2161393983533,-134.48519116478,179.021572025499));
#37163=CARTESIAN_POINT('Ctrl Pts',(-55.2350040948343,-134.537782230696,
178.935236023451));
#37164=CARTESIAN_POINT('Ctrl Pts',(-55.2387780153924,-134.556593973818,
178.89356055196));
#37165=CARTESIAN_POINT('Ctrl Pts',(-55.2340175155502,-134.580810251938,
178.818544651587));
#37166=CARTESIAN_POINT('Ctrl Pts',(-55.2287038814645,-134.588326749495,
178.786779446265));
#37167=CARTESIAN_POINT('Ctrl Pts',(-55.2164840634913,-134.595066474844,
178.743670002006));
#37168=CARTESIAN_POINT('Ctrl Pts',(-55.2127143077742,-134.596523763874,
178.732128079458));
#37169=CARTESIAN_POINT('Ctrl Pts',(-55.2057463832246,-134.598316032362,
178.713390185362));
#37170=CARTESIAN_POINT('Ctrl Pts',(-55.2028380535871,-134.598866536722,
178.706137794079));
#37171=CARTESIAN_POINT('Ctrl Pts',(-55.1968651951133,-134.599636773621,
178.692286024995));
#37172=CARTESIAN_POINT('Ctrl Pts',(-55.193831573278,-134.59987879483,178.685682280334));
#37173=CARTESIAN_POINT('Ctrl Pts',(-55.1864797675247,-134.600134874874,
178.670632508104));
#37174=CARTESIAN_POINT('Ctrl Pts',(-55.1820552312309,-134.600059906015,
178.662236804185));
#37175=CARTESIAN_POINT('Ctrl Pts',(-55.1676918971867,-134.599140681264,
178.636904781052));
#37176=CARTESIAN_POINT('Ctrl Pts',(-55.1569469175024,-134.597571422677,
178.620471804946));
#37177=CARTESIAN_POINT('Ctrl Pts',(-55.1192871565485,-134.589350578658,
178.570018044099));
#37178=CARTESIAN_POINT('Ctrl Pts',(-55.0891903299897,-134.579006462373,
178.539714408502));
#37179=CARTESIAN_POINT('Ctrl Pts',(-55.0239484505953,-134.548288948664,
178.488367558804));
#37180=CARTESIAN_POINT('Ctrl Pts',(-54.9897379336018,-134.52825959837,178.468092312789));
#37181=CARTESIAN_POINT('Ctrl Pts',(-54.9127579386383,-134.472622687455,
178.432278448833));
#37182=CARTESIAN_POINT('Ctrl Pts',(-54.8715145135347,-134.435262247312,
178.419952586932));
#37183=CARTESIAN_POINT('Ctrl Pts',(-54.7845359434711,-134.336527825942,
178.401695334183));
#37184=CARTESIAN_POINT('Ctrl Pts',(-54.7400959350076,-134.269848538465,
178.398821263656));
#37185=CARTESIAN_POINT('Ctrl Pts',(-54.6637259003796,-134.105649533411,
178.397771040799));
#37186=CARTESIAN_POINT('Ctrl Pts',(-54.6344128705762,-134.005471182846,
178.399901735339));
#37187=CARTESIAN_POINT('Ctrl Pts',(-54.62280141715,-133.896552554774,178.399901735339));
#37188=CARTESIAN_POINT('',(-55.3872025607663,-133.815062285981,179.902150755967));
#37189=CARTESIAN_POINT('Origin',(-61.1562134225954,-133.200047185959,175.985485069079));
#37190=CARTESIAN_POINT('',(-55.963244592837,-133.753652356887,180.646664753224));
#37191=CARTESIAN_POINT('Ctrl Pts',(-55.963244592837,-133.753652356887,180.646664753224));
#37192=CARTESIAN_POINT('Ctrl Pts',(-55.9771194953779,-133.88380276045,180.646664753224));
#37193=CARTESIAN_POINT('Ctrl Pts',(-56.0053503878778,-134.003191706013,
180.624827435906));
#37194=CARTESIAN_POINT('Ctrl Pts',(-56.0573970604472,-134.184986267805,
180.554323545746));
#37195=CARTESIAN_POINT('Ctrl Pts',(-56.0804206664297,-134.253912836984,
180.512187388971));
#37196=CARTESIAN_POINT('Ctrl Pts',(-56.1063095640505,-134.353233383846,
180.422617927188));
#37197=CARTESIAN_POINT('Ctrl Pts',(-56.1132331173457,-134.389554980947,
180.379494549411));
#37198=CARTESIAN_POINT('Ctrl Pts',(-56.1111717457673,-134.444376905523,
180.292512312315));
#37199=CARTESIAN_POINT('Ctrl Pts',(-56.104977458637,-134.464251326181,180.251627018014));
#37200=CARTESIAN_POINT('Ctrl Pts',(-56.0825765833158,-134.490348186181,
180.180538126642));
#37201=CARTESIAN_POINT('Ctrl Pts',(-56.0698795634517,-134.498651801989,
180.151151116536));
#37202=CARTESIAN_POINT('Ctrl Pts',(-56.0477728492981,-134.506445536525,
180.112373250109));
#37203=CARTESIAN_POINT('Ctrl Pts',(-56.0413692691035,-134.50818360884,180.102100763024));
#37204=CARTESIAN_POINT('Ctrl Pts',(-56.0301480293029,-134.51042930915,180.085610963709));
#37205=CARTESIAN_POINT('Ctrl Pts',(-56.0255991154346,-134.51115471075,180.079275366594));
#37206=CARTESIAN_POINT('Ctrl Pts',(-56.0165039590249,-134.512257805468,
180.067266989438));
#37207=CARTESIAN_POINT('Ctrl Pts',(-56.0119867645754,-134.512657985429,
180.061583180014));
#37208=CARTESIAN_POINT('Ctrl Pts',(-56.0012656199609,-134.513273259507,
180.04872671219));
#37209=CARTESIAN_POINT('Ctrl Pts',(-55.9949700757869,-134.513397752587,
180.04162596497));
#37210=CARTESIAN_POINT('Ctrl Pts',(-55.9749884168559,-134.513077478804,
180.020424727599));
#37211=CARTESIAN_POINT('Ctrl Pts',(-55.9606368415963,-134.511892707401,
180.006986406688));
#37212=CARTESIAN_POINT('Ctrl Pts',(-55.9120275852045,-134.504839152748,
179.966751975973));
#37213=CARTESIAN_POINT('Ctrl Pts',(-55.8755525337326,-134.495174997851,
179.944228548807));
#37214=CARTESIAN_POINT('Ctrl Pts',(-55.7998722057521,-134.4655702925,179.909119905611));
#37215=CARTESIAN_POINT('Ctrl Pts',(-55.7617584193857,-134.445957056798,
179.897066681094));
#37216=CARTESIAN_POINT('Ctrl Pts',(-55.6782972451937,-134.391011082889,
179.879200772612));
#37217=CARTESIAN_POINT('Ctrl Pts',(-55.6351912258566,-134.353849207735,
179.876099868631));
#37218=CARTESIAN_POINT('Ctrl Pts',(-55.5460646433215,-134.255343778846,
179.876566405119));
#37219=CARTESIAN_POINT('Ctrl Pts',(-55.5020132972087,-134.188623057366,
179.882659535915));
#37220=CARTESIAN_POINT('Ctrl Pts',(-55.4270846416986,-134.024270391666,
179.895647849101));
#37221=CARTESIAN_POINT('Ctrl Pts',(-55.3988140141925,-133.923980914052,
179.902150755967));
#37222=CARTESIAN_POINT('Ctrl Pts',(-55.3872025607663,-133.815062285981,
179.902150755967));
#37223=CARTESIAN_POINT('',(-56.4868776461708,-133.697829575064,181.176777403373));
#37224=CARTESIAN_POINT('Origin',(-61.1562134225954,-133.200047185959,175.985485069079));
#37225=CARTESIAN_POINT('',(-57.223350883061,-133.619316607712,181.761020143608));
#37226=CARTESIAN_POINT('Ctrl Pts',(-57.223350883061,-133.619316607712,181.761020143608));
#37227=CARTESIAN_POINT('Ctrl Pts',(-57.237225785602,-133.749467011276,181.761020143608));
#37228=CARTESIAN_POINT('Ctrl Pts',(-57.2598146785821,-133.869457431682,
181.736128117445));
#37229=CARTESIAN_POINT('Ctrl Pts',(-57.294145182622,-134.053140655397,181.659899466876));
#37230=CARTESIAN_POINT('Ctrl Pts',(-57.3066913787201,-134.123184186468,
181.61525743738));
#37231=CARTESIAN_POINT('Ctrl Pts',(-57.3108260656547,-134.224823877527,
181.524649644676));
#37232=CARTESIAN_POINT('Ctrl Pts',(-57.3073999952942,-134.262248813655,
181.4820532139));
#37233=CARTESIAN_POINT('Ctrl Pts',(-57.2848668463936,-134.319253166463,
181.39947983321));
#37234=CARTESIAN_POINT('Ctrl Pts',(-57.269182045857,-134.340139339255,181.361760820791));
#37235=CARTESIAN_POINT('Ctrl Pts',(-57.2305878917923,-134.367962510955,
181.298730366389));
#37236=CARTESIAN_POINT('Ctrl Pts',(-57.2112879664683,-134.376970040598,
181.27342941771));
#37237=CARTESIAN_POINT('Ctrl Pts',(-57.1806124249801,-134.385677269376,
181.241236757758));
#37238=CARTESIAN_POINT('Ctrl Pts',(-57.171953638511,-134.387655761746,181.232830705747));
#37239=CARTESIAN_POINT('Ctrl Pts',(-57.1571376499742,-134.390284686288,
181.21954732841));
#37240=CARTESIAN_POINT('Ctrl Pts',(-57.1512139912475,-134.391156644874,
181.214496727339));
#37241=CARTESIAN_POINT('Ctrl Pts',(-57.1395259320919,-134.392536160348,
181.205029625343));
#37242=CARTESIAN_POINT('Ctrl Pts',(-57.1337871894003,-134.393066565513,
181.200596073502));
#37243=CARTESIAN_POINT('Ctrl Pts',(-57.1203165473769,-134.393974954383,
181.19068008126));
#37244=CARTESIAN_POINT('Ctrl Pts',(-57.1125125206794,-134.394260261779,
181.185286960358));
#37245=CARTESIAN_POINT('Ctrl Pts',(-57.0880587868503,-134.394416741058,
181.169448647602));
#37246=CARTESIAN_POINT('Ctrl Pts',(-57.0709180469526,-134.393529313238,
181.15978596825));
#37247=CARTESIAN_POINT('Ctrl Pts',(-57.0141093333233,-134.387349875507,
181.132109146535));
#37248=CARTESIAN_POINT('Ctrl Pts',(-56.9732928312716,-134.378148548247,
181.118674907517));
#37249=CARTESIAN_POINT('Ctrl Pts',(-56.8913415381959,-134.34921236967,181.101844857552));
#37250=CARTESIAN_POINT('Ctrl Pts',(-56.8513944761148,-134.329794573407,
181.098714144129));
#37251=CARTESIAN_POINT('Ctrl Pts',(-56.7659114793704,-134.27506413929,181.099834492783));
#37252=CARTESIAN_POINT('Ctrl Pts',(-56.7231922271569,-134.237861032177,
181.106138759988));
#37253=CARTESIAN_POINT('Ctrl Pts',(-56.6364356978932,-134.139102939774,
181.12530197231));
#37254=CARTESIAN_POINT('Ctrl Pts',(-56.5948956204382,-134.072114500278,
181.140008193814));
#37255=CARTESIAN_POINT('Ctrl Pts',(-56.5247071718325,-133.907256496853,
181.166280209492));
#37256=CARTESIAN_POINT('Ctrl Pts',(-56.498489099597,-133.806748203135,181.176777403373));
#37257=CARTESIAN_POINT('Ctrl Pts',(-56.4868776461708,-133.697829575064,
181.176777403373));
#37258=CARTESIAN_POINT('Origin',(-61.1562134225954,-133.200047185959,175.985485069079));
#37259=CARTESIAN_POINT('Origin',(-61.1562134225954,-133.200047185959,175.985485069079));
#37260=CARTESIAN_POINT('Origin',(-61.1562134225954,-133.200047185959,175.985485069079));
#37261=CARTESIAN_POINT('Origin',(-61.1562134225954,-133.200047185959,175.985485069079));
#37262=CARTESIAN_POINT('Origin',(-61.1562134225954,-133.200047185959,175.985485069079));
#37263=CARTESIAN_POINT('Origin',(-61.1562134225954,-133.200047185959,175.985485069079));
#37264=CARTESIAN_POINT('Origin',(-54.1598171290174,-67.5719248685924,175.985485069079));
#37265=CARTESIAN_POINT('Ctrl Pts',(-52.354402310021,-68.0158107614237,173.617797875547));
#37266=CARTESIAN_POINT('Ctrl Pts',(-52.3922609029376,-68.008076981393,173.587868187509));
#37267=CARTESIAN_POINT('Ctrl Pts',(-52.4308701851704,-68.0002229772944,
173.558852597356));
#37268=CARTESIAN_POINT('Ctrl Pts',(-52.7925027578306,-67.926959058679,173.300747567891));
#37269=CARTESIAN_POINT('Ctrl Pts',(-53.1570390226867,-67.855260286434,173.138568265546));
#37270=CARTESIAN_POINT('Ctrl Pts',(-53.8341366603134,-67.7254283072159,
172.989462193406));
#37271=CARTESIAN_POINT('Ctrl Pts',(-54.1340786807895,-67.6689480666864,
172.970420115031));
#37272=CARTESIAN_POINT('Ctrl Pts',(-54.727201252603,-67.5592649898145,173.023972702883));
#37273=CARTESIAN_POINT('Ctrl Pts',(-55.0168740057393,-67.5050562916733,
173.095494376926));
#37274=CARTESIAN_POINT('Ctrl Pts',(-55.2910412295907,-67.4513288218826,
173.209554841606));
#37275=CARTESIAN_POINT('Origin',(-54.1598171290174,-67.5719248685924,175.985485069079));
#37276=CARTESIAN_POINT('Origin',(-54.1598171290174,-67.5719248685924,175.985485069079));
#37277=CARTESIAN_POINT('',(-67.2656014102483,-128.526079858515,173.57106840282));
#37278=CARTESIAN_POINT('Origin',(-54.1598171290174,-67.5719248685924,175.985485069079));
#37279=CARTESIAN_POINT('Origin',(-54.1598171290174,-67.5719248685924,175.985485069079));
#37280=CARTESIAN_POINT('Origin',(-54.1598171290174,-67.5719248685924,175.985485069079));
#37281=CARTESIAN_POINT('Origin',(-54.1598171290174,-67.5719248685924,175.985485069079));
#37282=CARTESIAN_POINT('Origin',(-54.1598171290174,-67.5719248685924,175.985485069079));
#37283=CARTESIAN_POINT('Origin',(-54.1598171290174,-67.5719248685924,175.985485069079));
#37284=CARTESIAN_POINT('Origin',(-54.1598171290174,-67.5719248685924,175.985485069079));
#37285=CARTESIAN_POINT('Origin',(-54.1598171290174,-67.5719248685924,175.985485069079));
#37286=CARTESIAN_POINT('Origin',(-54.1598171290174,-67.5719248685924,175.985485069079));
#37287=CARTESIAN_POINT('',(-56.7993268652684,-129.641854649084,181.761020143608));
#37288=CARTESIAN_POINT('Origin',(-54.1598171290174,-67.5719248685924,175.985485069079));
#37289=CARTESIAN_POINT('',(-56.0628536283782,-129.720367616436,181.176777403373));
#37290=CARTESIAN_POINT('',(-55.5392205750444,-129.776190398259,180.646664753224));
#37291=CARTESIAN_POINT('Origin',(-54.1598171290174,-67.5719248685924,175.985485069079));
#37292=CARTESIAN_POINT('',(-54.9631785429737,-129.837600327353,179.902150755967));
#37293=CARTESIAN_POINT('',(-54.5809107575323,-129.878352627172,179.261418542296));
#37294=CARTESIAN_POINT('Origin',(-54.1598171290174,-67.5719248685924,175.985485069079));
#37295=CARTESIAN_POINT('',(-54.1987773993573,-129.919090596146,178.399901735339));
#37296=CARTESIAN_POINT('',(-53.9800908960114,-129.942404038424,177.685786985438));
#37297=CARTESIAN_POINT('Origin',(-54.1598171290174,-67.5719248685924,175.985485069079));
#37298=CARTESIAN_POINT('',(-53.8140744135111,-129.960102504597,176.757335594116));
#37299=CARTESIAN_POINT('',(-53.771678456942,-129.96462219681,176.011340061548));
#37300=CARTESIAN_POINT('Origin',(-54.1598171290174,-67.5719248685924,175.985485069079));
#37301=CARTESIAN_POINT('',(-53.831427124634,-129.95825258966,175.06991230594));
#37302=CARTESIAN_POINT('',(-53.9677856137344,-129.943715863725,174.335390539474));
#37303=CARTESIAN_POINT('Origin',(-54.1598171290174,-67.5719248685924,175.985485069079));
#37304=CARTESIAN_POINT('',(-54.2498270562299,-129.913648361666,173.435698778786));
#37305=CARTESIAN_POINT('',(-54.5570153312564,-129.880900039256,172.755338513612));
#37306=CARTESIAN_POINT('Origin',(-54.1598171290174,-67.5719248685924,175.985485069079));
#37307=CARTESIAN_POINT('',(-55.0449583250965,-129.828882056217,171.949669562728));
#37308=CARTESIAN_POINT('',(-55.5051237200884,-129.779825350794,171.363010864448));
#37309=CARTESIAN_POINT('Origin',(-54.1598171290174,-67.5719248685924,175.985485069079));
#37310=CARTESIAN_POINT('',(-56.1706107920718,-129.708879982872,170.698187274307));
#37311=CARTESIAN_POINT('',(-56.7570101669053,-129.646365891843,170.239324614047));
#37312=CARTESIAN_POINT('Origin',(-54.1598171290174,-67.5719248685924,175.985485069079));
#37313=CARTESIAN_POINT('',(-57.5613656273554,-129.560616225945,169.753983515172));
#37314=CARTESIAN_POINT('',(-58.2399195818402,-129.48827784105,169.44958432285));
#37315=CARTESIAN_POINT('Origin',(-54.1598171290174,-67.5719248685924,175.985485069079));
#37316=CARTESIAN_POINT('',(-59.1363972151087,-129.392707336071,169.171931975764));
#37317=CARTESIAN_POINT('',(-59.8676706598535,-129.3147487013,169.03968682599));
#37318=CARTESIAN_POINT('Origin',(-54.1598171290174,-67.5719248685924,175.985485069079));
#37319=CARTESIAN_POINT('',(-60.8041704444585,-129.214911567606,168.985859375881));
#37320=CARTESIAN_POINT('',(-61.5456644249254,-129.135863355445,169.03345387607));
#37321=CARTESIAN_POINT('Origin',(-54.1598171290174,-67.5719248685924,175.985485069079));
#37322=CARTESIAN_POINT('',(-62.4677603974239,-129.037561764351,169.206579578684));
#37323=CARTESIAN_POINT('',(-63.1763819786892,-128.962017969562,169.431247709482));
#37324=CARTESIAN_POINT('Origin',(-54.1598171290174,-67.5719248685924,175.985485069079));
#37325=CARTESIAN_POINT('',(-64.030485272842,-128.870964852232,169.821265128268));
#37326=CARTESIAN_POINT('',(-64.6650519443373,-128.803315805577,170.209949994551));
#37327=CARTESIAN_POINT('Origin',(-54.1598171290174,-67.5719248685924,175.985485069079));
#37328=CARTESIAN_POINT('',(-65.4015251812274,-128.724802838225,170.794192734786));
#37329=CARTESIAN_POINT('',(-65.9251582345612,-128.668980056403,171.324305384935));
#37330=CARTESIAN_POINT('Origin',(-64.79464880995,-126.778167037988,181.510088520653));
#37331=CARTESIAN_POINT('',(-59.0118785952597,-127.394648976958,179.686725372425));
#37332=CARTESIAN_POINT('',(-64.4583706077394,-126.814016540979,175.424797521489));
#37333=CARTESIAN_POINT('Ctrl Pts',(-59.0118785952585,-127.39464897695,179.686725372426));
#37334=CARTESIAN_POINT('Ctrl Pts',(-59.4359949842293,-127.349435336409,
179.865346446743));
#37335=CARTESIAN_POINT('Ctrl Pts',(-59.8876448219349,-127.301286446285,
179.967826141208));
#37336=CARTESIAN_POINT('Ctrl Pts',(-60.7960132539299,-127.204448302721,
180.012144456981));
#37337=CARTESIAN_POINT('Ctrl Pts',(-61.2457410607842,-127.156504313926,
179.956996941234));
#37338=CARTESIAN_POINT('Ctrl Pts',(-62.1463022559178,-127.060498473971,
179.685447946453));
#37339=CARTESIAN_POINT('Ctrl Pts',(-62.5856624257918,-127.013659744544,
179.457395568183));
#37340=CARTESIAN_POINT('Ctrl Pts',(-63.3595262690438,-126.931160688751,
178.851724556864));
#37341=CARTESIAN_POINT('Ctrl Pts',(-63.6872391011354,-126.896224311435,
178.479429252066));
#37342=CARTESIAN_POINT('Ctrl Pts',(-64.1700987222909,-126.844748249885,
177.668306113048));
#37343=CARTESIAN_POINT('Ctrl Pts',(-64.3336854609466,-126.827308810639,
177.243537880892));
#37344=CARTESIAN_POINT('Ctrl Pts',(-64.5140884934819,-126.808076642117,
176.347356701111));
#37345=CARTESIAN_POINT('Ctrl Pts',(-64.5262870428016,-126.806776195262,
175.882015335093));
#37346=CARTESIAN_POINT('Ctrl Pts',(-64.4583706077402,-126.814016540982,
175.424797521489));
#37347=CARTESIAN_POINT('Ctrl Pts',(-64.4583706077523,-126.814016540981,
175.424797521484));
#37348=CARTESIAN_POINT('Ctrl Pts',(-64.340455120303,-126.826587119724,175.127034144718));
#37349=CARTESIAN_POINT('Ctrl Pts',(-64.185525566722,-126.843103645204,174.845600608932));
#37350=CARTESIAN_POINT('Ctrl Pts',(-63.8142461467475,-126.882684511852,
174.337218287797));
#37351=CARTESIAN_POINT('Ctrl Pts',(-63.6016307872636,-126.905350729633,
174.111030744869));
#37352=CARTESIAN_POINT('Ctrl Pts',(-63.1867614231896,-126.949578575542,
173.767005019069));
#37353=CARTESIAN_POINT('Ctrl Pts',(-62.9060963946901,-126.979499342674,
173.561578827361));
#37354=CARTESIAN_POINT('Ctrl Pts',(-62.237164000988,-127.050812004909,173.298981894668));
#37355=CARTESIAN_POINT('Ctrl Pts',(-61.9468760301073,-127.081758641988,
173.232074662412));
#37356=CARTESIAN_POINT('Ctrl Pts',(-61.6514014972809,-127.113258201221,
173.209554841667));
#37357=CARTESIAN_POINT('Ctrl Pts',(-57.5665324870373,-127.548732528291,
176.406000729816));
#37358=CARTESIAN_POINT('Ctrl Pts',(-57.5156929015415,-127.554152367759,
176.69915760637));
#37359=CARTESIAN_POINT('Ctrl Pts',(-57.5087873657294,-127.554888544012,
176.998153402395));
#37360=CARTESIAN_POINT('Ctrl Pts',(-57.5972658161105,-127.545456150086,
177.715327713047));
#37361=CARTESIAN_POINT('Ctrl Pts',(-57.7265253129934,-127.531676224149,
178.039347906201));
#37362=CARTESIAN_POINT('Ctrl Pts',(-57.9549266303152,-127.507327117798,
178.526645640705));
#37363=CARTESIAN_POINT('Ctrl Pts',(-58.1207929492895,-127.48964466006,178.789993473182));
#37364=CARTESIAN_POINT('Ctrl Pts',(-58.5199743484872,-127.447089256016,
179.277750850868));
#37365=CARTESIAN_POINT('Ctrl Pts',(-58.7534704118167,-127.422197015703,
179.498319550967));
#37366=CARTESIAN_POINT('Ctrl Pts',(-59.0118785952414,-127.394648976952,
179.686725372449));
#37367=CARTESIAN_POINT('Origin',(-61.2622194270436,-134.194412675616,175.985485069079));
#37368=CARTESIAN_POINT('Origin',(-54.1598171290174,-67.5719248685924,175.985485069079));
#37369=CARTESIAN_POINT('',(-66.8834680520733,-128.566817827489,172.709551595863));
#37370=CARTESIAN_POINT('',(-66.5012002666319,-128.607570127308,172.068819382192));
#37371=CARTESIAN_POINT('Origin',(-55.9917334493218,-67.3766303500087,178.353172262611));
#37372=CARTESIAN_POINT('',(-52.6515183282542,-67.7327195975386,179.686725372378));
#37373=CARTESIAN_POINT('Ctrl Pts',(-51.2061722201485,-67.8868031488672,
176.406000729815));
#37374=CARTESIAN_POINT('Ctrl Pts',(-51.1553326346522,-67.892222988335,176.699157606371));
#37375=CARTESIAN_POINT('Ctrl Pts',(-51.1484270988405,-67.8929591645877,
176.998153402397));
#37376=CARTESIAN_POINT('Ctrl Pts',(-51.2369055492213,-67.8835267706619,
177.715327713046));
#37377=CARTESIAN_POINT('Ctrl Pts',(-51.3661650461041,-67.8697468447252,
178.0393479062));
#37378=CARTESIAN_POINT('Ctrl Pts',(-51.5945663634263,-67.8453977383736,
178.526645640706));
#37379=CARTESIAN_POINT('Ctrl Pts',(-51.760432682401,-67.8277152806355,178.789993473183));
#37380=CARTESIAN_POINT('Ctrl Pts',(-52.1596140815011,-67.7851598766027,
179.277750850749));
#37381=CARTESIAN_POINT('Ctrl Pts',(-52.3931101446833,-67.760267636305,179.498319550776));
#37382=CARTESIAN_POINT('Ctrl Pts',(-52.6515183282542,-67.7327195975386,
179.686725372378));
#37383=CARTESIAN_POINT('',(-58.0980103408427,-67.1520871615593,175.424797521432));
#37384=CARTESIAN_POINT('Ctrl Pts',(-58.0980103408427,-67.1520871615593,
175.424797521432));
#37385=CARTESIAN_POINT('Ctrl Pts',(-57.9800948533587,-67.164657740306,175.127034144591));
#37386=CARTESIAN_POINT('Ctrl Pts',(-57.8251652997951,-67.1811742657839,
174.845600608881));
#37387=CARTESIAN_POINT('Ctrl Pts',(-57.4538858798669,-67.2207551324268,
174.337218287807));
#37388=CARTESIAN_POINT('Ctrl Pts',(-57.2412705203865,-67.2434213502081,
174.111030744881));
#37389=CARTESIAN_POINT('Ctrl Pts',(-56.8264011563053,-67.2876491961175,
173.767005019072));
#37390=CARTESIAN_POINT('Ctrl Pts',(-56.5457361278046,-67.3175699632491,
173.561578827364));
#37391=CARTESIAN_POINT('Ctrl Pts',(-55.8768037354484,-67.3888826253409,
173.298981895197));
#37392=CARTESIAN_POINT('Ctrl Pts',(-55.5865157635609,-67.4198292625273,
173.232074662357));
#37393=CARTESIAN_POINT('Ctrl Pts',(-55.29104122959,-67.4513288218827,173.209554841606));
#37394=CARTESIAN_POINT('Ctrl Pts',(-52.6515183282542,-67.7327195975386,
179.686725372378));
#37395=CARTESIAN_POINT('Ctrl Pts',(-53.0762789282691,-67.6874372797963,
179.865617762962));
#37396=CARTESIAN_POINT('Ctrl Pts',(-53.5286545057955,-67.6392110209586,
179.968135041463));
#37397=CARTESIAN_POINT('Ctrl Pts',(-54.4383742439024,-67.542228819135,180.012039202549));
#37398=CARTESIAN_POINT('Ctrl Pts',(-54.8887059634283,-67.4942204492149,
179.956466658887));
#37399=CARTESIAN_POINT('Ctrl Pts',(-55.7899722900454,-67.3981394375324,
179.68371381595));
#37400=CARTESIAN_POINT('Ctrl Pts',(-56.2294231124242,-67.3512910439425,
179.454971033449));
#37401=CARTESIAN_POINT('Ctrl Pts',(-57.0028982092043,-67.2688334311204,
178.847994825624));
#37402=CARTESIAN_POINT('Ctrl Pts',(-57.3301960056921,-67.2339412993728,
178.475171130105));
#37403=CARTESIAN_POINT('Ctrl Pts',(-57.8115564772304,-67.1826250571884,
177.664035140268));
#37404=CARTESIAN_POINT('Ctrl Pts',(-57.9743790814683,-67.165267079776,177.239932149216));
#37405=CARTESIAN_POINT('Ctrl Pts',(-58.153780989458,-67.1461416378191,176.345419634447));
#37406=CARTESIAN_POINT('Ctrl Pts',(-58.1657851525024,-67.1448619138401,
175.881061917132));
#37407=CARTESIAN_POINT('Ctrl Pts',(-58.0980103408427,-67.1520871615593,
175.424797521432));
#37408=CARTESIAN_POINT('Ctrl Pts',(-51.0870509156302,-66.8309817211475,
175.613978373734));
#37409=CARTESIAN_POINT('Ctrl Pts',(-50.9439729228075,-66.9405160196288,
176.847054148052));
#37410=CARTESIAN_POINT('Ctrl Pts',(-51.7127157157354,-66.9528441305708,
177.8277821816));
#37411=CARTESIAN_POINT('Ctrl Pts',(-52.4814585086634,-66.9651722415128,
178.808510215148));
#37412=CARTESIAN_POINT('Ctrl Pts',(-53.7175245676945,-66.9276805701509,
178.962393326872));
#37413=CARTESIAN_POINT('Ctrl Pts',(-54.9535906267256,-66.890188898789,179.116276438596));
#37414=CARTESIAN_POINT('Ctrl Pts',(-55.9387308009417,-66.8794476031576,
178.35317198867));
#37415=CARTESIAN_POINT('Ctrl Pts',(-56.9238709751577,-66.8687063075263,
177.590067538743));
#37416=CARTESIAN_POINT('Ctrl Pts',(-57.0868250938145,-66.9456155383557,
176.356991764425));
#37417=CARTESIAN_POINT('Ctrl Pts',(-57.2497792124713,-67.0225247691851,
175.123915990107));
#37418=CARTESIAN_POINT('Ctrl Pts',(-56.5009125453774,-67.1966401875538,
174.143187956559));
#37419=CARTESIAN_POINT('Ctrl Pts',(-55.7520458782835,-67.3707556059225,
173.162459923011));
#37420=CARTESIAN_POINT('Ctrl Pts',(-54.5358559450863,-67.5946908065951,
173.008576811287));
#37421=CARTESIAN_POINT('Ctrl Pts',(-53.3196660118892,-67.8186260072677,
172.854693699562));
#37422=CARTESIAN_POINT('Ctrl Pts',(-52.3544019635072,-68.0158108322098,
173.617798149489));
#37423=CARTESIAN_POINT('Ctrl Pts',(-51.3891379151252,-68.2129956571518,
174.380902599416));
#37424=CARTESIAN_POINT('Ctrl Pts',(-51.2460599223025,-68.3225299556331,
175.613978373734));
#37425=CARTESIAN_POINT('Ctrl Pts',(-51.1029819294797,-68.4320642541144,
176.847054148052));
#37426=CARTESIAN_POINT('Ctrl Pts',(-51.8717247224076,-68.4443923650564,
177.8277821816));
#37427=CARTESIAN_POINT('Ctrl Pts',(-52.6404675153356,-68.4567204759984,
178.808510215148));
#37428=CARTESIAN_POINT('Ctrl Pts',(-53.8765335743667,-68.4192288046365,
178.962393326872));
#37429=CARTESIAN_POINT('Ctrl Pts',(-55.1125996333979,-68.3817371332746,
179.116276438596));
#37430=CARTESIAN_POINT('Ctrl Pts',(-56.0977398076139,-68.3709958376432,
178.35317198867));
#37431=CARTESIAN_POINT('Ctrl Pts',(-57.0828799818299,-68.3602545420119,
177.590067538743));
#37432=CARTESIAN_POINT('Ctrl Pts',(-57.2458341004867,-68.4371637728413,
176.356991764425));
#37433=CARTESIAN_POINT('Ctrl Pts',(-57.4087882191435,-68.5140730036707,
175.123915990107));
#37434=CARTESIAN_POINT('Ctrl Pts',(-56.6599215520496,-68.6881884220394,
174.143187956559));
#37435=CARTESIAN_POINT('Ctrl Pts',(-55.9110548849557,-68.8623038404081,
173.162459923011));
#37436=CARTESIAN_POINT('Ctrl Pts',(-54.6948649517586,-69.0862390410807,
173.008576811287));
#37437=CARTESIAN_POINT('Ctrl Pts',(-53.4786750185615,-69.3101742417533,
172.854693699562));
#37438=CARTESIAN_POINT('Ctrl Pts',(-52.5134109701795,-69.5073590666954,
173.617798149489));
#37439=CARTESIAN_POINT('Ctrl Pts',(-51.5481469217975,-69.7045438916374,
174.380902599416));
#37440=CARTESIAN_POINT('Ctrl Pts',(-51.4050689289747,-69.8140781901187,
175.613978373734));
#37441=CARTESIAN_POINT('Ctrl Pts',(-51.2619909361519,-69.9236124886,176.847054148052));
#37442=CARTESIAN_POINT('Ctrl Pts',(-52.0307337290798,-69.935940599542,177.8277821816));
#37443=CARTESIAN_POINT('Ctrl Pts',(-52.7994765220078,-69.948268710484,178.808510215148));
#37444=CARTESIAN_POINT('Ctrl Pts',(-54.035542581039,-69.9107770391221,178.962393326872));
#37445=CARTESIAN_POINT('Ctrl Pts',(-55.2716086400701,-69.8732853677602,
179.116276438596));
#37446=CARTESIAN_POINT('Ctrl Pts',(-56.2567488142861,-69.8625440721288,
178.35317198867));
#37447=CARTESIAN_POINT('Ctrl Pts',(-57.2418889885021,-69.8518027764975,
177.590067538743));
#37448=CARTESIAN_POINT('Ctrl Pts',(-57.404843107159,-69.9287120073269,176.356991764425));
#37449=CARTESIAN_POINT('Ctrl Pts',(-57.5677972258158,-70.0056212381563,
175.123915990107));
#37450=CARTESIAN_POINT('Ctrl Pts',(-56.8189305587218,-70.179736656525,174.143187956559));
#37451=CARTESIAN_POINT('Ctrl Pts',(-56.0700638916279,-70.3538520748937,
173.162459923011));
#37452=CARTESIAN_POINT('Ctrl Pts',(-54.8538739584308,-70.5777872755663,
173.008576811287));
#37453=CARTESIAN_POINT('Ctrl Pts',(-53.6376840252337,-70.801722476239,172.854693699562));
#37454=CARTESIAN_POINT('Ctrl Pts',(-52.6724199768517,-70.998907301181,173.617798149489));
#37455=CARTESIAN_POINT('Ctrl Pts',(-51.7071559284697,-71.196092126123,174.380902599416));
#37456=CARTESIAN_POINT('Ctrl Pts',(-51.5640779356469,-71.3056264246043,
175.613978373734));
#37457=CARTESIAN_POINT('Ctrl Pts',(-51.4209999428241,-71.4151607230856,
176.847054148052));
#37458=CARTESIAN_POINT('Ctrl Pts',(-52.1897427357521,-71.4274888340276,
177.8277821816));
#37459=CARTESIAN_POINT('Ctrl Pts',(-52.95848552868,-71.4398169449696,178.808510215148));
#37460=CARTESIAN_POINT('Ctrl Pts',(-54.1945515877112,-71.4023252736077,
178.962393326872));
#37461=CARTESIAN_POINT('Ctrl Pts',(-55.4306176467423,-71.3648336022458,
179.116276438596));
#37462=CARTESIAN_POINT('Ctrl Pts',(-56.4157578209583,-71.3540923066144,
178.35317198867));
#37463=CARTESIAN_POINT('Ctrl Pts',(-57.4008979951744,-71.3433510109831,
177.590067538743));
#37464=CARTESIAN_POINT('Ctrl Pts',(-57.5638521138312,-71.4202602418125,
176.356991764425));
#37465=CARTESIAN_POINT('Ctrl Pts',(-57.726806232488,-71.4971694726419,175.123915990107));
#37466=CARTESIAN_POINT('Ctrl Pts',(-56.9779395653941,-71.6712848910106,
174.143187956559));
#37467=CARTESIAN_POINT('Ctrl Pts',(-56.2290728983002,-71.8454003093793,
173.162459923011));
#37468=CARTESIAN_POINT('Ctrl Pts',(-55.012882965103,-72.0693355100519,173.008576811287));
#37469=CARTESIAN_POINT('Ctrl Pts',(-53.7966930319059,-72.2932707107245,
172.854693699562));
#37470=CARTESIAN_POINT('Ctrl Pts',(-52.8314289835239,-72.4904555356666,
173.617798149489));
#37471=CARTESIAN_POINT('Ctrl Pts',(-51.8661649351419,-72.6876403606086,
174.380902599416));
#37472=CARTESIAN_POINT('Ctrl Pts',(-51.7230869423191,-72.7971746590899,
175.613978373734));
#37473=CARTESIAN_POINT('Ctrl Pts',(-51.5800089494964,-72.9067089575712,
176.847054148052));
#37474=CARTESIAN_POINT('Ctrl Pts',(-52.3487517424243,-72.9190370685132,
177.8277821816));
#37475=CARTESIAN_POINT('Ctrl Pts',(-53.1174945353523,-72.9313651794552,
178.808510215148));
#37476=CARTESIAN_POINT('Ctrl Pts',(-54.3535605943834,-72.8938735080933,
178.962393326872));
#37477=CARTESIAN_POINT('Ctrl Pts',(-55.5896266534145,-72.8563818367314,
179.116276438596));
#37478=CARTESIAN_POINT('Ctrl Pts',(-56.5747668276306,-72.8456405411,178.35317198867));
#37479=CARTESIAN_POINT('Ctrl Pts',(-57.5599070018466,-72.8348992454687,
177.590067538743));
#37480=CARTESIAN_POINT('Ctrl Pts',(-57.7228611205034,-72.9118084762981,
176.356991764425));
#37481=CARTESIAN_POINT('Ctrl Pts',(-57.8858152391602,-72.9887177071275,
175.123915990107));
#37482=CARTESIAN_POINT('Ctrl Pts',(-57.1369485720663,-73.1628331254962,
174.143187956559));
#37483=CARTESIAN_POINT('Ctrl Pts',(-56.3880819049724,-73.3369485438649,
173.162459923011));
#37484=CARTESIAN_POINT('Ctrl Pts',(-55.1718919717753,-73.5608837445375,
173.008576811287));
#37485=CARTESIAN_POINT('Ctrl Pts',(-53.9557020385781,-73.7848189452101,
172.854693699562));
#37486=CARTESIAN_POINT('Ctrl Pts',(-52.9904379901961,-73.9820037701522,
173.617798149489));
#37487=CARTESIAN_POINT('Ctrl Pts',(-52.0251739418142,-74.1791885950942,
174.380902599416));
#37488=CARTESIAN_POINT('Ctrl Pts',(-51.8820959489914,-74.2887228935755,
175.613978373734));
#37489=CARTESIAN_POINT('Ctrl Pts',(-51.7390179561686,-74.3982571920568,
176.847054148052));
#37490=CARTESIAN_POINT('Ctrl Pts',(-52.5077607490965,-74.4105853029988,
177.8277821816));
#37491=CARTESIAN_POINT('Ctrl Pts',(-53.2765035420245,-74.4229134139408,
178.808510215148));
#37492=CARTESIAN_POINT('Ctrl Pts',(-54.5125696010556,-74.3854217425789,
178.962393326872));
#37493=CARTESIAN_POINT('Ctrl Pts',(-55.7486356600868,-74.347930071217,179.116276438596));
#37494=CARTESIAN_POINT('Ctrl Pts',(-56.7337758343028,-74.3371887755856,
178.35317198867));
#37495=CARTESIAN_POINT('Ctrl Pts',(-57.7189160085188,-74.3264474799543,
177.590067538743));
#37496=CARTESIAN_POINT('Ctrl Pts',(-57.8818701271756,-74.4033567107837,
176.356991764425));
#37497=CARTESIAN_POINT('Ctrl Pts',(-58.0448242458325,-74.4802659416131,
175.123915990107));
#37498=CARTESIAN_POINT('Ctrl Pts',(-57.2959575787385,-74.6543813599818,
174.143187956559));
#37499=CARTESIAN_POINT('Ctrl Pts',(-56.5470909116446,-74.8284967783505,
173.162459923011));
#37500=CARTESIAN_POINT('Ctrl Pts',(-55.3309009784475,-75.0524319790231,
173.008576811287));
#37501=CARTESIAN_POINT('Ctrl Pts',(-54.1147110452504,-75.2763671796957,
172.854693699562));
#37502=CARTESIAN_POINT('Ctrl Pts',(-53.1494469968684,-75.4735520046378,
173.617798149489));
#37503=CARTESIAN_POINT('Ctrl Pts',(-52.1841829484864,-75.6707368295798,
174.380902599416));
#37504=CARTESIAN_POINT('Ctrl Pts',(-52.0411049556636,-75.7802711280611,
175.613978373734));
#37505=CARTESIAN_POINT('Ctrl Pts',(-51.8980269628408,-75.8898054265424,
176.847054148052));
#37506=CARTESIAN_POINT('Ctrl Pts',(-52.6667697557687,-75.9021335374844,
177.8277821816));
#37507=CARTESIAN_POINT('Ctrl Pts',(-53.4355125486967,-75.9144616484264,
178.808510215148));
#37508=CARTESIAN_POINT('Ctrl Pts',(-54.6715786077279,-75.8769699770645,
178.962393326872));
#37509=CARTESIAN_POINT('Ctrl Pts',(-55.907644666759,-75.8394783057026,179.116276438596));
#37510=CARTESIAN_POINT('Ctrl Pts',(-56.892784840975,-75.8287370100712,178.35317198867));
#37511=CARTESIAN_POINT('Ctrl Pts',(-57.877925015191,-75.8179957144399,177.590067538743));
#37512=CARTESIAN_POINT('Ctrl Pts',(-58.0408791338479,-75.8949049452693,
176.356991764425));
#37513=CARTESIAN_POINT('Ctrl Pts',(-58.2038332525047,-75.9718141760987,
175.123915990107));
#37514=CARTESIAN_POINT('Ctrl Pts',(-57.4549665854108,-76.1459295944674,
174.143187956559));
#37515=CARTESIAN_POINT('Ctrl Pts',(-56.7060999183168,-76.3200450128361,
173.162459923011));
#37516=CARTESIAN_POINT('Ctrl Pts',(-55.4899099851197,-76.5439802135087,
173.008576811287));
#37517=CARTESIAN_POINT('Ctrl Pts',(-54.2737200519226,-76.7679154141813,
172.854693699562));
#37518=CARTESIAN_POINT('Ctrl Pts',(-53.3084560035406,-76.9651002391234,
173.617798149489));
#37519=CARTESIAN_POINT('Ctrl Pts',(-52.3431919551586,-77.1622850640654,
174.380902599416));
#37520=CARTESIAN_POINT('Ctrl Pts',(-52.2001139623358,-77.2718193625467,
175.613978373734));
#37521=CARTESIAN_POINT('Ctrl Pts',(-52.057035969513,-77.381353661028,176.847054148052));
#37522=CARTESIAN_POINT('Ctrl Pts',(-52.825778762441,-77.39368177197,177.8277821816));
#37523=CARTESIAN_POINT('Ctrl Pts',(-53.5945215553689,-77.406009882912,178.808510215148));
#37524=CARTESIAN_POINT('Ctrl Pts',(-54.8305876144001,-77.3685182115501,
178.962393326872));
#37525=CARTESIAN_POINT('Ctrl Pts',(-56.0666536734312,-77.3310265401882,
179.116276438596));
#37526=CARTESIAN_POINT('Ctrl Pts',(-57.0517938476472,-77.3202852445568,
178.35317198867));
#37527=CARTESIAN_POINT('Ctrl Pts',(-58.0369340218633,-77.3095439489255,
177.590067538743));
#37528=CARTESIAN_POINT('Ctrl Pts',(-58.1998881405201,-77.3864531797549,
176.356991764425));
#37529=CARTESIAN_POINT('Ctrl Pts',(-58.3628422591769,-77.4633624105843,
175.123915990107));
#37530=CARTESIAN_POINT('Ctrl Pts',(-57.613975592083,-77.637477828953,174.143187956559));
#37531=CARTESIAN_POINT('Ctrl Pts',(-56.8651089249891,-77.8115932473217,
173.162459923011));
#37532=CARTESIAN_POINT('Ctrl Pts',(-55.6489189917919,-78.0355284479943,
173.008576811287));
#37533=CARTESIAN_POINT('Ctrl Pts',(-54.4327290585948,-78.259463648667,172.854693699562));
#37534=CARTESIAN_POINT('Ctrl Pts',(-53.4674650102128,-78.456648473609,173.617798149489));
#37535=CARTESIAN_POINT('Ctrl Pts',(-52.5022009618309,-78.653833298551,174.380902599416));
#37536=CARTESIAN_POINT('Ctrl Pts',(-52.359122969008,-78.7633675970323,175.613978373734));
#37537=CARTESIAN_POINT('Ctrl Pts',(-52.2160449761853,-78.8729018955136,
176.847054148052));
#37538=CARTESIAN_POINT('Ctrl Pts',(-52.9847877691132,-78.8852300064556,
177.8277821816));
#37539=CARTESIAN_POINT('Ctrl Pts',(-53.7535305620412,-78.8975581173976,
178.808510215148));
#37540=CARTESIAN_POINT('Ctrl Pts',(-54.9895966210723,-78.8600664460357,
178.962393326872));
#37541=CARTESIAN_POINT('Ctrl Pts',(-56.2256626801035,-78.8225747746738,
179.116276438596));
#37542=CARTESIAN_POINT('Ctrl Pts',(-57.2108028543195,-78.8118334790424,
178.35317198867));
#37543=CARTESIAN_POINT('Ctrl Pts',(-58.1959430285355,-78.8010921834111,
177.590067538743));
#37544=CARTESIAN_POINT('Ctrl Pts',(-58.3588971471923,-78.8780014142405,
176.356991764425));
#37545=CARTESIAN_POINT('Ctrl Pts',(-58.5218512658491,-78.9549106450699,
175.123915990107));
#37546=CARTESIAN_POINT('Ctrl Pts',(-57.7729845987552,-79.1290260634386,
174.143187956559));
#37547=CARTESIAN_POINT('Ctrl Pts',(-57.0241179316613,-79.3031414818073,
173.162459923011));
#37548=CARTESIAN_POINT('Ctrl Pts',(-55.8079279984642,-79.5270766824799,
173.008576811287));
#37549=CARTESIAN_POINT('Ctrl Pts',(-54.5917380652671,-79.7510118831525,
172.854693699562));
#37550=CARTESIAN_POINT('Ctrl Pts',(-53.6264740168851,-79.9481967080946,
173.617798149489));
#37551=CARTESIAN_POINT('Ctrl Pts',(-52.6612099685031,-80.1453815330366,
174.380902599416));
#37552=CARTESIAN_POINT('Ctrl Pts',(-52.5181319756803,-80.2549158315179,
175.613978373734));
#37553=CARTESIAN_POINT('Ctrl Pts',(-52.3750539828575,-80.3644501299992,
176.847054148052));
#37554=CARTESIAN_POINT('Ctrl Pts',(-53.1437967757854,-80.3767782409412,
177.8277821816));
#37555=CARTESIAN_POINT('Ctrl Pts',(-53.9125395687134,-80.3891063518832,
178.808510215148));
#37556=CARTESIAN_POINT('Ctrl Pts',(-55.1486056277445,-80.3516146805213,
178.962393326872));
#37557=CARTESIAN_POINT('Ctrl Pts',(-56.3846716867757,-80.3141230091594,
179.116276438596));
#37558=CARTESIAN_POINT('Ctrl Pts',(-57.3698118609917,-80.303381713528,178.35317198867));
#37559=CARTESIAN_POINT('Ctrl Pts',(-58.3549520352077,-80.2926404178967,
177.590067538743));
#37560=CARTESIAN_POINT('Ctrl Pts',(-58.5179061538645,-80.3695496487261,
176.356991764425));
#37561=CARTESIAN_POINT('Ctrl Pts',(-58.6808602725214,-80.4464588795555,
175.123915990107));
#37562=CARTESIAN_POINT('Ctrl Pts',(-57.9319936054274,-80.6205742979242,
174.143187956559));
#37563=CARTESIAN_POINT('Ctrl Pts',(-57.1831269383335,-80.7946897162929,
173.162459923011));
#37564=CARTESIAN_POINT('Ctrl Pts',(-55.9669370051364,-81.0186249169655,
173.008576811287));
#37565=CARTESIAN_POINT('Ctrl Pts',(-54.7507470719393,-81.2425601176382,
172.854693699562));
#37566=CARTESIAN_POINT('Ctrl Pts',(-53.7854830235573,-81.4397449425802,
173.617798149489));
#37567=CARTESIAN_POINT('Ctrl Pts',(-52.8202189751753,-81.6369297675222,
174.380902599416));
#37568=CARTESIAN_POINT('Ctrl Pts',(-52.6771409823525,-81.7464640660035,
175.613978373734));
#37569=CARTESIAN_POINT('Ctrl Pts',(-52.5340629895297,-81.8559983644848,
176.847054148052));
#37570=CARTESIAN_POINT('Ctrl Pts',(-53.3028057824577,-81.8683264754268,
177.8277821816));
#37571=CARTESIAN_POINT('Ctrl Pts',(-54.0715485753856,-81.8806545863688,
178.808510215148));
#37572=CARTESIAN_POINT('Ctrl Pts',(-55.3076146344168,-81.8431629150069,
178.962393326872));
#37573=CARTESIAN_POINT('Ctrl Pts',(-56.5436806934479,-81.805671243645,179.116276438596));
#37574=CARTESIAN_POINT('Ctrl Pts',(-57.5288208676639,-81.7949299480136,
178.35317198867));
#37575=CARTESIAN_POINT('Ctrl Pts',(-58.5139610418799,-81.7841886523823,
177.590067538743));
#37576=CARTESIAN_POINT('Ctrl Pts',(-58.6769151605368,-81.8610978832117,
176.356991764425));
#37577=CARTESIAN_POINT('Ctrl Pts',(-58.8398692791936,-81.9380071140411,
175.123915990107));
#37578=CARTESIAN_POINT('Ctrl Pts',(-58.0910026120997,-82.1121225324098,
174.143187956559));
#37579=CARTESIAN_POINT('Ctrl Pts',(-57.3421359450057,-82.2862379507785,
173.162459923011));
#37580=CARTESIAN_POINT('Ctrl Pts',(-56.1259460118086,-82.5101731514511,
173.008576811287));
#37581=CARTESIAN_POINT('Ctrl Pts',(-54.9097560786115,-82.7341083521237,
172.854693699562));
#37582=CARTESIAN_POINT('Ctrl Pts',(-53.9444920302295,-82.9312931770658,
173.617798149489));
#37583=CARTESIAN_POINT('Ctrl Pts',(-52.9792279818475,-83.1284780020078,
174.380902599416));
#37584=CARTESIAN_POINT('Ctrl Pts',(-52.8361499890247,-83.2380123004891,
175.613978373734));
#37585=CARTESIAN_POINT('Ctrl Pts',(-52.6930719962019,-83.3475465989704,
176.847054148052));
#37586=CARTESIAN_POINT('Ctrl Pts',(-53.4618147891299,-83.3598747099124,
177.8277821816));
#37587=CARTESIAN_POINT('Ctrl Pts',(-54.2305575820579,-83.3722028208544,
178.808510215148));
#37588=CARTESIAN_POINT('Ctrl Pts',(-55.466623641089,-83.3347111494925,178.962393326872));
#37589=CARTESIAN_POINT('Ctrl Pts',(-56.7026897001201,-83.2972194781306,
179.116276438596));
#37590=CARTESIAN_POINT('Ctrl Pts',(-57.6878298743361,-83.2864781824993,
178.35317198867));
#37591=CARTESIAN_POINT('Ctrl Pts',(-58.6729700485522,-83.2757368868679,
177.590067538743));
#37592=CARTESIAN_POINT('Ctrl Pts',(-58.835924167209,-83.3526461176973,176.356991764425));
#37593=CARTESIAN_POINT('Ctrl Pts',(-58.9988782858658,-83.4295553485267,
175.123915990107));
#37594=CARTESIAN_POINT('Ctrl Pts',(-58.2500116187719,-83.6036707668954,
174.143187956559));
#37595=CARTESIAN_POINT('Ctrl Pts',(-57.501144951678,-83.7777861852641,173.162459923011));
#37596=CARTESIAN_POINT('Ctrl Pts',(-56.2849550184808,-84.0017213859367,
173.008576811287));
#37597=CARTESIAN_POINT('Ctrl Pts',(-55.0687650852837,-84.2256565866093,
172.854693699562));
#37598=CARTESIAN_POINT('Ctrl Pts',(-54.1035010369017,-84.4228414115514,
173.617798149489));
#37599=CARTESIAN_POINT('Ctrl Pts',(-53.1382369885197,-84.6200262364934,
174.380902599416));
#37600=CARTESIAN_POINT('Ctrl Pts',(-52.9951589956969,-84.7295605349747,
175.613978373734));
#37601=CARTESIAN_POINT('Ctrl Pts',(-52.8520810028742,-84.839094833456,176.847054148052));
#37602=CARTESIAN_POINT('Ctrl Pts',(-53.6208237958021,-84.851422944398,177.8277821816));
#37603=CARTESIAN_POINT('Ctrl Pts',(-54.3895665887301,-84.86375105534,178.808510215148));
#37604=CARTESIAN_POINT('Ctrl Pts',(-55.6256326477612,-84.8262593839781,
178.962393326872));
#37605=CARTESIAN_POINT('Ctrl Pts',(-56.8616987067924,-84.7887677126162,
179.116276438596));
#37606=CARTESIAN_POINT('Ctrl Pts',(-57.8468388810084,-84.7780264169849,
178.35317198867));
#37607=CARTESIAN_POINT('Ctrl Pts',(-58.8319790552244,-84.7672851213535,
177.590067538743));
#37608=CARTESIAN_POINT('Ctrl Pts',(-58.9949331738812,-84.8441943521829,
176.356991764425));
#37609=CARTESIAN_POINT('Ctrl Pts',(-59.157887292538,-84.9211035830123,175.123915990107));
#37610=CARTESIAN_POINT('Ctrl Pts',(-58.4090206254441,-85.095219001381,174.143187956559));
#37611=CARTESIAN_POINT('Ctrl Pts',(-57.6601539583502,-85.2693344197497,
173.162459923011));
#37612=CARTESIAN_POINT('Ctrl Pts',(-56.4439640251531,-85.4932696204223,
173.008576811287));
#37613=CARTESIAN_POINT('Ctrl Pts',(-55.227774091956,-85.717204821095,172.854693699562));
#37614=CARTESIAN_POINT('Ctrl Pts',(-54.262510043574,-85.914389646037,173.617798149489));
#37615=CARTESIAN_POINT('Ctrl Pts',(-53.297245995192,-86.111574470979,174.380902599416));
#37616=CARTESIAN_POINT('Ctrl Pts',(-53.1541680023692,-86.2211087694603,
175.613978373734));
#37617=CARTESIAN_POINT('Ctrl Pts',(-53.0110900095464,-86.3306430679416,
176.847054148052));
#37618=CARTESIAN_POINT('Ctrl Pts',(-53.7798328024743,-86.3429711788836,
177.8277821816));
#37619=CARTESIAN_POINT('Ctrl Pts',(-54.5485755954023,-86.3552992898256,
178.808510215148));
#37620=CARTESIAN_POINT('Ctrl Pts',(-55.7846416544334,-86.3178076184637,
178.962393326872));
#37621=CARTESIAN_POINT('Ctrl Pts',(-57.0207077134646,-86.2803159471018,
179.116276438596));
#37622=CARTESIAN_POINT('Ctrl Pts',(-58.0058478876806,-86.2695746514704,
178.35317198867));
#37623=CARTESIAN_POINT('Ctrl Pts',(-58.9909880618966,-86.2588333558391,
177.590067538743));
#37624=CARTESIAN_POINT('Ctrl Pts',(-59.1539421805534,-86.3357425866685,
176.356991764425));
#37625=CARTESIAN_POINT('Ctrl Pts',(-59.3168962992103,-86.4126518174979,
175.123915990107));
#37626=CARTESIAN_POINT('Ctrl Pts',(-58.5680296321163,-86.5867672358666,
174.143187956559));
#37627=CARTESIAN_POINT('Ctrl Pts',(-57.8191629650224,-86.7608826542353,
173.162459923011));
#37628=CARTESIAN_POINT('Ctrl Pts',(-56.6029730318253,-86.9848178549079,
173.008576811287));
#37629=CARTESIAN_POINT('Ctrl Pts',(-55.3867830986282,-87.2087530555805,
172.854693699562));
#37630=CARTESIAN_POINT('Ctrl Pts',(-54.4215190502462,-87.4059378805226,
173.617798149489));
#37631=CARTESIAN_POINT('Ctrl Pts',(-53.4562550018642,-87.6031227054646,
174.380902599416));
#37632=CARTESIAN_POINT('Ctrl Pts',(-53.3131770090414,-87.7126570039459,
175.613978373734));
#37633=CARTESIAN_POINT('Ctrl Pts',(-53.1700990162186,-87.8221913024272,
176.847054148052));
#37634=CARTESIAN_POINT('Ctrl Pts',(-53.9388418091466,-87.8345194133692,
177.8277821816));
#37635=CARTESIAN_POINT('Ctrl Pts',(-54.7075846020745,-87.8468475243112,
178.808510215148));
#37636=CARTESIAN_POINT('Ctrl Pts',(-55.9436506611057,-87.8093558529493,
178.962393326872));
#37637=CARTESIAN_POINT('Ctrl Pts',(-57.1797167201368,-87.7718641815874,
179.116276438596));
#37638=CARTESIAN_POINT('Ctrl Pts',(-58.1648568943528,-87.761122885956,178.35317198867));
#37639=CARTESIAN_POINT('Ctrl Pts',(-59.1499970685689,-87.7503815903247,
177.590067538743));
#37640=CARTESIAN_POINT('Ctrl Pts',(-59.3129511872257,-87.8272908211541,
176.356991764425));
#37641=CARTESIAN_POINT('Ctrl Pts',(-59.4759053058825,-87.9042000519835,
175.123915990107));
#37642=CARTESIAN_POINT('Ctrl Pts',(-58.7270386387886,-88.0783154703522,
174.143187956559));
#37643=CARTESIAN_POINT('Ctrl Pts',(-57.9781719716946,-88.2524308887209,
173.162459923011));
#37644=CARTESIAN_POINT('Ctrl Pts',(-56.7619820384975,-88.4763660893935,
173.008576811287));
#37645=CARTESIAN_POINT('Ctrl Pts',(-55.5457921053004,-88.7003012900661,
172.854693699562));
#37646=CARTESIAN_POINT('Ctrl Pts',(-54.5805280569184,-88.8974861150082,
173.617798149489));
#37647=CARTESIAN_POINT('Ctrl Pts',(-53.6152640085364,-89.0946709399502,
174.380902599416));
#37648=CARTESIAN_POINT('Ctrl Pts',(-53.4721860157136,-89.2042052384315,
175.613978373734));
#37649=CARTESIAN_POINT('Ctrl Pts',(-53.3291080228908,-89.3137395369128,
176.847054148052));
#37650=CARTESIAN_POINT('Ctrl Pts',(-54.0978508158188,-89.3260676478548,
177.8277821816));
#37651=CARTESIAN_POINT('Ctrl Pts',(-54.8665936087468,-89.3383957587968,
178.808510215148));
#37652=CARTESIAN_POINT('Ctrl Pts',(-56.1026596677779,-89.3009040874349,
178.962393326872));
#37653=CARTESIAN_POINT('Ctrl Pts',(-57.3387257268091,-89.263412416073,179.116276438596));
#37654=CARTESIAN_POINT('Ctrl Pts',(-58.3238659010251,-89.2526711204416,
178.35317198867));
#37655=CARTESIAN_POINT('Ctrl Pts',(-59.3090060752411,-89.2419298248103,
177.590067538743));
#37656=CARTESIAN_POINT('Ctrl Pts',(-59.4719601938979,-89.3188390556397,
176.356991764425));
#37657=CARTESIAN_POINT('Ctrl Pts',(-59.6349143125547,-89.3957482864691,
175.123915990107));
#37658=CARTESIAN_POINT('Ctrl Pts',(-58.8860476454608,-89.5698637048378,
174.143187956559));
#37659=CARTESIAN_POINT('Ctrl Pts',(-58.1371809783669,-89.7439791232065,
173.162459923011));
#37660=CARTESIAN_POINT('Ctrl Pts',(-56.9209910451698,-89.9679143238791,
173.008576811287));
#37661=CARTESIAN_POINT('Ctrl Pts',(-55.7048011119726,-90.1918495245517,
172.854693699562));
#37662=CARTESIAN_POINT('Ctrl Pts',(-54.7395370635906,-90.3890343494938,
173.617798149489));
#37663=CARTESIAN_POINT('Ctrl Pts',(-53.7742730152086,-90.5862191744358,
174.380902599416));
#37664=CARTESIAN_POINT('Ctrl Pts',(-53.6311950223859,-90.6957534729171,
175.613978373734));
#37665=CARTESIAN_POINT('Ctrl Pts',(-53.4881170295631,-90.8052877713984,
176.847054148052));
#37666=CARTESIAN_POINT('Ctrl Pts',(-54.256859822491,-90.8176158823404,177.8277821816));
#37667=CARTESIAN_POINT('Ctrl Pts',(-55.025602615419,-90.8299439932824,178.808510215148));
#37668=CARTESIAN_POINT('Ctrl Pts',(-56.2616686744501,-90.7924523219205,
178.962393326872));
#37669=CARTESIAN_POINT('Ctrl Pts',(-57.4977347334813,-90.7549606505586,
179.116276438596));
#37670=CARTESIAN_POINT('Ctrl Pts',(-58.4828749076973,-90.7442193549272,
178.35317198867));
#37671=CARTESIAN_POINT('Ctrl Pts',(-59.4680150819133,-90.7334780592959,
177.590067538743));
#37672=CARTESIAN_POINT('Ctrl Pts',(-59.6309692005701,-90.8103872901253,
176.356991764425));
#37673=CARTESIAN_POINT('Ctrl Pts',(-59.793923319227,-90.8872965209547,175.123915990107));
#37674=CARTESIAN_POINT('Ctrl Pts',(-59.045056652133,-91.0614119393234,174.143187956559));
#37675=CARTESIAN_POINT('Ctrl Pts',(-58.2961899850391,-91.2355273576921,
173.162459923011));
#37676=CARTESIAN_POINT('Ctrl Pts',(-57.080000051842,-91.4594625583647,173.008576811287));
#37677=CARTESIAN_POINT('Ctrl Pts',(-55.8638101186449,-91.6833977590373,
172.854693699562));
#37678=CARTESIAN_POINT('Ctrl Pts',(-54.8985460702629,-91.8805825839794,
173.617798149489));
#37679=CARTESIAN_POINT('Ctrl Pts',(-53.9332820218809,-92.0777674089214,
174.380902599416));
#37680=CARTESIAN_POINT('Ctrl Pts',(-53.7902040290581,-92.1873017074027,
175.613978373734));
#37681=CARTESIAN_POINT('Ctrl Pts',(-53.6471260362353,-92.296836005884,176.847054148052));
#37682=CARTESIAN_POINT('Ctrl Pts',(-54.4158688291633,-92.309164116826,177.8277821816));
#37683=CARTESIAN_POINT('Ctrl Pts',(-55.1846116220912,-92.321492227768,178.808510215148));
#37684=CARTESIAN_POINT('Ctrl Pts',(-56.4206776811223,-92.2840005564061,
178.962393326872));
#37685=CARTESIAN_POINT('Ctrl Pts',(-57.6567437401535,-92.2465088850442,
179.116276438596));
#37686=CARTESIAN_POINT('Ctrl Pts',(-58.6418839143695,-92.2357675894128,
178.35317198867));
#37687=CARTESIAN_POINT('Ctrl Pts',(-59.6270240885855,-92.2250262937815,
177.590067538743));
#37688=CARTESIAN_POINT('Ctrl Pts',(-59.7899782072423,-92.3019355246109,
176.356991764425));
#37689=CARTESIAN_POINT('Ctrl Pts',(-59.9529323258992,-92.3788447554403,
175.123915990107));
#37690=CARTESIAN_POINT('Ctrl Pts',(-59.2040656588053,-92.552960173809,174.143187956559));
#37691=CARTESIAN_POINT('Ctrl Pts',(-58.4551989917113,-92.7270755921777,
173.162459923011));
#37692=CARTESIAN_POINT('Ctrl Pts',(-57.2390090585142,-92.9510107928503,
173.008576811287));
#37693=CARTESIAN_POINT('Ctrl Pts',(-56.0228191253171,-93.1749459935229,
172.854693699562));
#37694=CARTESIAN_POINT('Ctrl Pts',(-55.0575550769351,-93.372130818465,173.617798149489));
#37695=CARTESIAN_POINT('Ctrl Pts',(-54.0922910285531,-93.569315643407,174.380902599416));
#37696=CARTESIAN_POINT('Ctrl Pts',(-53.9492130357303,-93.6788499418883,
175.613978373734));
#37697=CARTESIAN_POINT('Ctrl Pts',(-53.8061350429075,-93.7883842403696,
176.847054148052));
#37698=CARTESIAN_POINT('Ctrl Pts',(-54.5748778358355,-93.8007123513116,
177.8277821816));
#37699=CARTESIAN_POINT('Ctrl Pts',(-55.3436206287634,-93.8130404622536,
178.808510215148));
#37700=CARTESIAN_POINT('Ctrl Pts',(-56.5796866877946,-93.7755487908917,
178.962393326872));
#37701=CARTESIAN_POINT('Ctrl Pts',(-57.8157527468257,-93.7380571195298,
179.116276438596));
#37702=CARTESIAN_POINT('Ctrl Pts',(-58.8008929210417,-93.7273158238985,
178.35317198867));
#37703=CARTESIAN_POINT('Ctrl Pts',(-59.7860330952578,-93.7165745282671,
177.590067538743));
#37704=CARTESIAN_POINT('Ctrl Pts',(-59.9489872139146,-93.7934837590965,
176.356991764425));
#37705=CARTESIAN_POINT('Ctrl Pts',(-60.1119413325714,-93.8703929899259,
175.123915990107));
#37706=CARTESIAN_POINT('Ctrl Pts',(-59.3630746654775,-94.0445084082946,
174.143187956559));
#37707=CARTESIAN_POINT('Ctrl Pts',(-58.6142079983836,-94.2186238266633,
173.162459923011));
#37708=CARTESIAN_POINT('Ctrl Pts',(-57.3980180651864,-94.4425590273359,
173.008576811287));
#37709=CARTESIAN_POINT('Ctrl Pts',(-56.1818281319893,-94.6664942280085,
172.854693699562));
#37710=CARTESIAN_POINT('Ctrl Pts',(-55.2165640836073,-94.8636790529506,
173.617798149489));
#37711=CARTESIAN_POINT('Ctrl Pts',(-54.2513000352253,-95.0608638778926,
174.380902599416));
#37712=CARTESIAN_POINT('Ctrl Pts',(-54.1082220424025,-95.1703981763739,
175.613978373734));
#37713=CARTESIAN_POINT('Ctrl Pts',(-53.9651440495798,-95.2799324748552,
176.847054148052));
#37714=CARTESIAN_POINT('Ctrl Pts',(-54.7338868425077,-95.2922605857972,
177.8277821816));
#37715=CARTESIAN_POINT('Ctrl Pts',(-55.5026296354357,-95.3045886967392,
178.808510215148));
#37716=CARTESIAN_POINT('Ctrl Pts',(-56.7386956944668,-95.2670970253773,
178.962393326872));
#37717=CARTESIAN_POINT('Ctrl Pts',(-57.974761753498,-95.2296053540154,179.116276438596));
#37718=CARTESIAN_POINT('Ctrl Pts',(-58.959901927714,-95.218864058384,178.35317198867));
#37719=CARTESIAN_POINT('Ctrl Pts',(-59.94504210193,-95.2081227627527,177.590067538743));
#37720=CARTESIAN_POINT('Ctrl Pts',(-60.1079962205868,-95.2850319935821,
176.356991764425));
#37721=CARTESIAN_POINT('Ctrl Pts',(-60.2709503392436,-95.3619412244115,
175.123915990107));
#37722=CARTESIAN_POINT('Ctrl Pts',(-59.5220836721497,-95.5360566427802,
174.143187956559));
#37723=CARTESIAN_POINT('Ctrl Pts',(-58.7732170050558,-95.7101720611489,
173.162459923011));
#37724=CARTESIAN_POINT('Ctrl Pts',(-57.5570270718587,-95.9341072618215,
173.008576811287));
#37725=CARTESIAN_POINT('Ctrl Pts',(-56.3408371386615,-96.1580424624942,
172.854693699562));
#37726=CARTESIAN_POINT('Ctrl Pts',(-55.3755730902795,-96.3552272874362,
173.617798149489));
#37727=CARTESIAN_POINT('Ctrl Pts',(-54.4103090418976,-96.5524121123782,
174.380902599416));
#37728=CARTESIAN_POINT('Ctrl Pts',(-54.2672310490748,-96.6619464108595,
175.613978373734));
#37729=CARTESIAN_POINT('Ctrl Pts',(-54.124153056252,-96.7714807093408,176.847054148052));
#37730=CARTESIAN_POINT('Ctrl Pts',(-54.8928958491799,-96.7838088202828,
177.8277821816));
#37731=CARTESIAN_POINT('Ctrl Pts',(-55.6616386421079,-96.7961369312248,
178.808510215148));
#37732=CARTESIAN_POINT('Ctrl Pts',(-56.897704701139,-96.7586452598629,178.962393326872));
#37733=CARTESIAN_POINT('Ctrl Pts',(-58.1337707601702,-96.721153588501,179.116276438596));
#37734=CARTESIAN_POINT('Ctrl Pts',(-59.1189109343862,-96.7104122928696,
178.35317198867));
#37735=CARTESIAN_POINT('Ctrl Pts',(-60.1040511086022,-96.6996709972383,
177.590067538743));
#37736=CARTESIAN_POINT('Ctrl Pts',(-60.267005227259,-96.7765802280677,176.356991764425));
#37737=CARTESIAN_POINT('Ctrl Pts',(-60.4299593459159,-96.8534894588971,
175.123915990107));
#37738=CARTESIAN_POINT('Ctrl Pts',(-59.6810926788219,-97.0276048772658,
174.143187956559));
#37739=CARTESIAN_POINT('Ctrl Pts',(-58.932226011728,-97.2017202956345,173.162459923011));
#37740=CARTESIAN_POINT('Ctrl Pts',(-57.7160360785309,-97.4256554963071,
173.008576811287));
#37741=CARTESIAN_POINT('Ctrl Pts',(-56.4998461453338,-97.6495906969797,
172.854693699562));
#37742=CARTESIAN_POINT('Ctrl Pts',(-55.5345820969518,-97.8467755219218,
173.617798149489));
#37743=CARTESIAN_POINT('Ctrl Pts',(-54.5693180485698,-98.0439603468638,
174.380902599416));
#37744=CARTESIAN_POINT('Ctrl Pts',(-54.426240055747,-98.1534946453451,175.613978373734));
#37745=CARTESIAN_POINT('Ctrl Pts',(-54.2831620629242,-98.2630289438264,
176.847054148052));
#37746=CARTESIAN_POINT('Ctrl Pts',(-55.0519048558522,-98.2753570547684,
177.8277821816));
#37747=CARTESIAN_POINT('Ctrl Pts',(-55.8206476487801,-98.2876851657105,
178.808510215148));
#37748=CARTESIAN_POINT('Ctrl Pts',(-57.0567137078113,-98.2501934943485,
178.962393326872));
#37749=CARTESIAN_POINT('Ctrl Pts',(-58.2927797668424,-98.2127018229866,
179.116276438596));
#37750=CARTESIAN_POINT('Ctrl Pts',(-59.2779199410584,-98.2019605273553,
178.35317198867));
#37751=CARTESIAN_POINT('Ctrl Pts',(-60.2630601152744,-98.1912192317239,
177.590067538743));
#37752=CARTESIAN_POINT('Ctrl Pts',(-60.4260142339313,-98.2681284625533,
176.356991764425));
#37753=CARTESIAN_POINT('Ctrl Pts',(-60.5889683525881,-98.3450376933827,
175.123915990107));
#37754=CARTESIAN_POINT('Ctrl Pts',(-59.8401016854942,-98.5191531117514,
174.143187956559));
#37755=CARTESIAN_POINT('Ctrl Pts',(-59.0912350184002,-98.6932685301201,
173.162459923011));
#37756=CARTESIAN_POINT('Ctrl Pts',(-57.8750450852031,-98.9172037307927,
173.008576811287));
#37757=CARTESIAN_POINT('Ctrl Pts',(-56.658855152006,-99.1411389314653,172.854693699562));
#37758=CARTESIAN_POINT('Ctrl Pts',(-55.693591103624,-99.3383237564074,173.617798149489));
#37759=CARTESIAN_POINT('Ctrl Pts',(-54.728327055242,-99.5355085813494,174.380902599416));
#37760=CARTESIAN_POINT('Ctrl Pts',(-54.5852490624192,-99.6450428798307,
175.613978373734));
#37761=CARTESIAN_POINT('Ctrl Pts',(-54.4421710695964,-99.754577178312,176.847054148052));
#37762=CARTESIAN_POINT('Ctrl Pts',(-55.2109138625244,-99.766905289254,177.8277821816));
#37763=CARTESIAN_POINT('Ctrl Pts',(-55.9796566554524,-99.779233400196,178.808510215148));
#37764=CARTESIAN_POINT('Ctrl Pts',(-57.2157227144835,-99.7417417288341,
178.962393326872));
#37765=CARTESIAN_POINT('Ctrl Pts',(-58.4517887735146,-99.7042500574722,
179.116276438596));
#37766=CARTESIAN_POINT('Ctrl Pts',(-59.4369289477306,-99.6935087618409,
178.35317198867));
#37767=CARTESIAN_POINT('Ctrl Pts',(-60.4220691219467,-99.6827674662096,
177.590067538743));
#37768=CARTESIAN_POINT('Ctrl Pts',(-60.5850232406035,-99.7596766970389,
176.356991764425));
#37769=CARTESIAN_POINT('Ctrl Pts',(-60.7479773592603,-99.8365859278683,
175.123915990107));
#37770=CARTESIAN_POINT('Ctrl Pts',(-59.9991106921664,-100.010701346237,
174.143187956559));
#37771=CARTESIAN_POINT('Ctrl Pts',(-59.2502440250725,-100.184816764606,
173.162459923011));
#37772=CARTESIAN_POINT('Ctrl Pts',(-58.0340540918753,-100.408751965278,
173.008576811287));
#37773=CARTESIAN_POINT('Ctrl Pts',(-56.8178641586782,-100.632687165951,
172.854693699562));
#37774=CARTESIAN_POINT('Ctrl Pts',(-55.8526001102962,-100.829871990893,
173.617798149489));
#37775=CARTESIAN_POINT('Ctrl Pts',(-54.8873360619142,-101.027056815835,
174.380902599416));
#37776=CARTESIAN_POINT('Ctrl Pts',(-54.7442580690915,-101.136591114316,
175.613978373734));
#37777=CARTESIAN_POINT('Ctrl Pts',(-54.6011800762687,-101.246125412798,
176.847054148052));
#37778=CARTESIAN_POINT('Ctrl Pts',(-55.3699228691966,-101.25845352374,177.8277821816));
#37779=CARTESIAN_POINT('Ctrl Pts',(-56.1386656621246,-101.270781634682,
178.808510215148));
#37780=CARTESIAN_POINT('Ctrl Pts',(-57.3747317211557,-101.23328996332,178.962393326872));
#37781=CARTESIAN_POINT('Ctrl Pts',(-58.6107977801869,-101.195798291958,
179.116276438596));
#37782=CARTESIAN_POINT('Ctrl Pts',(-59.5959379544029,-101.185056996326,
178.35317198867));
#37783=CARTESIAN_POINT('Ctrl Pts',(-60.5810781286189,-101.174315700695,
177.590067538743));
#37784=CARTESIAN_POINT('Ctrl Pts',(-60.7440322472757,-101.251224931525,
176.356991764425));
#37785=CARTESIAN_POINT('Ctrl Pts',(-60.9069863659325,-101.328134162354,
175.123915990107));
#37786=CARTESIAN_POINT('Ctrl Pts',(-60.1581196988386,-101.502249580723,
174.143187956559));
#37787=CARTESIAN_POINT('Ctrl Pts',(-59.4092530317447,-101.676364999091,
173.162459923011));
#37788=CARTESIAN_POINT('Ctrl Pts',(-58.1930630985476,-101.900300199764,
173.008576811287));
#37789=CARTESIAN_POINT('Ctrl Pts',(-56.9768731653505,-102.124235400437,
172.854693699562));
#37790=CARTESIAN_POINT('Ctrl Pts',(-56.0116091169685,-102.321420225379,
173.617798149489));
#37791=CARTESIAN_POINT('Ctrl Pts',(-55.0463450685865,-102.518605050321,
174.380902599416));
#37792=CARTESIAN_POINT('Ctrl Pts',(-54.9032670757637,-102.628139348802,
175.613978373734));
#37793=CARTESIAN_POINT('Ctrl Pts',(-54.7601890829409,-102.737673647283,
176.847054148052));
#37794=CARTESIAN_POINT('Ctrl Pts',(-55.5289318758688,-102.750001758225,
177.8277821816));
#37795=CARTESIAN_POINT('Ctrl Pts',(-56.2976746687968,-102.762329869167,
178.808510215148));
#37796=CARTESIAN_POINT('Ctrl Pts',(-57.5337407278279,-102.724838197805,
178.962393326872));
#37797=CARTESIAN_POINT('Ctrl Pts',(-58.7698067868591,-102.687346526443,
179.116276438596));
#37798=CARTESIAN_POINT('Ctrl Pts',(-59.7549469610751,-102.676605230812,
178.35317198867));
#37799=CARTESIAN_POINT('Ctrl Pts',(-60.7400871352911,-102.665863935181,
177.590067538743));
#37800=CARTESIAN_POINT('Ctrl Pts',(-60.9030412539479,-102.74277316601,176.356991764425));
#37801=CARTESIAN_POINT('Ctrl Pts',(-61.0659953726048,-102.81968239684,175.123915990107));
#37802=CARTESIAN_POINT('Ctrl Pts',(-60.3171287055108,-102.993797815208,
174.143187956559));
#37803=CARTESIAN_POINT('Ctrl Pts',(-59.5682620384169,-103.167913233577,
173.162459923011));
#37804=CARTESIAN_POINT('Ctrl Pts',(-58.3520721052198,-103.39184843425,173.008576811287));
#37805=CARTESIAN_POINT('Ctrl Pts',(-57.1358821720227,-103.615783634922,
172.854693699562));
#37806=CARTESIAN_POINT('Ctrl Pts',(-56.1706181236407,-103.812968459864,
173.617798149489));
#37807=CARTESIAN_POINT('Ctrl Pts',(-55.2053540752587,-104.010153284806,
174.380902599416));
#37808=CARTESIAN_POINT('Ctrl Pts',(-55.0622760824359,-104.119687583288,
175.613978373734));
#37809=CARTESIAN_POINT('Ctrl Pts',(-54.9191980896131,-104.229221881769,
176.847054148052));
#37810=CARTESIAN_POINT('Ctrl Pts',(-55.6879408825411,-104.241549992711,
177.8277821816));
#37811=CARTESIAN_POINT('Ctrl Pts',(-56.456683675469,-104.253878103653,178.808510215148));
#37812=CARTESIAN_POINT('Ctrl Pts',(-57.6927497345002,-104.216386432291,
178.962393326872));
#37813=CARTESIAN_POINT('Ctrl Pts',(-58.9288157935313,-104.178894760929,
179.116276438596));
#37814=CARTESIAN_POINT('Ctrl Pts',(-59.9139559677473,-104.168153465298,
178.35317198867));
#37815=CARTESIAN_POINT('Ctrl Pts',(-60.8990961419634,-104.157412169666,
177.590067538743));
#37816=CARTESIAN_POINT('Ctrl Pts',(-61.0620502606202,-104.234321400496,
176.356991764425));
#37817=CARTESIAN_POINT('Ctrl Pts',(-61.225004379277,-104.311230631325,175.123915990107));
#37818=CARTESIAN_POINT('Ctrl Pts',(-60.4761377121831,-104.485346049694,
174.143187956559));
#37819=CARTESIAN_POINT('Ctrl Pts',(-59.7272710450891,-104.659461468063,
173.162459923011));
#37820=CARTESIAN_POINT('Ctrl Pts',(-58.511081111892,-104.883396668735,173.008576811287));
#37821=CARTESIAN_POINT('Ctrl Pts',(-57.2948911786949,-105.107331869408,
172.854693699562));
#37822=CARTESIAN_POINT('Ctrl Pts',(-56.3296271303129,-105.30451669435,173.617798149489));
#37823=CARTESIAN_POINT('Ctrl Pts',(-55.3643630819309,-105.501701519292,
174.380902599416));
#37824=CARTESIAN_POINT('Ctrl Pts',(-55.2212850891081,-105.611235817773,
175.613978373734));
#37825=CARTESIAN_POINT('Ctrl Pts',(-55.0782070962854,-105.720770116254,
176.847054148052));
#37826=CARTESIAN_POINT('Ctrl Pts',(-55.8469498892133,-105.733098227196,
177.8277821816));
#37827=CARTESIAN_POINT('Ctrl Pts',(-56.6156926821413,-105.745426338138,
178.808510215148));
#37828=CARTESIAN_POINT('Ctrl Pts',(-57.8517587411724,-105.707934666776,
178.962393326872));
#37829=CARTESIAN_POINT('Ctrl Pts',(-59.0878248002036,-105.670442995415,
179.116276438596));
#37830=CARTESIAN_POINT('Ctrl Pts',(-60.0729649744196,-105.659701699783,
178.35317198867));
#37831=CARTESIAN_POINT('Ctrl Pts',(-61.0581051486356,-105.648960404152,
177.590067538743));
#37832=CARTESIAN_POINT('Ctrl Pts',(-61.2210592672924,-105.725869634981,
176.356991764425));
#37833=CARTESIAN_POINT('Ctrl Pts',(-61.3840133859492,-105.802778865811,
175.123915990107));
#37834=CARTESIAN_POINT('Ctrl Pts',(-60.6351467188553,-105.976894284179,
174.143187956559));
#37835=CARTESIAN_POINT('Ctrl Pts',(-59.8862800517614,-106.151009702548,
173.162459923011));
#37836=CARTESIAN_POINT('Ctrl Pts',(-58.6700901185642,-106.374944903221,
173.008576811287));
#37837=CARTESIAN_POINT('Ctrl Pts',(-57.4539001853671,-106.598880103893,
172.854693699562));
#37838=CARTESIAN_POINT('Ctrl Pts',(-56.4886361369851,-106.796064928835,
173.617798149489));
#37839=CARTESIAN_POINT('Ctrl Pts',(-55.5233720886032,-106.993249753777,
174.380902599416));
#37840=CARTESIAN_POINT('Ctrl Pts',(-55.3802940957804,-107.102784052259,
175.613978373734));
#37841=CARTESIAN_POINT('Ctrl Pts',(-55.2372161029576,-107.21231835074,176.847054148052));
#37842=CARTESIAN_POINT('Ctrl Pts',(-56.0059588958855,-107.224646461682,
177.8277821816));
#37843=CARTESIAN_POINT('Ctrl Pts',(-56.7747016888135,-107.236974572624,
178.808510215148));
#37844=CARTESIAN_POINT('Ctrl Pts',(-58.0107677478446,-107.199482901262,
178.962393326872));
#37845=CARTESIAN_POINT('Ctrl Pts',(-59.2468338068758,-107.1619912299,179.116276438596));
#37846=CARTESIAN_POINT('Ctrl Pts',(-60.2319739810918,-107.151249934269,
178.35317198867));
#37847=CARTESIAN_POINT('Ctrl Pts',(-61.2171141553078,-107.140508638638,
177.590067538743));
#37848=CARTESIAN_POINT('Ctrl Pts',(-61.3800682739646,-107.217417869467,
176.356991764425));
#37849=CARTESIAN_POINT('Ctrl Pts',(-61.5430223926215,-107.294327100296,
175.123915990107));
#37850=CARTESIAN_POINT('Ctrl Pts',(-60.7941557255275,-107.468442518665,
174.143187956559));
#37851=CARTESIAN_POINT('Ctrl Pts',(-60.0452890584336,-107.642557937034,
173.162459923011));
#37852=CARTESIAN_POINT('Ctrl Pts',(-58.8290991252365,-107.866493137706,
173.008576811287));
#37853=CARTESIAN_POINT('Ctrl Pts',(-57.6129091920394,-108.090428338379,
172.854693699562));
#37854=CARTESIAN_POINT('Ctrl Pts',(-56.6476451436574,-108.287613163321,
173.617798149489));
#37855=CARTESIAN_POINT('Ctrl Pts',(-55.6823810952754,-108.484797988263,
174.380902599416));
#37856=CARTESIAN_POINT('Ctrl Pts',(-55.5393031024526,-108.594332286744,
175.613978373734));
#37857=CARTESIAN_POINT('Ctrl Pts',(-55.3962251096298,-108.703866585226,
176.847054148052));
#37858=CARTESIAN_POINT('Ctrl Pts',(-56.1649679025577,-108.716194696168,
177.8277821816));
#37859=CARTESIAN_POINT('Ctrl Pts',(-56.9337106954857,-108.72852280711,178.808510215148));
#37860=CARTESIAN_POINT('Ctrl Pts',(-58.1697767545169,-108.691031135748,
178.962393326872));
#37861=CARTESIAN_POINT('Ctrl Pts',(-59.405842813548,-108.653539464386,179.116276438596));
#37862=CARTESIAN_POINT('Ctrl Pts',(-60.390982987764,-108.642798168754,178.35317198867));
#37863=CARTESIAN_POINT('Ctrl Pts',(-61.37612316198,-108.632056873123,177.590067538743));
#37864=CARTESIAN_POINT('Ctrl Pts',(-61.5390772806369,-108.708966103953,
176.356991764425));
#37865=CARTESIAN_POINT('Ctrl Pts',(-61.7020313992937,-108.785875334782,
175.123915990107));
#37866=CARTESIAN_POINT('Ctrl Pts',(-60.9531647321997,-108.959990753151,
174.143187956559));
#37867=CARTESIAN_POINT('Ctrl Pts',(-60.2042980651058,-109.134106171519,
173.162459923011));
#37868=CARTESIAN_POINT('Ctrl Pts',(-58.9881081319087,-109.358041372192,
173.008576811287));
#37869=CARTESIAN_POINT('Ctrl Pts',(-57.7719181987116,-109.581976572865,
172.854693699562));
#37870=CARTESIAN_POINT('Ctrl Pts',(-56.8066541503296,-109.779161397807,
173.617798149489));
#37871=CARTESIAN_POINT('Ctrl Pts',(-55.8413901019476,-109.976346222749,
174.380902599416));
#37872=CARTESIAN_POINT('Ctrl Pts',(-55.6983121091248,-110.08588052123,175.613978373734));
#37873=CARTESIAN_POINT('Ctrl Pts',(-55.555234116302,-110.195414819711,176.847054148052));
#37874=CARTESIAN_POINT('Ctrl Pts',(-56.32397690923,-110.207742930653,177.8277821816));
#37875=CARTESIAN_POINT('Ctrl Pts',(-57.092719702158,-110.220071041595,178.808510215148));
#37876=CARTESIAN_POINT('Ctrl Pts',(-58.3287857611891,-110.182579370233,
178.962393326872));
#37877=CARTESIAN_POINT('Ctrl Pts',(-59.5648518202202,-110.145087698871,
179.116276438596));
#37878=CARTESIAN_POINT('Ctrl Pts',(-60.5499919944362,-110.13434640324,178.35317198867));
#37879=CARTESIAN_POINT('Ctrl Pts',(-61.5351321686523,-110.123605107609,
177.590067538743));
#37880=CARTESIAN_POINT('Ctrl Pts',(-61.6980862873091,-110.200514338438,
176.356991764425));
#37881=CARTESIAN_POINT('Ctrl Pts',(-61.8610404059659,-110.277423569268,
175.123915990107));
#37882=CARTESIAN_POINT('Ctrl Pts',(-61.112173738872,-110.451538987636,174.143187956559));
#37883=CARTESIAN_POINT('Ctrl Pts',(-60.363307071778,-110.625654406005,173.162459923011));
#37884=CARTESIAN_POINT('Ctrl Pts',(-59.1471171385809,-110.849589606678,
173.008576811287));
#37885=CARTESIAN_POINT('Ctrl Pts',(-57.9309272053838,-111.07352480735,172.854693699562));
#37886=CARTESIAN_POINT('Ctrl Pts',(-56.9656631570018,-111.270709632292,
173.617798149489));
#37887=CARTESIAN_POINT('Ctrl Pts',(-56.0003991086198,-111.467894457234,
174.380902599416));
#37888=CARTESIAN_POINT('Ctrl Pts',(-55.857321115797,-111.577428755716,175.613978373734));
#37889=CARTESIAN_POINT('Ctrl Pts',(-55.7142431229743,-111.686963054197,
176.847054148052));
#37890=CARTESIAN_POINT('Ctrl Pts',(-56.4829859159022,-111.699291165139,
177.8277821816));
#37891=CARTESIAN_POINT('Ctrl Pts',(-57.2517287088302,-111.711619276081,
178.808510215148));
#37892=CARTESIAN_POINT('Ctrl Pts',(-58.4877947678613,-111.674127604719,
178.962393326872));
#37893=CARTESIAN_POINT('Ctrl Pts',(-59.7238608268925,-111.636635933357,
179.116276438596));
#37894=CARTESIAN_POINT('Ctrl Pts',(-60.7090010011085,-111.625894637726,
178.35317198867));
#37895=CARTESIAN_POINT('Ctrl Pts',(-61.6941411753245,-111.615153342094,
177.590067538743));
#37896=CARTESIAN_POINT('Ctrl Pts',(-61.8570952939813,-111.692062572924,
176.356991764425));
#37897=CARTESIAN_POINT('Ctrl Pts',(-62.0200494126381,-111.768971803753,
175.123915990107));
#37898=CARTESIAN_POINT('Ctrl Pts',(-61.2711827455442,-111.943087222122,
174.143187956559));
#37899=CARTESIAN_POINT('Ctrl Pts',(-60.5223160784503,-112.117202640491,
173.162459923011));
#37900=CARTESIAN_POINT('Ctrl Pts',(-59.3061261452532,-112.341137841163,
173.008576811287));
#37901=CARTESIAN_POINT('Ctrl Pts',(-58.0899362120561,-112.565073041836,
172.854693699562));
#37902=CARTESIAN_POINT('Ctrl Pts',(-57.124672163674,-112.762257866778,173.617798149489));
#37903=CARTESIAN_POINT('Ctrl Pts',(-56.1594081152921,-112.95944269172,174.380902599416));
#37904=CARTESIAN_POINT('Ctrl Pts',(-56.0163301224693,-113.068976990201,
175.613978373734));
#37905=CARTESIAN_POINT('Ctrl Pts',(-55.8732521296465,-113.178511288682,
176.847054148052));
#37906=CARTESIAN_POINT('Ctrl Pts',(-56.6419949225744,-113.190839399624,
177.8277821816));
#37907=CARTESIAN_POINT('Ctrl Pts',(-57.4107377155024,-113.203167510566,
178.808510215148));
#37908=CARTESIAN_POINT('Ctrl Pts',(-58.6468037745335,-113.165675839205,
178.962393326872));
#37909=CARTESIAN_POINT('Ctrl Pts',(-59.8828698335647,-113.128184167843,
179.116276438596));
#37910=CARTESIAN_POINT('Ctrl Pts',(-60.8680100077807,-113.117442872211,
178.35317198867));
#37911=CARTESIAN_POINT('Ctrl Pts',(-61.8531501819967,-113.10670157658,177.590067538743));
#37912=CARTESIAN_POINT('Ctrl Pts',(-62.0161043006535,-113.183610807409,
176.356991764425));
#37913=CARTESIAN_POINT('Ctrl Pts',(-62.1790584193104,-113.260520038239,
175.123915990107));
#37914=CARTESIAN_POINT('Ctrl Pts',(-61.4301917522164,-113.434635456607,
174.143187956559));
#37915=CARTESIAN_POINT('Ctrl Pts',(-60.6813250851225,-113.608750874976,
173.162459923011));
#37916=CARTESIAN_POINT('Ctrl Pts',(-59.4651351519254,-113.832686075649,
173.008576811287));
#37917=CARTESIAN_POINT('Ctrl Pts',(-58.2489452187283,-114.056621276321,
172.854693699562));
#37918=CARTESIAN_POINT('Ctrl Pts',(-57.2836811703463,-114.253806101263,
173.617798149489));
#37919=CARTESIAN_POINT('Ctrl Pts',(-56.3184171219643,-114.450990926205,
174.380902599416));
#37920=CARTESIAN_POINT('Ctrl Pts',(-56.1753391291415,-114.560525224687,
175.613978373734));
#37921=CARTESIAN_POINT('Ctrl Pts',(-56.0322611363187,-114.670059523168,
176.847054148052));
#37922=CARTESIAN_POINT('Ctrl Pts',(-56.8010039292467,-114.68238763411,177.8277821816));
#37923=CARTESIAN_POINT('Ctrl Pts',(-57.5697467221746,-114.694715745052,
178.808510215148));
#37924=CARTESIAN_POINT('Ctrl Pts',(-58.8058127812058,-114.65722407369,178.962393326872));
#37925=CARTESIAN_POINT('Ctrl Pts',(-60.0418788402369,-114.619732402328,
179.116276438596));
#37926=CARTESIAN_POINT('Ctrl Pts',(-61.0270190144529,-114.608991106697,
178.35317198867));
#37927=CARTESIAN_POINT('Ctrl Pts',(-62.0121591886689,-114.598249811066,
177.590067538743));
#37928=CARTESIAN_POINT('Ctrl Pts',(-62.1751133073258,-114.675159041895,
176.356991764425));
#37929=CARTESIAN_POINT('Ctrl Pts',(-62.3380674259826,-114.752068272724,
175.123915990107));
#37930=CARTESIAN_POINT('Ctrl Pts',(-61.5892007588887,-114.926183691093,
174.143187956559));
#37931=CARTESIAN_POINT('Ctrl Pts',(-60.8403340917947,-115.100299109462,
173.162459923011));
#37932=CARTESIAN_POINT('Ctrl Pts',(-59.6241441585976,-115.324234310134,
173.008576811287));
#37933=CARTESIAN_POINT('Ctrl Pts',(-58.4079542254005,-115.548169510807,
172.854693699562));
#37934=CARTESIAN_POINT('Ctrl Pts',(-57.4426901770185,-115.745354335749,
173.617798149489));
#37935=CARTESIAN_POINT('Ctrl Pts',(-56.4774261286365,-115.942539160691,
174.380902599416));
#37936=CARTESIAN_POINT('Ctrl Pts',(-56.3343481358137,-116.052073459172,
175.613978373734));
#37937=CARTESIAN_POINT('Ctrl Pts',(-56.1912701429909,-116.161607757654,
176.847054148052));
#37938=CARTESIAN_POINT('Ctrl Pts',(-56.9600129359189,-116.173935868596,
177.8277821816));
#37939=CARTESIAN_POINT('Ctrl Pts',(-57.7287557288468,-116.186263979538,
178.808510215148));
#37940=CARTESIAN_POINT('Ctrl Pts',(-58.964821787878,-116.148772308176,178.962393326872));
#37941=CARTESIAN_POINT('Ctrl Pts',(-60.2008878469091,-116.111280636814,
179.116276438596));
#37942=CARTESIAN_POINT('Ctrl Pts',(-61.1860280211252,-116.100539341182,
178.35317198867));
#37943=CARTESIAN_POINT('Ctrl Pts',(-62.1711681953412,-116.089798045551,
177.590067538743));
#37944=CARTESIAN_POINT('Ctrl Pts',(-62.334122313998,-116.166707276381,176.356991764425));
#37945=CARTESIAN_POINT('Ctrl Pts',(-62.4970764326548,-116.24361650721,175.123915990107));
#37946=CARTESIAN_POINT('Ctrl Pts',(-61.7482097655609,-116.417731925579,
174.143187956559));
#37947=CARTESIAN_POINT('Ctrl Pts',(-60.999343098467,-116.591847343947,173.162459923011));
#37948=CARTESIAN_POINT('Ctrl Pts',(-59.7831531652698,-116.81578254462,173.008576811287));
#37949=CARTESIAN_POINT('Ctrl Pts',(-58.5669632320727,-117.039717745293,
172.854693699562));
#37950=CARTESIAN_POINT('Ctrl Pts',(-57.6016991836907,-117.236902570235,
173.617798149489));
#37951=CARTESIAN_POINT('Ctrl Pts',(-56.6364351353087,-117.434087395177,
174.380902599416));
#37952=CARTESIAN_POINT('Ctrl Pts',(-56.4933571424859,-117.543621693658,
175.613978373734));
#37953=CARTESIAN_POINT('Ctrl Pts',(-56.3502791496632,-117.653155992139,
176.847054148052));
#37954=CARTESIAN_POINT('Ctrl Pts',(-57.1190219425911,-117.665484103081,
177.8277821816));
#37955=CARTESIAN_POINT('Ctrl Pts',(-57.8877647355191,-117.677812214023,
178.808510215148));
#37956=CARTESIAN_POINT('Ctrl Pts',(-59.1238307945502,-117.640320542661,
178.962393326872));
#37957=CARTESIAN_POINT('Ctrl Pts',(-60.3598968535814,-117.602828871299,
179.116276438596));
#37958=CARTESIAN_POINT('Ctrl Pts',(-61.3450370277974,-117.592087575668,
178.35317198867));
#37959=CARTESIAN_POINT('Ctrl Pts',(-62.3301772020134,-117.581346280037,
177.590067538743));
#37960=CARTESIAN_POINT('Ctrl Pts',(-62.4931313206702,-117.658255510866,
176.356991764425));
#37961=CARTESIAN_POINT('Ctrl Pts',(-62.656085439327,-117.735164741696,175.123915990107));
#37962=CARTESIAN_POINT('Ctrl Pts',(-61.9072187722331,-117.909280160064,
174.143187956559));
#37963=CARTESIAN_POINT('Ctrl Pts',(-61.1583521051392,-118.083395578433,
173.162459923011));
#37964=CARTESIAN_POINT('Ctrl Pts',(-59.9421621719421,-118.307330779106,
173.008576811287));
#37965=CARTESIAN_POINT('Ctrl Pts',(-58.725972238745,-118.531265979778,172.854693699562));
#37966=CARTESIAN_POINT('Ctrl Pts',(-57.760708190363,-118.72845080472,173.617798149489));
#37967=CARTESIAN_POINT('Ctrl Pts',(-56.795444141981,-118.925635629662,174.380902599416));
#37968=CARTESIAN_POINT('Ctrl Pts',(-56.6523661491582,-119.035169928144,
175.613978373734));
#37969=CARTESIAN_POINT('Ctrl Pts',(-56.5092881563354,-119.144704226625,
176.847054148052));
#37970=CARTESIAN_POINT('Ctrl Pts',(-57.2780309492633,-119.157032337567,
177.8277821816));
#37971=CARTESIAN_POINT('Ctrl Pts',(-58.0467737421913,-119.169360448509,
178.808510215148));
#37972=CARTESIAN_POINT('Ctrl Pts',(-59.2828398012224,-119.131868777147,
178.962393326872));
#37973=CARTESIAN_POINT('Ctrl Pts',(-60.5189058602536,-119.094377105785,
179.116276438596));
#37974=CARTESIAN_POINT('Ctrl Pts',(-61.5040460344696,-119.083635810154,
178.35317198867));
#37975=CARTESIAN_POINT('Ctrl Pts',(-62.4891862086856,-119.072894514522,
177.590067538743));
#37976=CARTESIAN_POINT('Ctrl Pts',(-62.6521403273424,-119.149803745352,
176.356991764425));
#37977=CARTESIAN_POINT('Ctrl Pts',(-62.8150944459993,-119.226712976181,
175.123915990107));
#37978=CARTESIAN_POINT('Ctrl Pts',(-62.0662277789053,-119.40082839455,174.143187956559));
#37979=CARTESIAN_POINT('Ctrl Pts',(-61.3173611118114,-119.574943812919,
173.162459923011));
#37980=CARTESIAN_POINT('Ctrl Pts',(-60.1011711786143,-119.798879013591,
173.008576811287));
#37981=CARTESIAN_POINT('Ctrl Pts',(-58.8849812454172,-120.022814214264,
172.854693699562));
#37982=CARTESIAN_POINT('Ctrl Pts',(-57.9197171970352,-120.219999039206,
173.617798149489));
#37983=CARTESIAN_POINT('Ctrl Pts',(-56.9544531486532,-120.417183864148,
174.380902599416));
#37984=CARTESIAN_POINT('Ctrl Pts',(-56.8113751558304,-120.526718162629,
175.613978373734));
#37985=CARTESIAN_POINT('Ctrl Pts',(-56.6682971630076,-120.63625246111,176.847054148052));
#37986=CARTESIAN_POINT('Ctrl Pts',(-57.4370399559356,-120.648580572052,
177.8277821816));
#37987=CARTESIAN_POINT('Ctrl Pts',(-58.2057827488635,-120.660908682994,
178.808510215148));
#37988=CARTESIAN_POINT('Ctrl Pts',(-59.4418488078947,-120.623417011633,
178.962393326872));
#37989=CARTESIAN_POINT('Ctrl Pts',(-60.6779148669258,-120.585925340271,
179.116276438596));
#37990=CARTESIAN_POINT('Ctrl Pts',(-61.6630550411418,-120.575184044639,
178.35317198867));
#37991=CARTESIAN_POINT('Ctrl Pts',(-62.6481952153579,-120.564442749008,
177.590067538743));
#37992=CARTESIAN_POINT('Ctrl Pts',(-62.8111493340147,-120.641351979837,
176.356991764425));
#37993=CARTESIAN_POINT('Ctrl Pts',(-62.9741034526715,-120.718261210667,
175.123915990107));
#37994=CARTESIAN_POINT('Ctrl Pts',(-62.2252367855776,-120.892376629035,
174.143187956559));
#37995=CARTESIAN_POINT('Ctrl Pts',(-61.4763701184836,-121.066492047404,
173.162459923011));
#37996=CARTESIAN_POINT('Ctrl Pts',(-60.2601801852865,-121.290427248077,
173.008576811287));
#37997=CARTESIAN_POINT('Ctrl Pts',(-59.0439902520894,-121.514362448749,
172.854693699562));
#37998=CARTESIAN_POINT('Ctrl Pts',(-58.0787262037074,-121.711547273691,
173.617798149489));
#37999=CARTESIAN_POINT('Ctrl Pts',(-57.1134621553254,-121.908732098633,
174.380902599416));
#38000=CARTESIAN_POINT('Ctrl Pts',(-56.9703841625026,-122.018266397115,
175.613978373734));
#38001=CARTESIAN_POINT('Ctrl Pts',(-56.8273061696798,-122.127800695596,
176.847054148052));
#38002=CARTESIAN_POINT('Ctrl Pts',(-57.5960489626078,-122.140128806538,
177.8277821816));
#38003=CARTESIAN_POINT('Ctrl Pts',(-58.3647917555358,-122.15245691748,178.808510215148));
#38004=CARTESIAN_POINT('Ctrl Pts',(-59.6008578145669,-122.114965246118,
178.962393326872));
#38005=CARTESIAN_POINT('Ctrl Pts',(-60.836923873598,-122.077473574756,179.116276438596));
#38006=CARTESIAN_POINT('Ctrl Pts',(-61.8220640478141,-122.066732279125,
178.35317198867));
#38007=CARTESIAN_POINT('Ctrl Pts',(-62.8072042220301,-122.055990983494,
177.590067538743));
#38008=CARTESIAN_POINT('Ctrl Pts',(-62.9701583406869,-122.132900214323,
176.356991764425));
#38009=CARTESIAN_POINT('Ctrl Pts',(-63.1331124593437,-122.209809445152,
175.123915990107));
#38010=CARTESIAN_POINT('Ctrl Pts',(-62.3842457922498,-122.383924863521,
174.143187956559));
#38011=CARTESIAN_POINT('Ctrl Pts',(-61.6353791251559,-122.55804028189,173.162459923011));
#38012=CARTESIAN_POINT('Ctrl Pts',(-60.4191891919588,-122.781975482562,
173.008576811287));
#38013=CARTESIAN_POINT('Ctrl Pts',(-59.2029992587616,-123.005910683235,
172.854693699562));
#38014=CARTESIAN_POINT('Ctrl Pts',(-58.2377352103796,-123.203095508177,
173.617798149489));
#38015=CARTESIAN_POINT('Ctrl Pts',(-57.2724711619977,-123.400280333119,
174.380902599416));
#38016=CARTESIAN_POINT('Ctrl Pts',(-57.1293931691749,-123.5098146316,175.613978373734));
#38017=CARTESIAN_POINT('Ctrl Pts',(-56.9863151763521,-123.619348930082,
176.847054148052));
#38018=CARTESIAN_POINT('Ctrl Pts',(-57.75505796928,-123.631677041024,177.8277821816));
#38019=CARTESIAN_POINT('Ctrl Pts',(-58.523800762208,-123.644005151966,178.808510215148));
#38020=CARTESIAN_POINT('Ctrl Pts',(-59.7598668212391,-123.606513480604,
178.962393326872));
#38021=CARTESIAN_POINT('Ctrl Pts',(-60.9959328802703,-123.569021809242,
179.116276438596));
#38022=CARTESIAN_POINT('Ctrl Pts',(-61.9810730544863,-123.55828051361,178.35317198867));
#38023=CARTESIAN_POINT('Ctrl Pts',(-62.9662132287023,-123.547539217979,
177.590067538743));
#38024=CARTESIAN_POINT('Ctrl Pts',(-63.1291673473591,-123.624448448809,
176.356991764425));
#38025=CARTESIAN_POINT('Ctrl Pts',(-63.292121466016,-123.701357679638,175.123915990107));
#38026=CARTESIAN_POINT('Ctrl Pts',(-62.543254798922,-123.875473098007,174.143187956559));
#38027=CARTESIAN_POINT('Ctrl Pts',(-61.7943881318281,-124.049588516375,
173.162459923011));
#38028=CARTESIAN_POINT('Ctrl Pts',(-60.578198198631,-124.273523717048,173.008576811287));
#38029=CARTESIAN_POINT('Ctrl Pts',(-59.3620082654339,-124.497458917721,
172.854693699562));
#38030=CARTESIAN_POINT('Ctrl Pts',(-58.3967442170519,-124.694643742663,
173.617798149489));
#38031=CARTESIAN_POINT('Ctrl Pts',(-57.4314801686699,-124.891828567605,
174.380902599416));
#38032=CARTESIAN_POINT('Ctrl Pts',(-57.2884021758471,-125.001362866086,
175.613978373734));
#38033=CARTESIAN_POINT('Ctrl Pts',(-57.1453241830243,-125.110897164567,
176.847054148052));
#38034=CARTESIAN_POINT('Ctrl Pts',(-57.9140669759523,-125.123225275509,
177.8277821816));
#38035=CARTESIAN_POINT('Ctrl Pts',(-58.6828097688802,-125.135553386451,
178.808510215148));
#38036=CARTESIAN_POINT('Ctrl Pts',(-59.9188758279114,-125.098061715089,
178.962393326872));
#38037=CARTESIAN_POINT('Ctrl Pts',(-61.1549418869425,-125.060570043727,
179.116276438596));
#38038=CARTESIAN_POINT('Ctrl Pts',(-62.1400820611585,-125.049828748096,
178.35317198867));
#38039=CARTESIAN_POINT('Ctrl Pts',(-63.1252222353745,-125.039087452465,
177.590067538743));
#38040=CARTESIAN_POINT('Ctrl Pts',(-63.2881763540314,-125.115996683294,
176.356991764425));
#38041=CARTESIAN_POINT('Ctrl Pts',(-63.4511304726882,-125.192905914124,
175.123915990107));
#38042=CARTESIAN_POINT('Ctrl Pts',(-62.7022638055942,-125.367021332492,
174.143187956559));
#38043=CARTESIAN_POINT('Ctrl Pts',(-61.9533971385003,-125.541136750861,
173.162459923011));
#38044=CARTESIAN_POINT('Ctrl Pts',(-60.7372072053032,-125.765071951534,
173.008576811287));
#38045=CARTESIAN_POINT('Ctrl Pts',(-59.5210172721061,-125.989007152206,
172.854693699562));
#38046=CARTESIAN_POINT('Ctrl Pts',(-58.5557532237241,-126.186191977148,
173.617798149489));
#38047=CARTESIAN_POINT('Ctrl Pts',(-57.5904891753421,-126.38337680209,174.380902599416));
#38048=CARTESIAN_POINT('Ctrl Pts',(-57.4474111825193,-126.492911100572,
175.613978373734));
#38049=CARTESIAN_POINT('Ctrl Pts',(-57.3043331896965,-126.602445399053,
176.847054148052));
#38050=CARTESIAN_POINT('Ctrl Pts',(-58.0730759826245,-126.614773509995,
177.8277821816));
#38051=CARTESIAN_POINT('Ctrl Pts',(-58.8418187755524,-126.627101620937,
178.808510215148));
#38052=CARTESIAN_POINT('Ctrl Pts',(-60.0778848345836,-126.589609949575,
178.962393326872));
#38053=CARTESIAN_POINT('Ctrl Pts',(-61.3139508936147,-126.552118278213,
179.116276438596));
#38054=CARTESIAN_POINT('Ctrl Pts',(-62.2990910678308,-126.541376982582,
178.35317198867));
#38055=CARTESIAN_POINT('Ctrl Pts',(-63.2842312420468,-126.53063568695,177.590067538743));
#38056=CARTESIAN_POINT('Ctrl Pts',(-63.4471853607036,-126.60754491778,176.356991764425));
#38057=CARTESIAN_POINT('Ctrl Pts',(-63.6101394793604,-126.684454148609,
175.123915990107));
#38058=CARTESIAN_POINT('Ctrl Pts',(-62.8612728122665,-126.858569566978,
174.143187956559));
#38059=CARTESIAN_POINT('Ctrl Pts',(-62.1124061451725,-127.032684985347,
173.162459923011));
#38060=CARTESIAN_POINT('Ctrl Pts',(-60.8962162119754,-127.256620186019,
173.008576811287));
#38061=CARTESIAN_POINT('Ctrl Pts',(-59.6800262787783,-127.480555386692,
172.854693699562));
#38062=CARTESIAN_POINT('Ctrl Pts',(-58.7147622303963,-127.677740211634,
173.617798149489));
#38063=CARTESIAN_POINT('Ctrl Pts',(-57.7494981820143,-127.874925036576,
174.380902599416));
#38064=CARTESIAN_POINT('Ctrl Pts',(-57.6064201891915,-127.984459335057,
175.613978373734));
#38065=CARTESIAN_POINT('Ctrl Pts',(-57.4633421963688,-128.093993633538,
176.847054148052));
#38066=CARTESIAN_POINT('Ctrl Pts',(-58.2320849892967,-128.10632174448,177.8277821816));
#38067=CARTESIAN_POINT('Ctrl Pts',(-59.0008277822247,-128.118649855422,
178.808510215148));
#38068=CARTESIAN_POINT('Ctrl Pts',(-60.2368938412558,-128.081158184061,
178.962393326872));
#38069=CARTESIAN_POINT('Ctrl Pts',(-61.472959900287,-128.043666512699,179.116276438596));
#38070=CARTESIAN_POINT('Ctrl Pts',(-62.458100074503,-128.032925217067,178.35317198867));
#38071=CARTESIAN_POINT('Ctrl Pts',(-63.443240248719,-128.022183921436,177.590067538743));
#38072=CARTESIAN_POINT('Ctrl Pts',(-63.6061943673758,-128.099093152265,
176.356991764425));
#38073=CARTESIAN_POINT('Ctrl Pts',(-63.7691484860326,-128.176002383095,
175.123915990107));
#38074=CARTESIAN_POINT('Ctrl Pts',(-63.0202818189387,-128.350117801463,
174.143187956559));
#38075=CARTESIAN_POINT('Ctrl Pts',(-62.2714151518448,-128.524233219832,
173.162459923011));
#38076=CARTESIAN_POINT('Ctrl Pts',(-61.0552252186477,-128.748168420505,
173.008576811287));
#38077=CARTESIAN_POINT('Ctrl Pts',(-59.8390352854505,-128.972103621177,
172.854693699562));
#38078=CARTESIAN_POINT('Ctrl Pts',(-58.8737712370686,-129.169288446119,
173.617798149489));
#38079=CARTESIAN_POINT('Ctrl Pts',(-57.9085071886866,-129.366473271061,
174.380902599416));
#38080=CARTESIAN_POINT('Ctrl Pts',(-57.7654291958638,-129.476007569543,
175.613978373734));
#38081=CARTESIAN_POINT('Ctrl Pts',(-57.622351203041,-129.585541868024,176.847054148052));
#38082=CARTESIAN_POINT('Ctrl Pts',(-58.3910939959689,-129.597869978966,
177.8277821816));
#38083=CARTESIAN_POINT('Ctrl Pts',(-59.1598367888969,-129.610198089908,
178.808510215148));
#38084=CARTESIAN_POINT('Ctrl Pts',(-60.395902847928,-129.572706418546,178.962393326872));
#38085=CARTESIAN_POINT('Ctrl Pts',(-61.6319689069592,-129.535214747184,
179.116276438596));
#38086=CARTESIAN_POINT('Ctrl Pts',(-62.6171090811752,-129.524473451553,
178.35317198867));
#38087=CARTESIAN_POINT('Ctrl Pts',(-63.6022492553912,-129.513732155922,
177.590067538743));
#38088=CARTESIAN_POINT('Ctrl Pts',(-63.765203374048,-129.590641386751,176.356991764425));
#38089=CARTESIAN_POINT('Ctrl Pts',(-63.9281574927048,-129.66755061758,175.123915990107));
#38090=CARTESIAN_POINT('Ctrl Pts',(-63.1792908256109,-129.841666035949,
174.143187956559));
#38091=CARTESIAN_POINT('Ctrl Pts',(-62.430424158517,-130.015781454318,173.162459923011));
#38092=CARTESIAN_POINT('Ctrl Pts',(-61.2142342253199,-130.23971665499,173.008576811287));
#38093=CARTESIAN_POINT('Ctrl Pts',(-59.9980442921228,-130.463651855663,
172.854693699562));
#38094=CARTESIAN_POINT('Ctrl Pts',(-59.0327802437408,-130.660836680605,
173.617798149489));
#38095=CARTESIAN_POINT('Ctrl Pts',(-58.0675161953588,-130.858021505547,
174.380902599416));
#38096=CARTESIAN_POINT('Ctrl Pts',(-57.924438202536,-130.967555804028,175.613978373734));
#38097=CARTESIAN_POINT('Ctrl Pts',(-57.7813602097132,-131.07709010251,176.847054148052));
#38098=CARTESIAN_POINT('Ctrl Pts',(-58.5501030026412,-131.089418213452,
177.8277821816));
#38099=CARTESIAN_POINT('Ctrl Pts',(-59.3188457955691,-131.101746324394,
178.808510215148));
#38100=CARTESIAN_POINT('Ctrl Pts',(-60.5549118546003,-131.064254653032,
178.962393326872));
#38101=CARTESIAN_POINT('Ctrl Pts',(-61.3544752486066,-131.040002738838,
179.061934368543));
#38102=CARTESIAN_POINT('Ctrl Pts',(-62.0977450155935,-131.026212373353,
178.749339314461));
#38103=CARTESIAN_POINT('Ctrl Pts',(-65.9070979972576,-130.955534979744,
177.14724952928));
#38104=CARTESIAN_POINT('Ctrl Pts',(-69.7164509789216,-130.884857586135,
175.545159744099));
#38105=CARTESIAN_POINT('Ctrl Pts',(-50.1268408042676,-67.1847631435675,
175.490142808619));
#38106=CARTESIAN_POINT('Ctrl Pts',(-49.9327574595315,-67.2997349533242,
177.134243841043));
#38107=CARTESIAN_POINT('Ctrl Pts',(-50.9544351624631,-67.2850985130284,
178.441881219107));
#38108=CARTESIAN_POINT('Ctrl Pts',(-51.9761128653947,-67.2704620727326,
179.74951859717));
#38109=CARTESIAN_POINT('Ctrl Pts',(-53.6208882564639,-67.1893992560316,
179.954696079469));
#38110=CARTESIAN_POINT('Ctrl Pts',(-55.2656636475331,-67.1083364393306,
180.159873561769));
#38111=CARTESIAN_POINT('Ctrl Pts',(-56.5758711921821,-67.0629407902703,
179.142400961866));
#38112=CARTESIAN_POINT('Ctrl Pts',(-57.8860787368312,-67.0175451412101,
178.124928361964));
#38113=CARTESIAN_POINT('Ctrl Pts',(-58.1000382074012,-67.0890168607642,
176.48082732954));
#38114=CARTESIAN_POINT('Ctrl Pts',(-58.3139976779713,-67.1604885803183,
174.836726297116));
#38115=CARTESIAN_POINT('Ctrl Pts',(-57.3121961008737,-67.3615685499248,
173.529088919052));
#38116=CARTESIAN_POINT('Ctrl Pts',(-56.3103945237762,-67.5626485195312,
172.221451540989));
#38117=CARTESIAN_POINT('Ctrl Pts',(-54.685495258541,-67.830154865543,172.016274058689));
#38118=CARTESIAN_POINT('Ctrl Pts',(-53.0605959933058,-68.0976612115547,
171.81109657639));
#38119=CARTESIAN_POINT('Ctrl Pts',(-51.7702645744908,-68.3295003899256,
172.828569176292));
#38120=CARTESIAN_POINT('Ctrl Pts',(-50.4799331556759,-68.5613395682965,
173.846041776195));
#38121=CARTESIAN_POINT('Ctrl Pts',(-50.2858498109398,-68.6763113780532,
175.490142808619));
#38122=CARTESIAN_POINT('Ctrl Pts',(-50.0917664662038,-68.7912831878098,
177.134243841043));
#38123=CARTESIAN_POINT('Ctrl Pts',(-51.1134441691353,-68.776646747514,178.441881219107));
#38124=CARTESIAN_POINT('Ctrl Pts',(-52.1351218720669,-68.7620103072182,
179.74951859717));
#38125=CARTESIAN_POINT('Ctrl Pts',(-53.7798972631361,-68.6809474905172,
179.954696079469));
#38126=CARTESIAN_POINT('Ctrl Pts',(-55.4246726542053,-68.5998846738162,
180.159873561769));
#38127=CARTESIAN_POINT('Ctrl Pts',(-56.7348801988543,-68.5544890247559,
179.142400961866));
#38128=CARTESIAN_POINT('Ctrl Pts',(-58.0450877435034,-68.5090933756957,
178.124928361964));
#38129=CARTESIAN_POINT('Ctrl Pts',(-58.2590472140735,-68.5805650952498,
176.48082732954));
#38130=CARTESIAN_POINT('Ctrl Pts',(-58.4730066846436,-68.6520368148039,
174.836726297116));
#38131=CARTESIAN_POINT('Ctrl Pts',(-57.471205107546,-68.8531167844104,173.529088919052));
#38132=CARTESIAN_POINT('Ctrl Pts',(-56.4694035304484,-69.0541967540168,
172.221451540989));
#38133=CARTESIAN_POINT('Ctrl Pts',(-54.8445042652132,-69.3217031000286,
172.016274058689));
#38134=CARTESIAN_POINT('Ctrl Pts',(-53.2196049999781,-69.5892094460403,
171.81109657639));
#38135=CARTESIAN_POINT('Ctrl Pts',(-51.9292735811631,-69.8210486244112,
172.828569176292));
#38136=CARTESIAN_POINT('Ctrl Pts',(-50.6389421623481,-70.0528878027821,
173.846041776195));
#38137=CARTESIAN_POINT('Ctrl Pts',(-50.444858817612,-70.1678596125387,175.490142808619));
#38138=CARTESIAN_POINT('Ctrl Pts',(-50.250775472876,-70.2828314222954,177.134243841043));
#38139=CARTESIAN_POINT('Ctrl Pts',(-51.2724531758076,-70.2681949819996,
178.441881219107));
#38140=CARTESIAN_POINT('Ctrl Pts',(-52.2941308787392,-70.2535585417038,
179.74951859717));
#38141=CARTESIAN_POINT('Ctrl Pts',(-53.9389062698084,-70.1724957250028,
179.954696079469));
#38142=CARTESIAN_POINT('Ctrl Pts',(-55.5836816608776,-70.0914329083018,
180.159873561769));
#38143=CARTESIAN_POINT('Ctrl Pts',(-56.8938892055266,-70.0460372592415,
179.142400961866));
#38144=CARTESIAN_POINT('Ctrl Pts',(-58.2040967501756,-70.0006416101813,
178.124928361964));
#38145=CARTESIAN_POINT('Ctrl Pts',(-58.4180562207457,-70.0721133297354,
176.48082732954));
#38146=CARTESIAN_POINT('Ctrl Pts',(-58.6320156913158,-70.1435850492895,
174.836726297116));
#38147=CARTESIAN_POINT('Ctrl Pts',(-57.6302141142182,-70.344665018896,173.529088919052));
#38148=CARTESIAN_POINT('Ctrl Pts',(-56.6284125371206,-70.5457449885024,
172.221451540989));
#38149=CARTESIAN_POINT('Ctrl Pts',(-55.0035132718855,-70.8132513345142,
172.016274058689));
#38150=CARTESIAN_POINT('Ctrl Pts',(-53.3786140066503,-71.0807576805259,
171.81109657639));
#38151=CARTESIAN_POINT('Ctrl Pts',(-52.0882825878353,-71.3125968588968,
172.828569176292));
#38152=CARTESIAN_POINT('Ctrl Pts',(-50.7979511690203,-71.5444360372677,
173.846041776195));
#38153=CARTESIAN_POINT('Ctrl Pts',(-50.6038678242842,-71.6594078470244,
175.490142808619));
#38154=CARTESIAN_POINT('Ctrl Pts',(-50.4097844795482,-71.774379656781,177.134243841043));
#38155=CARTESIAN_POINT('Ctrl Pts',(-51.4314621824798,-71.7597432164852,
178.441881219107));
#38156=CARTESIAN_POINT('Ctrl Pts',(-52.4531398854114,-71.7451067761894,
179.74951859717));
#38157=CARTESIAN_POINT('Ctrl Pts',(-54.0979152764806,-71.6640439594884,
179.954696079469));
#38158=CARTESIAN_POINT('Ctrl Pts',(-55.7426906675498,-71.5829811427874,
180.159873561769));
#38159=CARTESIAN_POINT('Ctrl Pts',(-57.0528982121988,-71.5375854937271,
179.142400961866));
#38160=CARTESIAN_POINT('Ctrl Pts',(-58.3631057568478,-71.4921898446669,
178.124928361964));
#38161=CARTESIAN_POINT('Ctrl Pts',(-58.5770652274179,-71.563661564221,176.48082732954));
#38162=CARTESIAN_POINT('Ctrl Pts',(-58.791024697988,-71.6351332837751,174.836726297116));
#38163=CARTESIAN_POINT('Ctrl Pts',(-57.7892231208904,-71.8362132533815,
173.529088919052));
#38164=CARTESIAN_POINT('Ctrl Pts',(-56.7874215437928,-72.037293222988,172.221451540989));
#38165=CARTESIAN_POINT('Ctrl Pts',(-55.1625222785577,-72.3047995689997,
172.016274058689));
#38166=CARTESIAN_POINT('Ctrl Pts',(-53.5376230133225,-72.5723059150115,
171.81109657639));
#38167=CARTESIAN_POINT('Ctrl Pts',(-52.2472915945075,-72.8041450933824,
172.828569176292));
#38168=CARTESIAN_POINT('Ctrl Pts',(-50.9569601756925,-73.0359842717533,
173.846041776195));
#38169=CARTESIAN_POINT('Ctrl Pts',(-50.7628768309565,-73.1509560815099,
175.490142808619));
#38170=CARTESIAN_POINT('Ctrl Pts',(-50.5687934862204,-73.2659278912666,
177.134243841043));
#38171=CARTESIAN_POINT('Ctrl Pts',(-51.590471189152,-73.2512914509708,178.441881219107));
#38172=CARTESIAN_POINT('Ctrl Pts',(-52.6121488920836,-73.236655010675,179.74951859717));
#38173=CARTESIAN_POINT('Ctrl Pts',(-54.2569242831528,-73.155592193974,179.954696079469));
#38174=CARTESIAN_POINT('Ctrl Pts',(-55.901699674222,-73.074529377273,180.159873561769));
#38175=CARTESIAN_POINT('Ctrl Pts',(-57.211907218871,-73.0291337282128,179.142400961866));
#38176=CARTESIAN_POINT('Ctrl Pts',(-58.5221147635201,-72.9837380791525,
178.124928361964));
#38177=CARTESIAN_POINT('Ctrl Pts',(-58.7360742340901,-73.0552097987066,
176.48082732954));
#38178=CARTESIAN_POINT('Ctrl Pts',(-58.9500337046602,-73.1266815182607,
174.836726297116));
#38179=CARTESIAN_POINT('Ctrl Pts',(-57.9482321275626,-73.3277614878671,
173.529088919052));
#38180=CARTESIAN_POINT('Ctrl Pts',(-56.9464305504651,-73.5288414574736,
172.221451540989));
#38181=CARTESIAN_POINT('Ctrl Pts',(-55.3215312852299,-73.7963478034854,
172.016274058689));
#38182=CARTESIAN_POINT('Ctrl Pts',(-53.6966320199948,-74.0638541494971,
171.81109657639));
#38183=CARTESIAN_POINT('Ctrl Pts',(-52.4063006011798,-74.295693327868,172.828569176292));
#38184=CARTESIAN_POINT('Ctrl Pts',(-51.1159691823648,-74.5275325062389,
173.846041776195));
#38185=CARTESIAN_POINT('Ctrl Pts',(-50.9218858376287,-74.6425043159955,
175.490142808619));
#38186=CARTESIAN_POINT('Ctrl Pts',(-50.7278024928926,-74.7574761257522,
177.134243841043));
#38187=CARTESIAN_POINT('Ctrl Pts',(-51.7494801958242,-74.7428396854564,
178.441881219107));
#38188=CARTESIAN_POINT('Ctrl Pts',(-52.7711578987558,-74.7282032451606,
179.74951859717));
#38189=CARTESIAN_POINT('Ctrl Pts',(-54.415933289825,-74.6471404284596,179.954696079469));
#38190=CARTESIAN_POINT('Ctrl Pts',(-56.0607086808942,-74.5660776117586,
180.159873561769));
#38191=CARTESIAN_POINT('Ctrl Pts',(-57.3709162255433,-74.5206819626983,
179.142400961866));
#38192=CARTESIAN_POINT('Ctrl Pts',(-58.6811237701923,-74.4752863136381,
178.124928361964));
#38193=CARTESIAN_POINT('Ctrl Pts',(-58.8950832407624,-74.5467580331922,
176.48082732954));
#38194=CARTESIAN_POINT('Ctrl Pts',(-59.1090427113324,-74.6182297527463,
174.836726297116));
#38195=CARTESIAN_POINT('Ctrl Pts',(-58.1072411342349,-74.8193097223528,
173.529088919052));
#38196=CARTESIAN_POINT('Ctrl Pts',(-57.1054395571373,-75.0203896919592,
172.221451540989));
#38197=CARTESIAN_POINT('Ctrl Pts',(-55.4805402919021,-75.287896037971,172.016274058689));
#38198=CARTESIAN_POINT('Ctrl Pts',(-53.855641026667,-75.5554023839827,171.81109657639));
#38199=CARTESIAN_POINT('Ctrl Pts',(-52.565309607852,-75.7872415623536,172.828569176292));
#38200=CARTESIAN_POINT('Ctrl Pts',(-51.274978189037,-76.0190807407245,173.846041776195));
#38201=CARTESIAN_POINT('Ctrl Pts',(-51.0808948443009,-76.1340525504811,
175.490142808619));
#38202=CARTESIAN_POINT('Ctrl Pts',(-50.8868114995649,-76.2490243602377,
177.134243841043));
#38203=CARTESIAN_POINT('Ctrl Pts',(-51.9084892024965,-76.234387919942,178.441881219107));
#38204=CARTESIAN_POINT('Ctrl Pts',(-52.9301669054281,-76.2197514796462,
179.74951859717));
#38205=CARTESIAN_POINT('Ctrl Pts',(-54.5749422964973,-76.1386886629452,
179.954696079469));
#38206=CARTESIAN_POINT('Ctrl Pts',(-56.2197176875665,-76.0576258462442,
180.159873561769));
#38207=CARTESIAN_POINT('Ctrl Pts',(-57.5299252322155,-76.012230197184,179.142400961866));
#38208=CARTESIAN_POINT('Ctrl Pts',(-58.8401327768645,-75.9668345481237,
178.124928361964));
#38209=CARTESIAN_POINT('Ctrl Pts',(-59.0540922474346,-76.0383062676778,
176.48082732954));
#38210=CARTESIAN_POINT('Ctrl Pts',(-59.2680517180047,-76.1097779872319,
174.836726297116));
#38211=CARTESIAN_POINT('Ctrl Pts',(-58.2662501409071,-76.3108579568383,
173.529088919052));
#38212=CARTESIAN_POINT('Ctrl Pts',(-57.2644485638095,-76.5119379264448,
172.221451540989));
#38213=CARTESIAN_POINT('Ctrl Pts',(-55.6395492985744,-76.7794442724566,
172.016274058689));
#38214=CARTESIAN_POINT('Ctrl Pts',(-54.0146500333392,-77.0469506184683,
171.81109657639));
#38215=CARTESIAN_POINT('Ctrl Pts',(-52.7243186145242,-77.2787897968392,
172.828569176292));
#38216=CARTESIAN_POINT('Ctrl Pts',(-51.4339871957092,-77.5106289752101,
173.846041776195));
#38217=CARTESIAN_POINT('Ctrl Pts',(-51.2399038509732,-77.6256007849667,
175.490142808619));
#38218=CARTESIAN_POINT('Ctrl Pts',(-51.0458205062371,-77.7405725947234,
177.134243841043));
#38219=CARTESIAN_POINT('Ctrl Pts',(-52.0674982091687,-77.7259361544276,
178.441881219107));
#38220=CARTESIAN_POINT('Ctrl Pts',(-53.0891759121003,-77.7112997141318,
179.74951859717));
#38221=CARTESIAN_POINT('Ctrl Pts',(-54.7339513031695,-77.6302368974308,
179.954696079469));
#38222=CARTESIAN_POINT('Ctrl Pts',(-56.3787266942387,-77.5491740807298,
180.159873561769));
#38223=CARTESIAN_POINT('Ctrl Pts',(-57.6889342388877,-77.5037784316696,
179.142400961866));
#38224=CARTESIAN_POINT('Ctrl Pts',(-58.9991417835367,-77.4583827826093,
178.124928361964));
#38225=CARTESIAN_POINT('Ctrl Pts',(-59.2131012541068,-77.5298545021634,
176.48082732954));
#38226=CARTESIAN_POINT('Ctrl Pts',(-59.4270607246769,-77.6013262217175,
174.836726297116));
#38227=CARTESIAN_POINT('Ctrl Pts',(-58.4252591475793,-77.802406191324,173.529088919052));
#38228=CARTESIAN_POINT('Ctrl Pts',(-57.4234575704818,-78.0034861609304,
172.221451540989));
#38229=CARTESIAN_POINT('Ctrl Pts',(-55.7985583052466,-78.2709925069422,
172.016274058689));
#38230=CARTESIAN_POINT('Ctrl Pts',(-54.1736590400114,-78.5384988529539,
171.81109657639));
#38231=CARTESIAN_POINT('Ctrl Pts',(-52.8833276211964,-78.7703380313248,
172.828569176292));
#38232=CARTESIAN_POINT('Ctrl Pts',(-51.5929962023814,-79.0021772096957,
173.846041776195));
#38233=CARTESIAN_POINT('Ctrl Pts',(-51.3989128576454,-79.1171490194523,
175.490142808619));
#38234=CARTESIAN_POINT('Ctrl Pts',(-51.2048295129093,-79.232120829209,177.134243841043));
#38235=CARTESIAN_POINT('Ctrl Pts',(-52.2265072158409,-79.2174843889132,
178.441881219107));
#38236=CARTESIAN_POINT('Ctrl Pts',(-53.2481849187725,-79.2028479486174,
179.74951859717));
#38237=CARTESIAN_POINT('Ctrl Pts',(-54.8929603098417,-79.1217851319164,
179.954696079469));
#38238=CARTESIAN_POINT('Ctrl Pts',(-56.5377357009109,-79.0407223152154,
180.159873561769));
#38239=CARTESIAN_POINT('Ctrl Pts',(-57.8479432455599,-78.9953266661552,
179.142400961866));
#38240=CARTESIAN_POINT('Ctrl Pts',(-59.158150790209,-78.9499310170949,178.124928361964));
#38241=CARTESIAN_POINT('Ctrl Pts',(-59.372110260779,-79.021402736649,176.48082732954));
#38242=CARTESIAN_POINT('Ctrl Pts',(-59.5860697313491,-79.0928744562031,
174.836726297116));
#38243=CARTESIAN_POINT('Ctrl Pts',(-58.5842681542516,-79.2939544258096,
173.529088919052));
#38244=CARTESIAN_POINT('Ctrl Pts',(-57.582466577154,-79.495034395416,172.221451540989));
#38245=CARTESIAN_POINT('Ctrl Pts',(-55.9575673119188,-79.7625407414277,
172.016274058689));
#38246=CARTESIAN_POINT('Ctrl Pts',(-54.3326680466837,-80.0300470874395,
171.81109657639));
#38247=CARTESIAN_POINT('Ctrl Pts',(-53.0423366278687,-80.2618862658104,
172.828569176292));
#38248=CARTESIAN_POINT('Ctrl Pts',(-51.7520052090537,-80.4937254441813,
173.846041776195));
#38249=CARTESIAN_POINT('Ctrl Pts',(-51.5579218643176,-80.6086972539379,
175.490142808619));
#38250=CARTESIAN_POINT('Ctrl Pts',(-51.3638385195816,-80.7236690636945,
177.134243841043));
#38251=CARTESIAN_POINT('Ctrl Pts',(-52.3855162225132,-80.7090326233988,
178.441881219107));
#38252=CARTESIAN_POINT('Ctrl Pts',(-53.4071939254448,-80.694396183103,179.74951859717));
#38253=CARTESIAN_POINT('Ctrl Pts',(-55.0519693165139,-80.613333366402,179.954696079469));
#38254=CARTESIAN_POINT('Ctrl Pts',(-56.6967447075831,-80.532270549701,180.159873561769));
#38255=CARTESIAN_POINT('Ctrl Pts',(-58.0069522522322,-80.4868749006407,
179.142400961866));
#38256=CARTESIAN_POINT('Ctrl Pts',(-59.3171597968812,-80.4414792515805,
178.124928361964));
#38257=CARTESIAN_POINT('Ctrl Pts',(-59.5311192674513,-80.5129509711346,
176.48082732954));
#38258=CARTESIAN_POINT('Ctrl Pts',(-59.7450787380214,-80.5844226906887,
174.836726297116));
#38259=CARTESIAN_POINT('Ctrl Pts',(-58.7432771609238,-80.7855026602952,
173.529088919052));
#38260=CARTESIAN_POINT('Ctrl Pts',(-57.7414755838262,-80.9865826299016,
172.221451540989));
#38261=CARTESIAN_POINT('Ctrl Pts',(-56.116576318591,-81.2540889759133,172.016274058689));
#38262=CARTESIAN_POINT('Ctrl Pts',(-54.4916770533559,-81.5215953219251,
171.81109657639));
#38263=CARTESIAN_POINT('Ctrl Pts',(-53.2013456345409,-81.753434500296,172.828569176292));
#38264=CARTESIAN_POINT('Ctrl Pts',(-51.9110142157259,-81.9852736786669,
173.846041776195));
#38265=CARTESIAN_POINT('Ctrl Pts',(-51.7169308709898,-82.1002454884235,
175.490142808619));
#38266=CARTESIAN_POINT('Ctrl Pts',(-51.5228475262538,-82.2152172981802,
177.134243841043));
#38267=CARTESIAN_POINT('Ctrl Pts',(-52.5445252291854,-82.2005808578844,
178.441881219107));
#38268=CARTESIAN_POINT('Ctrl Pts',(-53.566202932117,-82.1859444175886,179.74951859717));
#38269=CARTESIAN_POINT('Ctrl Pts',(-55.2109783231862,-82.1048816008876,
179.954696079469));
#38270=CARTESIAN_POINT('Ctrl Pts',(-56.8557537142554,-82.0238187841866,
180.159873561769));
#38271=CARTESIAN_POINT('Ctrl Pts',(-58.1659612589044,-81.9784231351264,
179.142400961866));
#38272=CARTESIAN_POINT('Ctrl Pts',(-59.4761688035534,-81.9330274860661,
178.124928361964));
#38273=CARTESIAN_POINT('Ctrl Pts',(-59.6901282741235,-82.0044992056202,
176.48082732954));
#38274=CARTESIAN_POINT('Ctrl Pts',(-59.9040877446936,-82.0759709251743,
174.836726297116));
#38275=CARTESIAN_POINT('Ctrl Pts',(-58.902286167596,-82.2770508947808,173.529088919052));
#38276=CARTESIAN_POINT('Ctrl Pts',(-57.9004845904984,-82.4781308643872,
172.221451540989));
#38277=CARTESIAN_POINT('Ctrl Pts',(-56.2755853252633,-82.745637210399,172.016274058689));
#38278=CARTESIAN_POINT('Ctrl Pts',(-54.6506860600281,-83.0131435564107,
171.81109657639));
#38279=CARTESIAN_POINT('Ctrl Pts',(-53.3603546412131,-83.2449827347816,
172.828569176292));
#38280=CARTESIAN_POINT('Ctrl Pts',(-52.0700232223981,-83.4768219131525,
173.846041776195));
#38281=CARTESIAN_POINT('Ctrl Pts',(-51.8759398776621,-83.5917937229092,
175.490142808619));
#38282=CARTESIAN_POINT('Ctrl Pts',(-51.681856532926,-83.7067655326658,177.134243841043));
#38283=CARTESIAN_POINT('Ctrl Pts',(-52.7035342358576,-83.69212909237,178.441881219107));
#38284=CARTESIAN_POINT('Ctrl Pts',(-53.7252119387892,-83.6774926520742,
179.74951859717));
#38285=CARTESIAN_POINT('Ctrl Pts',(-55.3699873298584,-83.5964298353732,
179.954696079469));
#38286=CARTESIAN_POINT('Ctrl Pts',(-57.0147627209276,-83.5153670186722,
180.159873561769));
#38287=CARTESIAN_POINT('Ctrl Pts',(-58.3249702655766,-83.469971369612,179.142400961866));
#38288=CARTESIAN_POINT('Ctrl Pts',(-59.6351778102256,-83.4245757205517,
178.124928361964));
#38289=CARTESIAN_POINT('Ctrl Pts',(-59.8491372807957,-83.4960474401058,
176.48082732954));
#38290=CARTESIAN_POINT('Ctrl Pts',(-60.0630967513658,-83.5675191596599,
174.836726297116));
#38291=CARTESIAN_POINT('Ctrl Pts',(-59.0612951742682,-83.7685991292663,
173.529088919052));
#38292=CARTESIAN_POINT('Ctrl Pts',(-58.0594935971707,-83.9696790988728,
172.221451540989));
#38293=CARTESIAN_POINT('Ctrl Pts',(-56.4345943319355,-84.2371854448845,
172.016274058689));
#38294=CARTESIAN_POINT('Ctrl Pts',(-54.8096950667003,-84.5046917908963,
171.81109657639));
#38295=CARTESIAN_POINT('Ctrl Pts',(-53.5193636478853,-84.7365309692672,
172.828569176292));
#38296=CARTESIAN_POINT('Ctrl Pts',(-52.2290322290704,-84.9683701476381,
173.846041776195));
#38297=CARTESIAN_POINT('Ctrl Pts',(-52.0349488843343,-85.0833419573947,
175.490142808619));
#38298=CARTESIAN_POINT('Ctrl Pts',(-51.8408655395982,-85.1983137671514,
177.134243841043));
#38299=CARTESIAN_POINT('Ctrl Pts',(-52.8625432425298,-85.1836773268556,
178.441881219107));
#38300=CARTESIAN_POINT('Ctrl Pts',(-53.8842209454614,-85.1690408865598,
179.74951859717));
#38301=CARTESIAN_POINT('Ctrl Pts',(-55.5289963365306,-85.0879780698588,
179.954696079469));
#38302=CARTESIAN_POINT('Ctrl Pts',(-57.1737717275998,-85.0069152531578,
180.159873561769));
#38303=CARTESIAN_POINT('Ctrl Pts',(-58.4839792722488,-84.9615196040975,
179.142400961866));
#38304=CARTESIAN_POINT('Ctrl Pts',(-59.7941868168979,-84.9161239550373,
178.124928361964));
#38305=CARTESIAN_POINT('Ctrl Pts',(-60.008146287468,-84.9875956745914,176.48082732954));
#38306=CARTESIAN_POINT('Ctrl Pts',(-60.222105758038,-85.0590673941455,174.836726297116));
#38307=CARTESIAN_POINT('Ctrl Pts',(-59.2203041809405,-85.260147363752,173.529088919052));
#38308=CARTESIAN_POINT('Ctrl Pts',(-58.2185026038429,-85.4612273333584,
172.221451540989));
#38309=CARTESIAN_POINT('Ctrl Pts',(-56.5936033386077,-85.7287336793702,
172.016274058689));
#38310=CARTESIAN_POINT('Ctrl Pts',(-54.9687040733726,-85.9962400253819,
171.81109657639));
#38311=CARTESIAN_POINT('Ctrl Pts',(-53.6783726545576,-86.2280792037528,
172.828569176292));
#38312=CARTESIAN_POINT('Ctrl Pts',(-52.3880412357426,-86.4599183821237,
173.846041776195));
#38313=CARTESIAN_POINT('Ctrl Pts',(-52.1939578910065,-86.5748901918803,
175.490142808619));
#38314=CARTESIAN_POINT('Ctrl Pts',(-51.9998745462705,-86.689862001637,177.134243841043));
#38315=CARTESIAN_POINT('Ctrl Pts',(-53.0215522492021,-86.6752255613412,
178.441881219107));
#38316=CARTESIAN_POINT('Ctrl Pts',(-54.0432299521337,-86.6605891210454,
179.74951859717));
#38317=CARTESIAN_POINT('Ctrl Pts',(-55.6880053432029,-86.5795263043444,
179.954696079469));
#38318=CARTESIAN_POINT('Ctrl Pts',(-57.332780734272,-86.4984634876434,180.159873561769));
#38319=CARTESIAN_POINT('Ctrl Pts',(-58.6429882789211,-86.4530678385832,
179.142400961866));
#38320=CARTESIAN_POINT('Ctrl Pts',(-59.9531958235701,-86.4076721895229,
178.124928361964));
#38321=CARTESIAN_POINT('Ctrl Pts',(-60.1671552941402,-86.479143909077,176.48082732954));
#38322=CARTESIAN_POINT('Ctrl Pts',(-60.3811147647103,-86.5506156286311,
174.836726297116));
#38323=CARTESIAN_POINT('Ctrl Pts',(-59.3793131876127,-86.7516955982376,
173.529088919052));
#38324=CARTESIAN_POINT('Ctrl Pts',(-58.3775116105151,-86.952775567844,172.221451540989));
#38325=CARTESIAN_POINT('Ctrl Pts',(-56.7526123452799,-87.2202819138558,
172.016274058689));
#38326=CARTESIAN_POINT('Ctrl Pts',(-55.1277130800448,-87.4877882598675,
171.81109657639));
#38327=CARTESIAN_POINT('Ctrl Pts',(-53.8373816612298,-87.7196274382384,
172.828569176292));
#38328=CARTESIAN_POINT('Ctrl Pts',(-52.5470502424148,-87.9514666166093,
173.846041776195));
#38329=CARTESIAN_POINT('Ctrl Pts',(-52.3529668976787,-88.0664384263659,
175.490142808619));
#38330=CARTESIAN_POINT('Ctrl Pts',(-52.1588835529427,-88.1814102361226,
177.134243841043));
#38331=CARTESIAN_POINT('Ctrl Pts',(-53.1805612558743,-88.1667737958268,
178.441881219107));
#38332=CARTESIAN_POINT('Ctrl Pts',(-54.2022389588059,-88.152137355531,179.74951859717));
#38333=CARTESIAN_POINT('Ctrl Pts',(-55.8470143498751,-88.07107453883,179.954696079469));
#38334=CARTESIAN_POINT('Ctrl Pts',(-57.4917897409443,-87.990011722129,180.159873561769));
#38335=CARTESIAN_POINT('Ctrl Pts',(-58.8019972855933,-87.9446160730687,
179.142400961866));
#38336=CARTESIAN_POINT('Ctrl Pts',(-60.1122048302423,-87.8992204240085,
178.124928361964));
#38337=CARTESIAN_POINT('Ctrl Pts',(-60.3261643008124,-87.9706921435626,
176.48082732954));
#38338=CARTESIAN_POINT('Ctrl Pts',(-60.5401237713825,-88.0421638631167,
174.836726297116));
#38339=CARTESIAN_POINT('Ctrl Pts',(-59.5383221942849,-88.2432438327232,
173.529088919052));
#38340=CARTESIAN_POINT('Ctrl Pts',(-58.5365206171873,-88.4443238023296,
172.221451540989));
#38341=CARTESIAN_POINT('Ctrl Pts',(-56.9116213519522,-88.7118301483414,
172.016274058689));
#38342=CARTESIAN_POINT('Ctrl Pts',(-55.286722086717,-88.9793364943531,171.81109657639));
#38343=CARTESIAN_POINT('Ctrl Pts',(-53.996390667902,-89.211175672724,172.828569176292));
#38344=CARTESIAN_POINT('Ctrl Pts',(-52.706059249087,-89.4430148510949,173.846041776195));
#38345=CARTESIAN_POINT('Ctrl Pts',(-52.511975904351,-89.5579866608516,175.490142808619));
#38346=CARTESIAN_POINT('Ctrl Pts',(-52.3178925596149,-89.6729584706082,
177.134243841043));
#38347=CARTESIAN_POINT('Ctrl Pts',(-53.3395702625465,-89.6583220303124,
178.441881219107));
#38348=CARTESIAN_POINT('Ctrl Pts',(-54.3612479654781,-89.6436855900166,
179.74951859717));
#38349=CARTESIAN_POINT('Ctrl Pts',(-56.0060233565473,-89.5626227733156,
179.954696079469));
#38350=CARTESIAN_POINT('Ctrl Pts',(-57.6507987476165,-89.4815599566146,
180.159873561769));
#38351=CARTESIAN_POINT('Ctrl Pts',(-58.9610062922655,-89.4361643075543,
179.142400961866));
#38352=CARTESIAN_POINT('Ctrl Pts',(-60.2712138369146,-89.3907686584941,
178.124928361964));
#38353=CARTESIAN_POINT('Ctrl Pts',(-60.4851733074846,-89.4622403780482,
176.48082732954));
#38354=CARTESIAN_POINT('Ctrl Pts',(-60.6991327780547,-89.5337120976023,
174.836726297116));
#38355=CARTESIAN_POINT('Ctrl Pts',(-59.6973312009571,-89.7347920672087,
173.529088919052));
#38356=CARTESIAN_POINT('Ctrl Pts',(-58.6955296238596,-89.9358720368152,
172.221451540989));
#38357=CARTESIAN_POINT('Ctrl Pts',(-57.0706303586244,-90.203378382827,172.016274058689));
#38358=CARTESIAN_POINT('Ctrl Pts',(-55.4457310933893,-90.4708847288387,
171.81109657639));
#38359=CARTESIAN_POINT('Ctrl Pts',(-54.1553996745743,-90.7027239072096,
172.828569176292));
#38360=CARTESIAN_POINT('Ctrl Pts',(-52.8650682557593,-90.9345630855805,
173.846041776195));
#38361=CARTESIAN_POINT('Ctrl Pts',(-52.6709849110232,-91.0495348953371,
175.490142808619));
#38362=CARTESIAN_POINT('Ctrl Pts',(-52.4769015662871,-91.1645067050937,
177.134243841043));
#38363=CARTESIAN_POINT('Ctrl Pts',(-53.4985792692187,-91.149870264798,178.441881219107));
#38364=CARTESIAN_POINT('Ctrl Pts',(-54.5202569721503,-91.1352338245022,
179.74951859717));
#38365=CARTESIAN_POINT('Ctrl Pts',(-56.1650323632195,-91.0541710078012,
179.954696079469));
#38366=CARTESIAN_POINT('Ctrl Pts',(-57.8098077542887,-90.9731081911002,
180.159873561769));
#38367=CARTESIAN_POINT('Ctrl Pts',(-59.1200152989378,-90.92771254204,179.142400961866));
#38368=CARTESIAN_POINT('Ctrl Pts',(-60.4302228435868,-90.8823168929797,
178.124928361964));
#38369=CARTESIAN_POINT('Ctrl Pts',(-60.6441823141569,-90.9537886125338,
176.48082732954));
#38370=CARTESIAN_POINT('Ctrl Pts',(-60.858141784727,-91.0252603320879,174.836726297116));
#38371=CARTESIAN_POINT('Ctrl Pts',(-59.8563402076294,-91.2263403016943,
173.529088919052));
#38372=CARTESIAN_POINT('Ctrl Pts',(-58.8545386305318,-91.4274202713008,
172.221451540989));
#38373=CARTESIAN_POINT('Ctrl Pts',(-57.2296393652966,-91.6949266173126,
172.016274058689));
#38374=CARTESIAN_POINT('Ctrl Pts',(-55.6047401000615,-91.9624329633243,
171.81109657639));
#38375=CARTESIAN_POINT('Ctrl Pts',(-54.3144086812465,-92.1942721416952,
172.828569176292));
#38376=CARTESIAN_POINT('Ctrl Pts',(-53.0240772624315,-92.4261113200661,
173.846041776195));
#38377=CARTESIAN_POINT('Ctrl Pts',(-52.8299939176954,-92.5410831298227,
175.490142808619));
#38378=CARTESIAN_POINT('Ctrl Pts',(-52.6359105729594,-92.6560549395794,
177.134243841043));
#38379=CARTESIAN_POINT('Ctrl Pts',(-53.657588275891,-92.6414184992836,178.441881219107));
#38380=CARTESIAN_POINT('Ctrl Pts',(-54.6792659788226,-92.6267820589878,
179.74951859717));
#38381=CARTESIAN_POINT('Ctrl Pts',(-56.3240413698918,-92.5457192422868,
179.954696079469));
#38382=CARTESIAN_POINT('Ctrl Pts',(-57.968816760961,-92.4646564255858,180.159873561769));
#38383=CARTESIAN_POINT('Ctrl Pts',(-59.27902430561,-92.4192607765256,179.142400961866));
#38384=CARTESIAN_POINT('Ctrl Pts',(-60.589231850259,-92.3738651274653,178.124928361964));
#38385=CARTESIAN_POINT('Ctrl Pts',(-60.8031913208291,-92.4453368470194,
176.48082732954));
#38386=CARTESIAN_POINT('Ctrl Pts',(-61.0171507913992,-92.5168085665735,
174.836726297116));
#38387=CARTESIAN_POINT('Ctrl Pts',(-60.0153492143016,-92.71788853618,173.529088919052));
#38388=CARTESIAN_POINT('Ctrl Pts',(-59.013547637204,-92.9189685057864,172.221451540989));
#38389=CARTESIAN_POINT('Ctrl Pts',(-57.3886483719689,-93.1864748517982,
172.016274058689));
#38390=CARTESIAN_POINT('Ctrl Pts',(-55.7637491067337,-93.4539811978099,
171.81109657639));
#38391=CARTESIAN_POINT('Ctrl Pts',(-54.4734176879187,-93.6858203761808,
172.828569176292));
#38392=CARTESIAN_POINT('Ctrl Pts',(-53.1830862691037,-93.9176595545517,
173.846041776195));
#38393=CARTESIAN_POINT('Ctrl Pts',(-52.9890029243677,-94.0326313643084,
175.490142808619));
#38394=CARTESIAN_POINT('Ctrl Pts',(-52.7949195796316,-94.147603174065,177.134243841043));
#38395=CARTESIAN_POINT('Ctrl Pts',(-53.8165972825632,-94.1329667337692,
178.441881219107));
#38396=CARTESIAN_POINT('Ctrl Pts',(-54.8382749854948,-94.1183302934734,
179.74951859717));
#38397=CARTESIAN_POINT('Ctrl Pts',(-56.483050376564,-94.0372674767724,179.954696079469));
#38398=CARTESIAN_POINT('Ctrl Pts',(-58.1278257676332,-93.9562046600714,
180.159873561769));
#38399=CARTESIAN_POINT('Ctrl Pts',(-59.4380333122822,-93.9108090110112,
179.142400961866));
#38400=CARTESIAN_POINT('Ctrl Pts',(-60.7482408569312,-93.8654133619509,
178.124928361964));
#38401=CARTESIAN_POINT('Ctrl Pts',(-60.9622003275013,-93.936885081505,176.48082732954));
#38402=CARTESIAN_POINT('Ctrl Pts',(-61.1761597980714,-94.0083568010591,
174.836726297116));
#38403=CARTESIAN_POINT('Ctrl Pts',(-60.1743582209738,-94.2094367706656,
173.529088919052));
#38404=CARTESIAN_POINT('Ctrl Pts',(-59.1725566438763,-94.410516740272,172.221451540989));
#38405=CARTESIAN_POINT('Ctrl Pts',(-57.5476573786411,-94.6780230862838,
172.016274058689));
#38406=CARTESIAN_POINT('Ctrl Pts',(-55.9227581134059,-94.9455294322955,
171.81109657639));
#38407=CARTESIAN_POINT('Ctrl Pts',(-54.6324266945909,-95.1773686106664,
172.828569176292));
#38408=CARTESIAN_POINT('Ctrl Pts',(-53.342095275776,-95.4092077890373,173.846041776195));
#38409=CARTESIAN_POINT('Ctrl Pts',(-53.1480119310399,-95.5241795987939,
175.490142808619));
#38410=CARTESIAN_POINT('Ctrl Pts',(-52.9539285863038,-95.6391514085506,
177.134243841043));
#38411=CARTESIAN_POINT('Ctrl Pts',(-53.9756062892354,-95.6245149682548,
178.441881219107));
#38412=CARTESIAN_POINT('Ctrl Pts',(-54.997283992167,-95.609878527959,179.74951859717));
#38413=CARTESIAN_POINT('Ctrl Pts',(-56.6420593832362,-95.528815711258,179.954696079469));
#38414=CARTESIAN_POINT('Ctrl Pts',(-58.2868347743054,-95.447752894557,180.159873561769));
#38415=CARTESIAN_POINT('Ctrl Pts',(-59.5970423189544,-95.4023572454968,
179.142400961866));
#38416=CARTESIAN_POINT('Ctrl Pts',(-60.9072498636035,-95.3569615964365,
178.124928361964));
#38417=CARTESIAN_POINT('Ctrl Pts',(-61.1212093341735,-95.4284333159906,
176.48082732954));
#38418=CARTESIAN_POINT('Ctrl Pts',(-61.3351688047436,-95.4999050355447,
174.836726297116));
#38419=CARTESIAN_POINT('Ctrl Pts',(-60.3333672276461,-95.7009850051512,
173.529088919052));
#38420=CARTESIAN_POINT('Ctrl Pts',(-59.3315656505485,-95.9020649747577,
172.221451540989));
#38421=CARTESIAN_POINT('Ctrl Pts',(-57.7066663853133,-96.1695713207694,
172.016274058689));
#38422=CARTESIAN_POINT('Ctrl Pts',(-56.0817671200782,-96.4370776667811,
171.81109657639));
#38423=CARTESIAN_POINT('Ctrl Pts',(-54.7914357012632,-96.668916845152,172.828569176292));
#38424=CARTESIAN_POINT('Ctrl Pts',(-53.5011042824482,-96.9007560235229,
173.846041776195));
#38425=CARTESIAN_POINT('Ctrl Pts',(-53.3070209377121,-97.0157278332795,
175.490142808619));
#38426=CARTESIAN_POINT('Ctrl Pts',(-53.1129375929761,-97.1306996430362,
177.134243841043));
#38427=CARTESIAN_POINT('Ctrl Pts',(-54.1346152959077,-97.1160632027404,
178.441881219107));
#38428=CARTESIAN_POINT('Ctrl Pts',(-55.1562929988393,-97.1014267624446,
179.74951859717));
#38429=CARTESIAN_POINT('Ctrl Pts',(-56.8010683899085,-97.0203639457436,
179.954696079469));
#38430=CARTESIAN_POINT('Ctrl Pts',(-58.4458437809776,-96.9393011290426,
180.159873561769));
#38431=CARTESIAN_POINT('Ctrl Pts',(-59.7560513256267,-96.8939054799824,
179.142400961866));
#38432=CARTESIAN_POINT('Ctrl Pts',(-61.0662588702757,-96.8485098309221,
178.124928361964));
#38433=CARTESIAN_POINT('Ctrl Pts',(-61.2802183408458,-96.9199815504762,
176.48082732954));
#38434=CARTESIAN_POINT('Ctrl Pts',(-61.4941778114159,-96.9914532700303,
174.836726297116));
#38435=CARTESIAN_POINT('Ctrl Pts',(-60.4923762343183,-97.1925332396368,
173.529088919052));
#38436=CARTESIAN_POINT('Ctrl Pts',(-59.4905746572207,-97.3936132092432,
172.221451540989));
#38437=CARTESIAN_POINT('Ctrl Pts',(-57.8656753919855,-97.661119555255,172.016274058689));
#38438=CARTESIAN_POINT('Ctrl Pts',(-56.2407761267504,-97.9286259012667,
171.81109657639));
#38439=CARTESIAN_POINT('Ctrl Pts',(-54.9504447079354,-98.1604650796376,
172.828569176292));
#38440=CARTESIAN_POINT('Ctrl Pts',(-53.6601132891204,-98.3923042580085,
173.846041776195));
#38441=CARTESIAN_POINT('Ctrl Pts',(-53.4660299443843,-98.5072760677652,
175.490142808619));
#38442=CARTESIAN_POINT('Ctrl Pts',(-53.2719465996483,-98.6222478775218,
177.134243841043));
#38443=CARTESIAN_POINT('Ctrl Pts',(-54.2936243025799,-98.607611437226,178.441881219107));
#38444=CARTESIAN_POINT('Ctrl Pts',(-55.3153020055115,-98.5929749969302,
179.74951859717));
#38445=CARTESIAN_POINT('Ctrl Pts',(-56.9600773965807,-98.5119121802292,
179.954696079469));
#38446=CARTESIAN_POINT('Ctrl Pts',(-58.6048527876499,-98.4308493635282,
180.159873561769));
#38447=CARTESIAN_POINT('Ctrl Pts',(-59.9150603322989,-98.385453714468,179.142400961866));
#38448=CARTESIAN_POINT('Ctrl Pts',(-61.2252678769479,-98.3400580654077,
178.124928361964));
#38449=CARTESIAN_POINT('Ctrl Pts',(-61.439227347518,-98.4115297849618,176.48082732954));
#38450=CARTESIAN_POINT('Ctrl Pts',(-61.6531868180881,-98.4830015045159,
174.836726297116));
#38451=CARTESIAN_POINT('Ctrl Pts',(-60.6513852409905,-98.6840814741224,
173.529088919052));
#38452=CARTESIAN_POINT('Ctrl Pts',(-59.6495836638929,-98.8851614437288,
172.221451540989));
#38453=CARTESIAN_POINT('Ctrl Pts',(-58.0246843986578,-99.1526677897406,
172.016274058689));
#38454=CARTESIAN_POINT('Ctrl Pts',(-56.3997851334226,-99.4201741357523,
171.81109657639));
#38455=CARTESIAN_POINT('Ctrl Pts',(-55.1094537146076,-99.6520133141232,
172.828569176292));
#38456=CARTESIAN_POINT('Ctrl Pts',(-53.8191222957926,-99.8838524924941,
173.846041776195));
#38457=CARTESIAN_POINT('Ctrl Pts',(-53.6250389510566,-99.9988243022507,
175.490142808619));
#38458=CARTESIAN_POINT('Ctrl Pts',(-53.4309556063205,-100.113796112007,
177.134243841043));
#38459=CARTESIAN_POINT('Ctrl Pts',(-54.4526333092521,-100.099159671712,
178.441881219107));
#38460=CARTESIAN_POINT('Ctrl Pts',(-55.4743110121837,-100.084523231416,
179.74951859717));
#38461=CARTESIAN_POINT('Ctrl Pts',(-57.1190864032529,-100.003460414715,
179.954696079469));
#38462=CARTESIAN_POINT('Ctrl Pts',(-58.7638617943221,-99.9223975980138,
180.159873561769));
#38463=CARTESIAN_POINT('Ctrl Pts',(-60.0740693389711,-99.8770019489536,
179.142400961866));
#38464=CARTESIAN_POINT('Ctrl Pts',(-61.3842768836201,-99.8316062998934,
178.124928361964));
#38465=CARTESIAN_POINT('Ctrl Pts',(-61.5982363541902,-99.9030780194474,
176.48082732954));
#38466=CARTESIAN_POINT('Ctrl Pts',(-61.8121958247603,-99.9745497390015,
174.836726297116));
#38467=CARTESIAN_POINT('Ctrl Pts',(-60.8103942476627,-100.175629708608,
173.529088919052));
#38468=CARTESIAN_POINT('Ctrl Pts',(-59.8085926705652,-100.376709678214,
172.221451540989));
#38469=CARTESIAN_POINT('Ctrl Pts',(-58.18369340533,-100.644216024226,172.016274058689));
#38470=CARTESIAN_POINT('Ctrl Pts',(-56.5587941400948,-100.911722370238,
171.81109657639));
#38471=CARTESIAN_POINT('Ctrl Pts',(-55.2684627212798,-101.143561548609,
172.828569176292));
#38472=CARTESIAN_POINT('Ctrl Pts',(-53.9781313024648,-101.37540072698,173.846041776195));
#38473=CARTESIAN_POINT('Ctrl Pts',(-53.7840479577288,-101.490372536736,
175.490142808619));
#38474=CARTESIAN_POINT('Ctrl Pts',(-53.5899646129927,-101.605344346493,
177.134243841043));
#38475=CARTESIAN_POINT('Ctrl Pts',(-54.6116423159243,-101.590707906197,
178.441881219107));
#38476=CARTESIAN_POINT('Ctrl Pts',(-55.6333200188559,-101.576071465901,
179.74951859717));
#38477=CARTESIAN_POINT('Ctrl Pts',(-57.2780954099251,-101.4950086492,179.954696079469));
#38478=CARTESIAN_POINT('Ctrl Pts',(-58.9228708009943,-101.413945832499,
180.159873561769));
#38479=CARTESIAN_POINT('Ctrl Pts',(-60.2330783456433,-101.368550183439,
179.142400961866));
#38480=CARTESIAN_POINT('Ctrl Pts',(-61.5432858902924,-101.323154534379,
178.124928361964));
#38481=CARTESIAN_POINT('Ctrl Pts',(-61.7572453608625,-101.394626253933,
176.48082732954));
#38482=CARTESIAN_POINT('Ctrl Pts',(-61.9712048314326,-101.466097973487,
174.836726297116));
#38483=CARTESIAN_POINT('Ctrl Pts',(-60.969403254335,-101.667177943094,173.529088919052));
#38484=CARTESIAN_POINT('Ctrl Pts',(-59.9676016772374,-101.8682579127,172.221451540989));
#38485=CARTESIAN_POINT('Ctrl Pts',(-58.3427024120022,-102.135764258712,
172.016274058689));
#38486=CARTESIAN_POINT('Ctrl Pts',(-56.7178031467671,-102.403270604724,
171.81109657639));
#38487=CARTESIAN_POINT('Ctrl Pts',(-55.4274717279521,-102.635109783094,
172.828569176292));
#38488=CARTESIAN_POINT('Ctrl Pts',(-54.1371403091371,-102.866948961465,
173.846041776195));
#38489=CARTESIAN_POINT('Ctrl Pts',(-53.943056964401,-102.981920771222,175.490142808619));
#38490=CARTESIAN_POINT('Ctrl Pts',(-53.748973619665,-103.096892580979,177.134243841043));
#38491=CARTESIAN_POINT('Ctrl Pts',(-54.7706513225966,-103.082256140683,
178.441881219107));
#38492=CARTESIAN_POINT('Ctrl Pts',(-55.7923290255282,-103.067619700387,
179.74951859717));
#38493=CARTESIAN_POINT('Ctrl Pts',(-57.4371044165974,-102.986556883686,
179.954696079469));
#38494=CARTESIAN_POINT('Ctrl Pts',(-59.0818798076666,-102.905494066985,
180.159873561769));
#38495=CARTESIAN_POINT('Ctrl Pts',(-60.3920873523156,-102.860098417925,
179.142400961866));
#38496=CARTESIAN_POINT('Ctrl Pts',(-61.7022948969646,-102.814702768865,
178.124928361964));
#38497=CARTESIAN_POINT('Ctrl Pts',(-61.9162543675347,-102.886174488419,
176.48082732954));
#38498=CARTESIAN_POINT('Ctrl Pts',(-62.1302138381048,-102.957646207973,
174.836726297116));
#38499=CARTESIAN_POINT('Ctrl Pts',(-61.1284122610072,-103.158726177579,
173.529088919052));
#38500=CARTESIAN_POINT('Ctrl Pts',(-60.1266106839096,-103.359806147186,
172.221451540989));
#38501=CARTESIAN_POINT('Ctrl Pts',(-58.5017114186745,-103.627312493197,
172.016274058689));
#38502=CARTESIAN_POINT('Ctrl Pts',(-56.8768121534393,-103.894818839209,
171.81109657639));
#38503=CARTESIAN_POINT('Ctrl Pts',(-55.5864807346243,-104.12665801758,172.828569176292));
#38504=CARTESIAN_POINT('Ctrl Pts',(-54.2961493158093,-104.358497195951,
173.846041776195));
#38505=CARTESIAN_POINT('Ctrl Pts',(-54.1020659710732,-104.473469005708,
175.490142808619));
#38506=CARTESIAN_POINT('Ctrl Pts',(-53.9079826263372,-104.588440815464,
177.134243841043));
#38507=CARTESIAN_POINT('Ctrl Pts',(-54.9296603292688,-104.573804375168,
178.441881219107));
#38508=CARTESIAN_POINT('Ctrl Pts',(-55.9513380322004,-104.559167934873,
179.74951859717));
#38509=CARTESIAN_POINT('Ctrl Pts',(-57.5961134232696,-104.478105118172,
179.954696079469));
#38510=CARTESIAN_POINT('Ctrl Pts',(-59.2408888143388,-104.397042301471,
180.159873561769));
#38511=CARTESIAN_POINT('Ctrl Pts',(-60.5510963589878,-104.35164665241,179.142400961866));
#38512=CARTESIAN_POINT('Ctrl Pts',(-61.8613039036368,-104.30625100335,178.124928361964));
#38513=CARTESIAN_POINT('Ctrl Pts',(-62.0752633742069,-104.377722722904,
176.48082732954));
#38514=CARTESIAN_POINT('Ctrl Pts',(-62.289222844777,-104.449194442458,174.836726297116));
#38515=CARTESIAN_POINT('Ctrl Pts',(-61.2874212676794,-104.650274412065,
173.529088919052));
#38516=CARTESIAN_POINT('Ctrl Pts',(-60.2856196905818,-104.851354381671,
172.221451540989));
#38517=CARTESIAN_POINT('Ctrl Pts',(-58.6607204253467,-105.118860727683,
172.016274058689));
#38518=CARTESIAN_POINT('Ctrl Pts',(-57.0358211601115,-105.386367073695,
171.81109657639));
#38519=CARTESIAN_POINT('Ctrl Pts',(-55.7454897412965,-105.618206252066,
172.828569176292));
#38520=CARTESIAN_POINT('Ctrl Pts',(-54.4551583224815,-105.850045430437,
173.846041776195));
#38521=CARTESIAN_POINT('Ctrl Pts',(-54.2610749777455,-105.965017240193,
175.490142808619));
#38522=CARTESIAN_POINT('Ctrl Pts',(-54.0669916330094,-106.07998904995,177.134243841043));
#38523=CARTESIAN_POINT('Ctrl Pts',(-55.088669335941,-106.065352609654,178.441881219107));
#38524=CARTESIAN_POINT('Ctrl Pts',(-56.1103470388726,-106.050716169358,
179.74951859717));
#38525=CARTESIAN_POINT('Ctrl Pts',(-57.7551224299418,-105.969653352657,
179.954696079469));
#38526=CARTESIAN_POINT('Ctrl Pts',(-59.399897821011,-105.888590535956,180.159873561769));
#38527=CARTESIAN_POINT('Ctrl Pts',(-60.71010536566,-105.843194886896,179.142400961866));
#38528=CARTESIAN_POINT('Ctrl Pts',(-62.0203129103091,-105.797799237836,
178.124928361964));
#38529=CARTESIAN_POINT('Ctrl Pts',(-62.2342723808791,-105.86927095739,176.48082732954));
#38530=CARTESIAN_POINT('Ctrl Pts',(-62.4482318514492,-105.940742676944,
174.836726297116));
#38531=CARTESIAN_POINT('Ctrl Pts',(-61.4464302743516,-106.14182264655,173.529088919052));
#38532=CARTESIAN_POINT('Ctrl Pts',(-60.4446286972541,-106.342902616157,
172.221451540989));
#38533=CARTESIAN_POINT('Ctrl Pts',(-58.8197294320189,-106.610408962169,
172.016274058689));
#38534=CARTESIAN_POINT('Ctrl Pts',(-57.1948301667837,-106.87791530818,171.81109657639));
#38535=CARTESIAN_POINT('Ctrl Pts',(-55.9044987479688,-107.109754486551,
172.828569176292));
#38536=CARTESIAN_POINT('Ctrl Pts',(-54.6141673291538,-107.341593664922,
173.846041776195));
#38537=CARTESIAN_POINT('Ctrl Pts',(-54.4200839844177,-107.456565474679,
175.490142808619));
#38538=CARTESIAN_POINT('Ctrl Pts',(-54.2260006396817,-107.571537284435,
177.134243841043));
#38539=CARTESIAN_POINT('Ctrl Pts',(-55.2476783426132,-107.55690084414,178.441881219107));
#38540=CARTESIAN_POINT('Ctrl Pts',(-56.2693560455449,-107.542264403844,
179.74951859717));
#38541=CARTESIAN_POINT('Ctrl Pts',(-57.914131436614,-107.461201587143,179.954696079469));
#38542=CARTESIAN_POINT('Ctrl Pts',(-59.5589068276832,-107.380138770442,
180.159873561769));
#38543=CARTESIAN_POINT('Ctrl Pts',(-60.8691143723323,-107.334743121382,
179.142400961866));
#38544=CARTESIAN_POINT('Ctrl Pts',(-62.1793219169813,-107.289347472321,
178.124928361964));
#38545=CARTESIAN_POINT('Ctrl Pts',(-62.3932813875514,-107.360819191875,
176.48082732954));
#38546=CARTESIAN_POINT('Ctrl Pts',(-62.6072408581214,-107.43229091143,174.836726297116));
#38547=CARTESIAN_POINT('Ctrl Pts',(-61.6054392810239,-107.633370881036,
173.529088919052));
#38548=CARTESIAN_POINT('Ctrl Pts',(-60.6036377039263,-107.834450850642,
172.221451540989));
#38549=CARTESIAN_POINT('Ctrl Pts',(-58.9787384386911,-108.101957196654,
172.016274058689));
#38550=CARTESIAN_POINT('Ctrl Pts',(-57.353839173456,-108.369463542666,171.81109657639));
#38551=CARTESIAN_POINT('Ctrl Pts',(-56.063507754641,-108.601302721037,172.828569176292));
#38552=CARTESIAN_POINT('Ctrl Pts',(-54.773176335826,-108.833141899408,173.846041776195));
#38553=CARTESIAN_POINT('Ctrl Pts',(-54.5790929910899,-108.948113709164,
175.490142808619));
#38554=CARTESIAN_POINT('Ctrl Pts',(-54.3850096463539,-109.063085518921,
177.134243841043));
#38555=CARTESIAN_POINT('Ctrl Pts',(-55.4066873492855,-109.048449078625,
178.441881219107));
#38556=CARTESIAN_POINT('Ctrl Pts',(-56.4283650522171,-109.033812638329,
179.74951859717));
#38557=CARTESIAN_POINT('Ctrl Pts',(-58.0731404432863,-108.952749821628,
179.954696079469));
#38558=CARTESIAN_POINT('Ctrl Pts',(-59.7179158343555,-108.871687004927,
180.159873561769));
#38559=CARTESIAN_POINT('Ctrl Pts',(-61.0281233790045,-108.826291355867,
179.142400961866));
#38560=CARTESIAN_POINT('Ctrl Pts',(-62.3383309236535,-108.780895706807,
178.124928361964));
#38561=CARTESIAN_POINT('Ctrl Pts',(-62.5522903942236,-108.852367426361,
176.48082732954));
#38562=CARTESIAN_POINT('Ctrl Pts',(-62.7662498647937,-108.923839145915,
174.836726297116));
#38563=CARTESIAN_POINT('Ctrl Pts',(-61.7644482876961,-109.124919115522,
173.529088919052));
#38564=CARTESIAN_POINT('Ctrl Pts',(-60.7626467105985,-109.325999085128,
172.221451540989));
#38565=CARTESIAN_POINT('Ctrl Pts',(-59.1377474453634,-109.59350543114,172.016274058689));
#38566=CARTESIAN_POINT('Ctrl Pts',(-57.5128481801282,-109.861011777152,
171.81109657639));
#38567=CARTESIAN_POINT('Ctrl Pts',(-56.2225167613132,-110.092850955522,
172.828569176292));
#38568=CARTESIAN_POINT('Ctrl Pts',(-54.9321853424982,-110.324690133893,
173.846041776195));
#38569=CARTESIAN_POINT('Ctrl Pts',(-54.7381019977622,-110.43966194365,175.490142808619));
#38570=CARTESIAN_POINT('Ctrl Pts',(-54.5440186530261,-110.554633753407,
177.134243841043));
#38571=CARTESIAN_POINT('Ctrl Pts',(-55.5656963559577,-110.539997313111,
178.441881219107));
#38572=CARTESIAN_POINT('Ctrl Pts',(-56.5873740588893,-110.525360872815,
179.74951859717));
#38573=CARTESIAN_POINT('Ctrl Pts',(-58.2321494499585,-110.444298056114,
179.954696079469));
#38574=CARTESIAN_POINT('Ctrl Pts',(-59.8769248410277,-110.363235239413,
180.159873561769));
#38575=CARTESIAN_POINT('Ctrl Pts',(-61.1871323856767,-110.317839590353,
179.142400961866));
#38576=CARTESIAN_POINT('Ctrl Pts',(-62.4973399303257,-110.272443941293,
178.124928361964));
#38577=CARTESIAN_POINT('Ctrl Pts',(-62.7112994008958,-110.343915660847,
176.48082732954));
#38578=CARTESIAN_POINT('Ctrl Pts',(-62.9252588714659,-110.415387380401,
174.836726297116));
#38579=CARTESIAN_POINT('Ctrl Pts',(-61.9234572943683,-110.616467350007,
173.529088919052));
#38580=CARTESIAN_POINT('Ctrl Pts',(-60.9216557172708,-110.817547319614,
172.221451540989));
#38581=CARTESIAN_POINT('Ctrl Pts',(-59.2967564520356,-111.085053665625,
172.016274058689));
#38582=CARTESIAN_POINT('Ctrl Pts',(-57.6718571868004,-111.352560011637,
171.81109657639));
#38583=CARTESIAN_POINT('Ctrl Pts',(-56.3815257679854,-111.584399190008,
172.828569176292));
#38584=CARTESIAN_POINT('Ctrl Pts',(-55.0911943491704,-111.816238368379,
173.846041776195));
#38585=CARTESIAN_POINT('Ctrl Pts',(-54.8971110044344,-111.931210178136,
175.490142808619));
#38586=CARTESIAN_POINT('Ctrl Pts',(-54.7030276596983,-112.046181987892,
177.134243841043));
#38587=CARTESIAN_POINT('Ctrl Pts',(-55.7247053626299,-112.031545547596,
178.441881219107));
#38588=CARTESIAN_POINT('Ctrl Pts',(-56.7463830655615,-112.016909107301,
179.74951859717));
#38589=CARTESIAN_POINT('Ctrl Pts',(-58.3911584566307,-111.9358462906,179.954696079469));
#38590=CARTESIAN_POINT('Ctrl Pts',(-60.0359338476999,-111.854783473899,
180.159873561769));
#38591=CARTESIAN_POINT('Ctrl Pts',(-61.3461413923489,-111.809387824838,
179.142400961866));
#38592=CARTESIAN_POINT('Ctrl Pts',(-62.656348936998,-111.763992175778,178.124928361964));
#38593=CARTESIAN_POINT('Ctrl Pts',(-62.870308407568,-111.835463895332,176.48082732954));
#38594=CARTESIAN_POINT('Ctrl Pts',(-63.0842678781381,-111.906935614886,
174.836726297116));
#38595=CARTESIAN_POINT('Ctrl Pts',(-62.0824663010406,-112.108015584493,
173.529088919052));
#38596=CARTESIAN_POINT('Ctrl Pts',(-61.080664723943,-112.309095554099,172.221451540989));
#38597=CARTESIAN_POINT('Ctrl Pts',(-59.4557654587078,-112.576601900111,
172.016274058689));
#38598=CARTESIAN_POINT('Ctrl Pts',(-57.8308661934727,-112.844108246123,
171.81109657639));
#38599=CARTESIAN_POINT('Ctrl Pts',(-56.5405347746577,-113.075947424494,
172.828569176292));
#38600=CARTESIAN_POINT('Ctrl Pts',(-55.2502033558427,-113.307786602865,
173.846041776195));
#38601=CARTESIAN_POINT('Ctrl Pts',(-55.0561200111066,-113.422758412621,
175.490142808619));
#38602=CARTESIAN_POINT('Ctrl Pts',(-54.8620366663706,-113.537730222378,
177.134243841043));
#38603=CARTESIAN_POINT('Ctrl Pts',(-55.8837143693022,-113.523093782082,
178.441881219107));
#38604=CARTESIAN_POINT('Ctrl Pts',(-56.9053920722338,-113.508457341786,
179.74951859717));
#38605=CARTESIAN_POINT('Ctrl Pts',(-58.550167463303,-113.427394525085,179.954696079469));
#38606=CARTESIAN_POINT('Ctrl Pts',(-60.1949428543721,-113.346331708384,
180.159873561769));
#38607=CARTESIAN_POINT('Ctrl Pts',(-61.5051503990212,-113.300936059324,
179.142400961866));
#38608=CARTESIAN_POINT('Ctrl Pts',(-62.8153579436702,-113.255540410264,
178.124928361964));
#38609=CARTESIAN_POINT('Ctrl Pts',(-63.0293174142403,-113.327012129818,
176.48082732954));
#38610=CARTESIAN_POINT('Ctrl Pts',(-63.2432768848104,-113.398483849372,
174.836726297116));
#38611=CARTESIAN_POINT('Ctrl Pts',(-62.2414753077128,-113.599563818978,
173.529088919052));
#38612=CARTESIAN_POINT('Ctrl Pts',(-61.2396737306152,-113.800643788585,
172.221451540989));
#38613=CARTESIAN_POINT('Ctrl Pts',(-59.6147744653801,-114.068150134597,
172.016274058689));
#38614=CARTESIAN_POINT('Ctrl Pts',(-57.9898752001449,-114.335656480608,
171.81109657639));
#38615=CARTESIAN_POINT('Ctrl Pts',(-56.6995437813299,-114.567495658979,
172.828569176292));
#38616=CARTESIAN_POINT('Ctrl Pts',(-55.4092123625149,-114.79933483735,173.846041776195));
#38617=CARTESIAN_POINT('Ctrl Pts',(-55.2151290177788,-114.914306647107,
175.490142808619));
#38618=CARTESIAN_POINT('Ctrl Pts',(-55.0210456730428,-115.029278456863,
177.134243841043));
#38619=CARTESIAN_POINT('Ctrl Pts',(-56.0427233759744,-115.014642016568,
178.441881219107));
#38620=CARTESIAN_POINT('Ctrl Pts',(-57.064401078906,-115.000005576272,179.74951859717));
#38621=CARTESIAN_POINT('Ctrl Pts',(-58.7091764699752,-114.918942759571,
179.954696079469));
#38622=CARTESIAN_POINT('Ctrl Pts',(-60.3539518610444,-114.83787994287,180.159873561769));
#38623=CARTESIAN_POINT('Ctrl Pts',(-61.6641594056934,-114.79248429381,179.142400961866));
#38624=CARTESIAN_POINT('Ctrl Pts',(-62.9743669503424,-114.747088644749,
178.124928361964));
#38625=CARTESIAN_POINT('Ctrl Pts',(-63.1883264209125,-114.818560364303,
176.48082732954));
#38626=CARTESIAN_POINT('Ctrl Pts',(-63.4022858914826,-114.890032083858,
174.836726297116));
#38627=CARTESIAN_POINT('Ctrl Pts',(-62.400484314385,-115.091112053464,173.529088919052));
#38628=CARTESIAN_POINT('Ctrl Pts',(-61.3986827372874,-115.29219202307,172.221451540989));
#38629=CARTESIAN_POINT('Ctrl Pts',(-59.7737834720523,-115.559698369082,
172.016274058689));
#38630=CARTESIAN_POINT('Ctrl Pts',(-58.1488842068171,-115.827204715094,
171.81109657639));
#38631=CARTESIAN_POINT('Ctrl Pts',(-56.8585527880021,-116.059043893465,
172.828569176292));
#38632=CARTESIAN_POINT('Ctrl Pts',(-55.5682213691871,-116.290883071836,
173.846041776195));
#38633=CARTESIAN_POINT('Ctrl Pts',(-55.3741380244511,-116.405854881592,
175.490142808619));
#38634=CARTESIAN_POINT('Ctrl Pts',(-55.180054679715,-116.520826691349,177.134243841043));
#38635=CARTESIAN_POINT('Ctrl Pts',(-56.2017323826466,-116.506190251053,
178.441881219107));
#38636=CARTESIAN_POINT('Ctrl Pts',(-57.2234100855782,-116.491553810757,
179.74951859717));
#38637=CARTESIAN_POINT('Ctrl Pts',(-58.8681854766474,-116.410490994056,
179.954696079469));
#38638=CARTESIAN_POINT('Ctrl Pts',(-60.5129608677166,-116.329428177355,
180.159873561769));
#38639=CARTESIAN_POINT('Ctrl Pts',(-61.8231684123656,-116.284032528295,
179.142400961866));
#38640=CARTESIAN_POINT('Ctrl Pts',(-63.1333759570146,-116.238636879235,
178.124928361964));
#38641=CARTESIAN_POINT('Ctrl Pts',(-63.3473354275847,-116.310108598789,
176.48082732954));
#38642=CARTESIAN_POINT('Ctrl Pts',(-63.5612948981548,-116.381580318343,
174.836726297116));
#38643=CARTESIAN_POINT('Ctrl Pts',(-62.5594933210572,-116.58266028795,173.529088919052));
#38644=CARTESIAN_POINT('Ctrl Pts',(-61.5576917439597,-116.783740257556,
172.221451540989));
#38645=CARTESIAN_POINT('Ctrl Pts',(-59.9327924787245,-117.051246603568,
172.016274058689));
#38646=CARTESIAN_POINT('Ctrl Pts',(-58.3078932134894,-117.318752949579,
171.81109657639));
#38647=CARTESIAN_POINT('Ctrl Pts',(-57.0175617946743,-117.55059212795,172.828569176292));
#38648=CARTESIAN_POINT('Ctrl Pts',(-55.7272303758593,-117.782431306321,
173.846041776195));
#38649=CARTESIAN_POINT('Ctrl Pts',(-55.5331470311233,-117.897403116078,
175.490142808619));
#38650=CARTESIAN_POINT('Ctrl Pts',(-55.3390636863872,-118.012374925835,
177.134243841043));
#38651=CARTESIAN_POINT('Ctrl Pts',(-56.3607413893188,-117.997738485539,
178.441881219107));
#38652=CARTESIAN_POINT('Ctrl Pts',(-57.3824190922504,-117.983102045243,
179.74951859717));
#38653=CARTESIAN_POINT('Ctrl Pts',(-59.0271944833196,-117.902039228542,
179.954696079469));
#38654=CARTESIAN_POINT('Ctrl Pts',(-60.6719698743888,-117.820976411841,
180.159873561769));
#38655=CARTESIAN_POINT('Ctrl Pts',(-61.9821774190378,-117.775580762781,
179.142400961866));
#38656=CARTESIAN_POINT('Ctrl Pts',(-63.2923849636869,-117.730185113721,
178.124928361964));
#38657=CARTESIAN_POINT('Ctrl Pts',(-63.506344434257,-117.801656833275,176.48082732954));
#38658=CARTESIAN_POINT('Ctrl Pts',(-63.720303904827,-117.873128552829,174.836726297116));
#38659=CARTESIAN_POINT('Ctrl Pts',(-62.7185023277295,-118.074208522435,
173.529088919052));
#38660=CARTESIAN_POINT('Ctrl Pts',(-61.7167007506319,-118.275288492042,
172.221451540989));
#38661=CARTESIAN_POINT('Ctrl Pts',(-60.0918014853967,-118.542794838053,
172.016274058689));
#38662=CARTESIAN_POINT('Ctrl Pts',(-58.4669022201616,-118.810301184065,
171.81109657639));
#38663=CARTESIAN_POINT('Ctrl Pts',(-57.1765708013466,-119.042140362436,
172.828569176292));
#38664=CARTESIAN_POINT('Ctrl Pts',(-55.8862393825316,-119.273979540807,
173.846041776195));
#38665=CARTESIAN_POINT('Ctrl Pts',(-55.6921560377955,-119.388951350564,
175.490142808619));
#38666=CARTESIAN_POINT('Ctrl Pts',(-55.4980726930595,-119.50392316032,177.134243841043));
#38667=CARTESIAN_POINT('Ctrl Pts',(-56.5197503959911,-119.489286720024,
178.441881219107));
#38668=CARTESIAN_POINT('Ctrl Pts',(-57.5414280989227,-119.474650279729,
179.74951859717));
#38669=CARTESIAN_POINT('Ctrl Pts',(-59.1862034899919,-119.393587463028,
179.954696079469));
#38670=CARTESIAN_POINT('Ctrl Pts',(-60.8309788810611,-119.312524646327,
180.159873561769));
#38671=CARTESIAN_POINT('Ctrl Pts',(-62.1411864257101,-119.267128997266,
179.142400961866));
#38672=CARTESIAN_POINT('Ctrl Pts',(-63.4513939703591,-119.221733348206,
178.124928361964));
#38673=CARTESIAN_POINT('Ctrl Pts',(-63.6653534409292,-119.29320506776,176.48082732954));
#38674=CARTESIAN_POINT('Ctrl Pts',(-63.8793129114993,-119.364676787314,
174.836726297116));
#38675=CARTESIAN_POINT('Ctrl Pts',(-62.8775113344017,-119.565756756921,
173.529088919052));
#38676=CARTESIAN_POINT('Ctrl Pts',(-61.8757097573041,-119.766836726527,
172.221451540989));
#38677=CARTESIAN_POINT('Ctrl Pts',(-60.250810492069,-120.034343072539,172.016274058689));
#38678=CARTESIAN_POINT('Ctrl Pts',(-58.6259112268338,-120.301849418551,
171.81109657639));
#38679=CARTESIAN_POINT('Ctrl Pts',(-57.3355798080188,-120.533688596922,
172.828569176292));
#38680=CARTESIAN_POINT('Ctrl Pts',(-56.0452483892038,-120.765527775293,
173.846041776195));
#38681=CARTESIAN_POINT('Ctrl Pts',(-55.8511650444677,-120.880499585049,
175.490142808619));
#38682=CARTESIAN_POINT('Ctrl Pts',(-55.6570816997317,-120.995471394806,
177.134243841043));
#38683=CARTESIAN_POINT('Ctrl Pts',(-56.6787594026633,-120.98083495451,178.441881219107));
#38684=CARTESIAN_POINT('Ctrl Pts',(-57.7004371055949,-120.966198514214,
179.74951859717));
#38685=CARTESIAN_POINT('Ctrl Pts',(-59.3452124966641,-120.885135697513,
179.954696079469));
#38686=CARTESIAN_POINT('Ctrl Pts',(-60.9899878877333,-120.804072880812,
180.159873561769));
#38687=CARTESIAN_POINT('Ctrl Pts',(-62.3001954323823,-120.758677231752,
179.142400961866));
#38688=CARTESIAN_POINT('Ctrl Pts',(-63.6104029770313,-120.713281582692,
178.124928361964));
#38689=CARTESIAN_POINT('Ctrl Pts',(-63.8243624476014,-120.784753302246,
176.48082732954));
#38690=CARTESIAN_POINT('Ctrl Pts',(-64.0383219181715,-120.8562250218,174.836726297116));
#38691=CARTESIAN_POINT('Ctrl Pts',(-63.0365203410739,-121.057304991406,
173.529088919052));
#38692=CARTESIAN_POINT('Ctrl Pts',(-62.0347187639764,-121.258384961013,
172.221451540989));
#38693=CARTESIAN_POINT('Ctrl Pts',(-60.4098194987412,-121.525891307025,
172.016274058689));
#38694=CARTESIAN_POINT('Ctrl Pts',(-58.784920233506,-121.793397653036,171.81109657639));
#38695=CARTESIAN_POINT('Ctrl Pts',(-57.494588814691,-122.025236831407,172.828569176292));
#38696=CARTESIAN_POINT('Ctrl Pts',(-56.204257395876,-122.257076009778,173.846041776195));
#38697=CARTESIAN_POINT('Ctrl Pts',(-56.01017405114,-122.372047819535,175.490142808619));
#38698=CARTESIAN_POINT('Ctrl Pts',(-55.8160907064039,-122.487019629291,
177.134243841043));
#38699=CARTESIAN_POINT('Ctrl Pts',(-56.8377684093355,-122.472383188996,
178.441881219107));
#38700=CARTESIAN_POINT('Ctrl Pts',(-57.8594461122671,-122.4577467487,179.74951859717));
#38701=CARTESIAN_POINT('Ctrl Pts',(-59.5042215033363,-122.376683931999,
179.954696079469));
#38702=CARTESIAN_POINT('Ctrl Pts',(-61.1489968944055,-122.295621115298,
180.159873561769));
#38703=CARTESIAN_POINT('Ctrl Pts',(-62.4592044390545,-122.250225466238,
179.142400961866));
#38704=CARTESIAN_POINT('Ctrl Pts',(-63.7694119837035,-122.204829817177,
178.124928361964));
#38705=CARTESIAN_POINT('Ctrl Pts',(-63.9833714542736,-122.276301536731,
176.48082732954));
#38706=CARTESIAN_POINT('Ctrl Pts',(-64.1973309248437,-122.347773256285,
174.836726297116));
#38707=CARTESIAN_POINT('Ctrl Pts',(-63.1955293477461,-122.548853225892,
173.529088919052));
#38708=CARTESIAN_POINT('Ctrl Pts',(-62.1937277706486,-122.749933195498,
172.221451540989));
#38709=CARTESIAN_POINT('Ctrl Pts',(-60.5688285054134,-123.01743954151,172.016274058689));
#38710=CARTESIAN_POINT('Ctrl Pts',(-58.9439292401782,-123.284945887522,
171.81109657639));
#38711=CARTESIAN_POINT('Ctrl Pts',(-57.6535978213633,-123.516785065893,
172.828569176292));
#38712=CARTESIAN_POINT('Ctrl Pts',(-56.3632664025483,-123.748624244264,
173.846041776195));
#38713=CARTESIAN_POINT('Ctrl Pts',(-56.1691830578122,-123.86359605402,175.490142808619));
#38714=CARTESIAN_POINT('Ctrl Pts',(-55.9750997130761,-123.978567863777,
177.134243841043));
#38715=CARTESIAN_POINT('Ctrl Pts',(-56.9967774160077,-123.963931423481,
178.441881219107));
#38716=CARTESIAN_POINT('Ctrl Pts',(-58.0184551189394,-123.949294983185,
179.74951859717));
#38717=CARTESIAN_POINT('Ctrl Pts',(-59.6632305100085,-123.868232166484,
179.954696079469));
#38718=CARTESIAN_POINT('Ctrl Pts',(-61.3080059010777,-123.787169349783,
180.159873561769));
#38719=CARTESIAN_POINT('Ctrl Pts',(-62.6182134457268,-123.741773700723,
179.142400961866));
#38720=CARTESIAN_POINT('Ctrl Pts',(-63.9284209903758,-123.696378051663,
178.124928361964));
#38721=CARTESIAN_POINT('Ctrl Pts',(-64.1423804609459,-123.767849771217,
176.48082732954));
#38722=CARTESIAN_POINT('Ctrl Pts',(-64.3563399315159,-123.839321490771,
174.836726297116));
#38723=CARTESIAN_POINT('Ctrl Pts',(-63.3545383544184,-124.040401460378,
173.529088919052));
#38724=CARTESIAN_POINT('Ctrl Pts',(-62.3527367773208,-124.241481429984,
172.221451540989));
#38725=CARTESIAN_POINT('Ctrl Pts',(-60.7278375120856,-124.508987775996,
172.016274058689));
#38726=CARTESIAN_POINT('Ctrl Pts',(-59.1029382468505,-124.776494122007,
171.81109657639));
#38727=CARTESIAN_POINT('Ctrl Pts',(-57.8126068280355,-125.008333300378,
172.828569176292));
#38728=CARTESIAN_POINT('Ctrl Pts',(-56.5222754092205,-125.240172478749,
173.846041776195));
#38729=CARTESIAN_POINT('Ctrl Pts',(-56.3281920644844,-125.355144288506,
175.490142808619));
#38730=CARTESIAN_POINT('Ctrl Pts',(-56.1341087197484,-125.470116098263,
177.134243841043));
#38731=CARTESIAN_POINT('Ctrl Pts',(-57.15578642268,-125.455479657967,178.441881219107));
#38732=CARTESIAN_POINT('Ctrl Pts',(-58.1774641256116,-125.440843217671,
179.74951859717));
#38733=CARTESIAN_POINT('Ctrl Pts',(-59.8222395166808,-125.35978040097,179.954696079469));
#38734=CARTESIAN_POINT('Ctrl Pts',(-61.46701490775,-125.278717584269,180.159873561769));
#38735=CARTESIAN_POINT('Ctrl Pts',(-62.777222452399,-125.233321935209,179.142400961866));
#38736=CARTESIAN_POINT('Ctrl Pts',(-64.087429997048,-125.187926286149,178.124928361964));
#38737=CARTESIAN_POINT('Ctrl Pts',(-64.3013894676181,-125.259398005703,
176.48082732954));
#38738=CARTESIAN_POINT('Ctrl Pts',(-64.5153489381882,-125.330869725257,
174.836726297116));
#38739=CARTESIAN_POINT('Ctrl Pts',(-63.5135473610906,-125.531949694863,
173.529088919052));
#38740=CARTESIAN_POINT('Ctrl Pts',(-62.511745783993,-125.73302966447,172.221451540989));
#38741=CARTESIAN_POINT('Ctrl Pts',(-60.8868465187579,-126.000536010481,
172.016274058689));
#38742=CARTESIAN_POINT('Ctrl Pts',(-59.2619472535227,-126.268042356493,
171.81109657639));
#38743=CARTESIAN_POINT('Ctrl Pts',(-57.9716158347077,-126.499881534864,
172.828569176292));
#38744=CARTESIAN_POINT('Ctrl Pts',(-56.6812844158927,-126.731720713235,
173.846041776195));
#38745=CARTESIAN_POINT('Ctrl Pts',(-56.4872010711566,-126.846692522992,
175.490142808619));
#38746=CARTESIAN_POINT('Ctrl Pts',(-56.2931177264206,-126.961664332748,
177.134243841043));
#38747=CARTESIAN_POINT('Ctrl Pts',(-57.3147954293522,-126.947027892452,
178.441881219107));
#38748=CARTESIAN_POINT('Ctrl Pts',(-58.3364731322838,-126.932391452157,
179.74951859717));
#38749=CARTESIAN_POINT('Ctrl Pts',(-59.981248523353,-126.851328635456,179.954696079469));
#38750=CARTESIAN_POINT('Ctrl Pts',(-61.6260239144222,-126.770265818755,
180.159873561769));
#38751=CARTESIAN_POINT('Ctrl Pts',(-62.9362314590712,-126.724870169694,
179.142400961866));
#38752=CARTESIAN_POINT('Ctrl Pts',(-64.2464390037202,-126.679474520634,
178.124928361964));
#38753=CARTESIAN_POINT('Ctrl Pts',(-64.4603984742903,-126.750946240188,
176.48082732954));
#38754=CARTESIAN_POINT('Ctrl Pts',(-64.6743579448604,-126.822417959742,
174.836726297116));
#38755=CARTESIAN_POINT('Ctrl Pts',(-63.6725563677628,-127.023497929349,
173.529088919052));
#38756=CARTESIAN_POINT('Ctrl Pts',(-62.6707547906653,-127.224577898955,
172.221451540989));
#38757=CARTESIAN_POINT('Ctrl Pts',(-61.0458555254301,-127.492084244967,
172.016274058689));
#38758=CARTESIAN_POINT('Ctrl Pts',(-59.4209562601949,-127.759590590979,
171.81109657639));
#38759=CARTESIAN_POINT('Ctrl Pts',(-58.1306248413799,-127.99142976935,172.828569176292));
#38760=CARTESIAN_POINT('Ctrl Pts',(-56.8402934225649,-128.223268947721,
173.846041776195));
#38761=CARTESIAN_POINT('Ctrl Pts',(-56.6462100778289,-128.338240757477,
175.490142808619));
#38762=CARTESIAN_POINT('Ctrl Pts',(-56.4521267330928,-128.453212567234,
177.134243841043));
#38763=CARTESIAN_POINT('Ctrl Pts',(-57.4738044360244,-128.438576126938,
178.441881219107));
#38764=CARTESIAN_POINT('Ctrl Pts',(-58.495482138956,-128.423939686642,179.74951859717));
#38765=CARTESIAN_POINT('Ctrl Pts',(-60.1402575300252,-128.342876869941,
179.954696079469));
#38766=CARTESIAN_POINT('Ctrl Pts',(-61.7850329210944,-128.26181405324,180.159873561769));
#38767=CARTESIAN_POINT('Ctrl Pts',(-63.0952404657434,-128.21641840418,179.142400961866));
#38768=CARTESIAN_POINT('Ctrl Pts',(-64.4054480103925,-128.17102275512,178.124928361964));
#38769=CARTESIAN_POINT('Ctrl Pts',(-64.6194074809625,-128.242494474674,
176.48082732954));
#38770=CARTESIAN_POINT('Ctrl Pts',(-64.8333669515326,-128.313966194228,
174.836726297116));
#38771=CARTESIAN_POINT('Ctrl Pts',(-63.831565374435,-128.515046163834,173.529088919052));
#38772=CARTESIAN_POINT('Ctrl Pts',(-62.8297637973375,-128.716126133441,
172.221451540989));
#38773=CARTESIAN_POINT('Ctrl Pts',(-61.2048645321023,-128.983632479453,
172.016274058689));
#38774=CARTESIAN_POINT('Ctrl Pts',(-59.5799652668672,-129.251138825464,
171.81109657639));
#38775=CARTESIAN_POINT('Ctrl Pts',(-58.2896338480522,-129.482978003835,
172.828569176292));
#38776=CARTESIAN_POINT('Ctrl Pts',(-56.9993024292372,-129.714817182206,
173.846041776195));
#38777=CARTESIAN_POINT('Ctrl Pts',(-56.8052190845011,-129.829788991963,
175.490142808619));
#38778=CARTESIAN_POINT('Ctrl Pts',(-56.611135739765,-129.944760801719,177.134243841043));
#38779=CARTESIAN_POINT('Ctrl Pts',(-57.6328134426967,-129.930124361424,
178.441881219107));
#38780=CARTESIAN_POINT('Ctrl Pts',(-58.6544911456282,-129.915487921128,
179.74951859717));
#38781=CARTESIAN_POINT('Ctrl Pts',(-60.2992665366974,-129.834425104427,
179.954696079469));
#38782=CARTESIAN_POINT('Ctrl Pts',(-61.9440419277666,-129.753362287726,
180.159873561769));
#38783=CARTESIAN_POINT('Ctrl Pts',(-63.2542494724157,-129.707966638666,
179.142400961866));
#38784=CARTESIAN_POINT('Ctrl Pts',(-64.5644570170647,-129.662570989605,
178.124928361964));
#38785=CARTESIAN_POINT('Ctrl Pts',(-64.7784164876348,-129.734042709159,
176.48082732954));
#38786=CARTESIAN_POINT('Ctrl Pts',(-64.9923759582049,-129.805514428714,
174.836726297116));
#38787=CARTESIAN_POINT('Ctrl Pts',(-63.9905743811073,-130.00659439832,173.529088919052));
#38788=CARTESIAN_POINT('Ctrl Pts',(-62.9887728040097,-130.207674367926,
172.221451540989));
#38789=CARTESIAN_POINT('Ctrl Pts',(-61.3638735387745,-130.475180713938,
172.016274058689));
#38790=CARTESIAN_POINT('Ctrl Pts',(-59.7389742735394,-130.74268705995,171.81109657639));
#38791=CARTESIAN_POINT('Ctrl Pts',(-58.4486428547244,-130.974526238321,
172.828569176292));
#38792=CARTESIAN_POINT('Ctrl Pts',(-57.1583114359094,-131.206365416692,
173.846041776195));
#38793=CARTESIAN_POINT('Ctrl Pts',(-56.9642280911733,-131.321337226448,
175.490142808619));
#38794=CARTESIAN_POINT('Ctrl Pts',(-56.7701447464373,-131.436309036205,
177.134243841043));
#38795=CARTESIAN_POINT('Ctrl Pts',(-57.7918224493689,-131.421672595909,
178.441881219107));
#38796=CARTESIAN_POINT('Ctrl Pts',(-58.8135001523005,-131.407036155613,
179.74951859717));
#38797=CARTESIAN_POINT('Ctrl Pts',(-60.4582755433697,-131.325973338912,
179.954696079469));
#38798=CARTESIAN_POINT('Ctrl Pts',(-61.522217219021,-131.273536933612,180.087417468365));
#38799=CARTESIAN_POINT('Ctrl Pts',(-62.5109440081377,-131.233579209696,
179.670624062921));
#38800=CARTESIAN_POINT('Ctrl Pts',(-67.5782957416017,-131.028790744588,
177.534504349347));
#38801=CARTESIAN_POINT('Ctrl Pts',(-72.6456474750658,-130.824002279481,
175.398384635772));
#38802=CARTESIAN_POINT('Ctrl Pts',(-58.0980103408427,-67.1520871615593,
175.424797521432));
#38803=CARTESIAN_POINT('Ctrl Pts',(-57.9563744146254,-67.2322701352371,
174.369925727914));
#38804=CARTESIAN_POINT('Ctrl Pts',(-57.3121961008737,-67.3615685499248,
173.529088919052));
#38805=CARTESIAN_POINT('Ctrl Pts',(-56.3103945237762,-67.5626485195312,
172.221451540989));
#38806=CARTESIAN_POINT('Ctrl Pts',(-54.685495258541,-67.830154865543,172.016274058689));
#38807=CARTESIAN_POINT('Ctrl Pts',(-53.0605959933058,-68.0976612115547,
171.81109657639));
#38808=CARTESIAN_POINT('Ctrl Pts',(-51.7702645744908,-68.3295003899256,
172.828569176292));
#38809=CARTESIAN_POINT('Ctrl Pts',(-50.4799331556759,-68.5613395682965,
173.846041776195));
#38810=CARTESIAN_POINT('Ctrl Pts',(-50.2858498109398,-68.6763113780532,
175.490142808619));
#38811=CARTESIAN_POINT('Ctrl Pts',(-50.0917664662038,-68.7912831878098,
177.134243841043));
#38812=CARTESIAN_POINT('Ctrl Pts',(-51.1134441691353,-68.776646747514,178.441881219107));
#38813=CARTESIAN_POINT('Ctrl Pts',(-52.1351218720669,-68.7620103072182,
179.74951859717));
#38814=CARTESIAN_POINT('Ctrl Pts',(-53.7798972631361,-68.6809474905172,
179.954696079469));
#38815=CARTESIAN_POINT('Ctrl Pts',(-55.4246726542053,-68.5998846738162,
180.159873561769));
#38816=CARTESIAN_POINT('Ctrl Pts',(-56.7348801988543,-68.5544890247559,
179.142400961866));
#38817=CARTESIAN_POINT('Ctrl Pts',(-58.0450877435034,-68.5090933756957,
178.124928361964));
#38818=CARTESIAN_POINT('Ctrl Pts',(-58.2590472140735,-68.5805650952498,
176.48082732954));
#38819=CARTESIAN_POINT('Ctrl Pts',(-58.4730066846436,-68.6520368148039,
174.836726297116));
#38820=CARTESIAN_POINT('Ctrl Pts',(-57.471205107546,-68.8531167844104,173.529088919052));
#38821=CARTESIAN_POINT('Ctrl Pts',(-56.4694035304484,-69.0541967540168,
172.221451540989));
#38822=CARTESIAN_POINT('Ctrl Pts',(-54.8445042652132,-69.3217031000286,
172.016274058689));
#38823=CARTESIAN_POINT('Ctrl Pts',(-53.2196049999781,-69.5892094460403,
171.81109657639));
#38824=CARTESIAN_POINT('Ctrl Pts',(-51.9292735811631,-69.8210486244112,
172.828569176292));
#38825=CARTESIAN_POINT('Ctrl Pts',(-50.6389421623481,-70.0528878027821,
173.846041776195));
#38826=CARTESIAN_POINT('Ctrl Pts',(-50.444858817612,-70.1678596125387,175.490142808619));
#38827=CARTESIAN_POINT('Ctrl Pts',(-50.250775472876,-70.2828314222954,177.134243841043));
#38828=CARTESIAN_POINT('Ctrl Pts',(-51.2724531758076,-70.2681949819996,
178.441881219107));
#38829=CARTESIAN_POINT('Ctrl Pts',(-52.2941308787392,-70.2535585417038,
179.74951859717));
#38830=CARTESIAN_POINT('Ctrl Pts',(-53.9389062698084,-70.1724957250028,
179.954696079469));
#38831=CARTESIAN_POINT('Ctrl Pts',(-55.5836816608776,-70.0914329083018,
180.159873561769));
#38832=CARTESIAN_POINT('Ctrl Pts',(-56.8938892055266,-70.0460372592415,
179.142400961866));
#38833=CARTESIAN_POINT('Ctrl Pts',(-58.2040967501756,-70.0006416101813,
178.124928361964));
#38834=CARTESIAN_POINT('Ctrl Pts',(-58.4180562207457,-70.0721133297354,
176.48082732954));
#38835=CARTESIAN_POINT('Ctrl Pts',(-58.6320156913158,-70.1435850492895,
174.836726297116));
#38836=CARTESIAN_POINT('Ctrl Pts',(-57.6302141142182,-70.344665018896,173.529088919052));
#38837=CARTESIAN_POINT('Ctrl Pts',(-56.6284125371206,-70.5457449885024,
172.221451540989));
#38838=CARTESIAN_POINT('Ctrl Pts',(-55.0035132718855,-70.8132513345142,
172.016274058689));
#38839=CARTESIAN_POINT('Ctrl Pts',(-53.3786140066503,-71.0807576805259,
171.81109657639));
#38840=CARTESIAN_POINT('Ctrl Pts',(-52.0882825878353,-71.3125968588968,
172.828569176292));
#38841=CARTESIAN_POINT('Ctrl Pts',(-50.7979511690203,-71.5444360372677,
173.846041776195));
#38842=CARTESIAN_POINT('Ctrl Pts',(-50.6038678242843,-71.6594078470244,
175.490142808619));
#38843=CARTESIAN_POINT('Ctrl Pts',(-50.4097844795482,-71.774379656781,177.134243841043));
#38844=CARTESIAN_POINT('Ctrl Pts',(-51.4314621824798,-71.7597432164852,
178.441881219107));
#38845=CARTESIAN_POINT('Ctrl Pts',(-52.4531398854114,-71.7451067761894,
179.74951859717));
#38846=CARTESIAN_POINT('Ctrl Pts',(-54.0979152764806,-71.6640439594884,
179.954696079469));
#38847=CARTESIAN_POINT('Ctrl Pts',(-55.7426906675498,-71.5829811427874,
180.159873561769));
#38848=CARTESIAN_POINT('Ctrl Pts',(-57.0528982121988,-71.5375854937271,
179.142400961866));
#38849=CARTESIAN_POINT('Ctrl Pts',(-58.3631057568478,-71.4921898446669,
178.124928361964));
#38850=CARTESIAN_POINT('Ctrl Pts',(-58.5770652274179,-71.563661564221,176.48082732954));
#38851=CARTESIAN_POINT('Ctrl Pts',(-58.791024697988,-71.6351332837751,174.836726297116));
#38852=CARTESIAN_POINT('Ctrl Pts',(-57.7892231208904,-71.8362132533815,
173.529088919052));
#38853=CARTESIAN_POINT('Ctrl Pts',(-56.7874215437929,-72.037293222988,172.221451540989));
#38854=CARTESIAN_POINT('Ctrl Pts',(-55.1625222785577,-72.3047995689997,
172.016274058689));
#38855=CARTESIAN_POINT('Ctrl Pts',(-53.5376230133225,-72.5723059150115,
171.81109657639));
#38856=CARTESIAN_POINT('Ctrl Pts',(-52.2472915945075,-72.8041450933824,
172.828569176292));
#38857=CARTESIAN_POINT('Ctrl Pts',(-50.9569601756925,-73.0359842717533,
173.846041776195));
#38858=CARTESIAN_POINT('Ctrl Pts',(-50.7628768309565,-73.1509560815099,
175.490142808619));
#38859=CARTESIAN_POINT('Ctrl Pts',(-50.5687934862204,-73.2659278912666,
177.134243841043));
#38860=CARTESIAN_POINT('Ctrl Pts',(-51.590471189152,-73.2512914509708,178.441881219107));
#38861=CARTESIAN_POINT('Ctrl Pts',(-52.6121488920836,-73.236655010675,179.74951859717));
#38862=CARTESIAN_POINT('Ctrl Pts',(-54.2569242831528,-73.155592193974,179.954696079469));
#38863=CARTESIAN_POINT('Ctrl Pts',(-55.901699674222,-73.074529377273,180.159873561769));
#38864=CARTESIAN_POINT('Ctrl Pts',(-57.211907218871,-73.0291337282128,179.142400961866));
#38865=CARTESIAN_POINT('Ctrl Pts',(-58.5221147635201,-72.9837380791525,
178.124928361964));
#38866=CARTESIAN_POINT('Ctrl Pts',(-58.7360742340901,-73.0552097987066,
176.48082732954));
#38867=CARTESIAN_POINT('Ctrl Pts',(-58.9500337046602,-73.1266815182607,
174.836726297116));
#38868=CARTESIAN_POINT('Ctrl Pts',(-57.9482321275626,-73.3277614878671,
173.529088919052));
#38869=CARTESIAN_POINT('Ctrl Pts',(-56.9464305504651,-73.5288414574736,
172.221451540989));
#38870=CARTESIAN_POINT('Ctrl Pts',(-55.3215312852299,-73.7963478034854,
172.016274058689));
#38871=CARTESIAN_POINT('Ctrl Pts',(-53.6966320199948,-74.0638541494971,
171.81109657639));
#38872=CARTESIAN_POINT('Ctrl Pts',(-52.4063006011798,-74.295693327868,172.828569176292));
#38873=CARTESIAN_POINT('Ctrl Pts',(-51.1159691823648,-74.5275325062389,
173.846041776195));
#38874=CARTESIAN_POINT('Ctrl Pts',(-50.9218858376287,-74.6425043159955,
175.490142808619));
#38875=CARTESIAN_POINT('Ctrl Pts',(-50.7278024928926,-74.7574761257522,
177.134243841043));
#38876=CARTESIAN_POINT('Ctrl Pts',(-51.7494801958242,-74.7428396854564,
178.441881219107));
#38877=CARTESIAN_POINT('Ctrl Pts',(-52.7711578987559,-74.7282032451606,
179.74951859717));
#38878=CARTESIAN_POINT('Ctrl Pts',(-54.415933289825,-74.6471404284596,179.954696079469));
#38879=CARTESIAN_POINT('Ctrl Pts',(-56.0607086808942,-74.5660776117586,
180.159873561769));
#38880=CARTESIAN_POINT('Ctrl Pts',(-57.3709162255433,-74.5206819626983,
179.142400961866));
#38881=CARTESIAN_POINT('Ctrl Pts',(-58.6811237701923,-74.4752863136381,
178.124928361964));
#38882=CARTESIAN_POINT('Ctrl Pts',(-58.8950832407624,-74.5467580331922,
176.48082732954));
#38883=CARTESIAN_POINT('Ctrl Pts',(-59.1090427113324,-74.6182297527463,
174.836726297116));
#38884=CARTESIAN_POINT('Ctrl Pts',(-58.1072411342349,-74.8193097223528,
173.529088919052));
#38885=CARTESIAN_POINT('Ctrl Pts',(-57.1054395571373,-75.0203896919592,
172.221451540989));
#38886=CARTESIAN_POINT('Ctrl Pts',(-55.4805402919021,-75.287896037971,172.016274058689));
#38887=CARTESIAN_POINT('Ctrl Pts',(-53.855641026667,-75.5554023839827,171.81109657639));
#38888=CARTESIAN_POINT('Ctrl Pts',(-52.565309607852,-75.7872415623536,172.828569176292));
#38889=CARTESIAN_POINT('Ctrl Pts',(-51.274978189037,-76.0190807407245,173.846041776195));
#38890=CARTESIAN_POINT('Ctrl Pts',(-51.0808948443009,-76.1340525504811,
175.490142808619));
#38891=CARTESIAN_POINT('Ctrl Pts',(-50.8868114995649,-76.2490243602378,
177.134243841043));
#38892=CARTESIAN_POINT('Ctrl Pts',(-51.9084892024965,-76.234387919942,178.441881219107));
#38893=CARTESIAN_POINT('Ctrl Pts',(-52.9301669054281,-76.2197514796462,
179.74951859717));
#38894=CARTESIAN_POINT('Ctrl Pts',(-54.5749422964973,-76.1386886629452,
179.954696079469));
#38895=CARTESIAN_POINT('Ctrl Pts',(-56.2197176875665,-76.0576258462442,
180.159873561769));
#38896=CARTESIAN_POINT('Ctrl Pts',(-57.5299252322155,-76.012230197184,179.142400961866));
#38897=CARTESIAN_POINT('Ctrl Pts',(-58.8401327768645,-75.9668345481237,
178.124928361964));
#38898=CARTESIAN_POINT('Ctrl Pts',(-59.0540922474346,-76.0383062676778,
176.48082732954));
#38899=CARTESIAN_POINT('Ctrl Pts',(-59.2680517180047,-76.1097779872319,
174.836726297116));
#38900=CARTESIAN_POINT('Ctrl Pts',(-58.2662501409071,-76.3108579568383,
173.529088919052));
#38901=CARTESIAN_POINT('Ctrl Pts',(-57.2644485638095,-76.5119379264448,
172.221451540989));
#38902=CARTESIAN_POINT('Ctrl Pts',(-55.6395492985744,-76.7794442724566,
172.016274058689));
#38903=CARTESIAN_POINT('Ctrl Pts',(-54.0146500333392,-77.0469506184683,
171.81109657639));
#38904=CARTESIAN_POINT('Ctrl Pts',(-52.7243186145242,-77.2787897968392,
172.828569176292));
#38905=CARTESIAN_POINT('Ctrl Pts',(-51.4339871957092,-77.5106289752101,
173.846041776195));
#38906=CARTESIAN_POINT('Ctrl Pts',(-51.2399038509732,-77.6256007849667,
175.490142808619));
#38907=CARTESIAN_POINT('Ctrl Pts',(-51.0458205062371,-77.7405725947234,
177.134243841043));
#38908=CARTESIAN_POINT('Ctrl Pts',(-52.0674982091687,-77.7259361544276,
178.441881219107));
#38909=CARTESIAN_POINT('Ctrl Pts',(-53.0891759121003,-77.7112997141318,
179.74951859717));
#38910=CARTESIAN_POINT('Ctrl Pts',(-54.7339513031695,-77.6302368974308,
179.954696079469));
#38911=CARTESIAN_POINT('Ctrl Pts',(-56.3787266942387,-77.5491740807298,
180.159873561769));
#38912=CARTESIAN_POINT('Ctrl Pts',(-57.6889342388877,-77.5037784316696,
179.142400961866));
#38913=CARTESIAN_POINT('Ctrl Pts',(-58.9991417835367,-77.4583827826093,
178.124928361964));
#38914=CARTESIAN_POINT('Ctrl Pts',(-59.2131012541068,-77.5298545021634,
176.48082732954));
#38915=CARTESIAN_POINT('Ctrl Pts',(-59.4270607246769,-77.6013262217175,
174.836726297116));
#38916=CARTESIAN_POINT('Ctrl Pts',(-58.4252591475793,-77.802406191324,173.529088919052));
#38917=CARTESIAN_POINT('Ctrl Pts',(-57.4234575704818,-78.0034861609304,
172.221451540989));
#38918=CARTESIAN_POINT('Ctrl Pts',(-55.7985583052466,-78.2709925069422,
172.016274058689));
#38919=CARTESIAN_POINT('Ctrl Pts',(-54.1736590400114,-78.5384988529539,
171.81109657639));
#38920=CARTESIAN_POINT('Ctrl Pts',(-52.8833276211964,-78.7703380313248,
172.828569176292));
#38921=CARTESIAN_POINT('Ctrl Pts',(-51.5929962023814,-79.0021772096957,
173.846041776195));
#38922=CARTESIAN_POINT('Ctrl Pts',(-51.3989128576454,-79.1171490194523,
175.490142808619));
#38923=CARTESIAN_POINT('Ctrl Pts',(-51.2048295129093,-79.232120829209,177.134243841043));
#38924=CARTESIAN_POINT('Ctrl Pts',(-52.2265072158409,-79.2174843889132,
178.441881219107));
#38925=CARTESIAN_POINT('Ctrl Pts',(-53.2481849187725,-79.2028479486174,
179.74951859717));
#38926=CARTESIAN_POINT('Ctrl Pts',(-54.8929603098417,-79.1217851319164,
179.954696079469));
#38927=CARTESIAN_POINT('Ctrl Pts',(-56.5377357009109,-79.0407223152154,
180.159873561769));
#38928=CARTESIAN_POINT('Ctrl Pts',(-57.8479432455599,-78.9953266661552,
179.142400961866));
#38929=CARTESIAN_POINT('Ctrl Pts',(-59.158150790209,-78.9499310170949,178.124928361964));
#38930=CARTESIAN_POINT('Ctrl Pts',(-59.372110260779,-79.021402736649,176.48082732954));
#38931=CARTESIAN_POINT('Ctrl Pts',(-59.5860697313491,-79.0928744562031,
174.836726297116));
#38932=CARTESIAN_POINT('Ctrl Pts',(-58.5842681542516,-79.2939544258096,
173.529088919052));
#38933=CARTESIAN_POINT('Ctrl Pts',(-57.582466577154,-79.495034395416,172.221451540989));
#38934=CARTESIAN_POINT('Ctrl Pts',(-55.9575673119188,-79.7625407414277,
172.016274058689));
#38935=CARTESIAN_POINT('Ctrl Pts',(-54.3326680466837,-80.0300470874395,
171.81109657639));
#38936=CARTESIAN_POINT('Ctrl Pts',(-53.0423366278687,-80.2618862658104,
172.828569176292));
#38937=CARTESIAN_POINT('Ctrl Pts',(-51.7520052090537,-80.4937254441813,
173.846041776195));
#38938=CARTESIAN_POINT('Ctrl Pts',(-51.5579218643176,-80.6086972539379,
175.490142808619));
#38939=CARTESIAN_POINT('Ctrl Pts',(-51.3638385195816,-80.7236690636945,
177.134243841043));
#38940=CARTESIAN_POINT('Ctrl Pts',(-52.3855162225132,-80.7090326233988,
178.441881219107));
#38941=CARTESIAN_POINT('Ctrl Pts',(-53.4071939254448,-80.694396183103,179.74951859717));
#38942=CARTESIAN_POINT('Ctrl Pts',(-55.0519693165139,-80.613333366402,179.954696079469));
#38943=CARTESIAN_POINT('Ctrl Pts',(-56.6967447075831,-80.532270549701,180.159873561769));
#38944=CARTESIAN_POINT('Ctrl Pts',(-58.0069522522322,-80.4868749006407,
179.142400961866));
#38945=CARTESIAN_POINT('Ctrl Pts',(-59.3171597968812,-80.4414792515805,
178.124928361964));
#38946=CARTESIAN_POINT('Ctrl Pts',(-59.5311192674513,-80.5129509711346,
176.48082732954));
#38947=CARTESIAN_POINT('Ctrl Pts',(-59.7450787380214,-80.5844226906887,
174.836726297116));
#38948=CARTESIAN_POINT('Ctrl Pts',(-58.7432771609238,-80.7855026602952,
173.529088919052));
#38949=CARTESIAN_POINT('Ctrl Pts',(-57.7414755838262,-80.9865826299016,
172.221451540989));
#38950=CARTESIAN_POINT('Ctrl Pts',(-56.116576318591,-81.2540889759133,172.016274058689));
#38951=CARTESIAN_POINT('Ctrl Pts',(-54.4916770533559,-81.5215953219251,
171.81109657639));
#38952=CARTESIAN_POINT('Ctrl Pts',(-53.2013456345409,-81.753434500296,172.828569176292));
#38953=CARTESIAN_POINT('Ctrl Pts',(-51.9110142157259,-81.9852736786669,
173.846041776195));
#38954=CARTESIAN_POINT('Ctrl Pts',(-51.7169308709898,-82.1002454884235,
175.490142808619));
#38955=CARTESIAN_POINT('Ctrl Pts',(-51.5228475262538,-82.2152172981801,
177.134243841043));
#38956=CARTESIAN_POINT('Ctrl Pts',(-52.5445252291854,-82.2005808578844,
178.441881219107));
#38957=CARTESIAN_POINT('Ctrl Pts',(-53.566202932117,-82.1859444175886,179.74951859717));
#38958=CARTESIAN_POINT('Ctrl Pts',(-55.2109783231862,-82.1048816008876,
179.954696079469));
#38959=CARTESIAN_POINT('Ctrl Pts',(-56.8557537142554,-82.0238187841866,
180.159873561769));
#38960=CARTESIAN_POINT('Ctrl Pts',(-58.1659612589044,-81.9784231351264,
179.142400961866));
#38961=CARTESIAN_POINT('Ctrl Pts',(-59.4761688035534,-81.9330274860661,
178.124928361964));
#38962=CARTESIAN_POINT('Ctrl Pts',(-59.6901282741235,-82.0044992056202,
176.48082732954));
#38963=CARTESIAN_POINT('Ctrl Pts',(-59.9040877446936,-82.0759709251743,
174.836726297116));
#38964=CARTESIAN_POINT('Ctrl Pts',(-58.902286167596,-82.2770508947808,173.529088919052));
#38965=CARTESIAN_POINT('Ctrl Pts',(-57.9004845904984,-82.4781308643872,
172.221451540989));
#38966=CARTESIAN_POINT('Ctrl Pts',(-56.2755853252633,-82.745637210399,172.016274058689));
#38967=CARTESIAN_POINT('Ctrl Pts',(-54.6506860600281,-83.0131435564107,
171.81109657639));
#38968=CARTESIAN_POINT('Ctrl Pts',(-53.3603546412131,-83.2449827347816,
172.828569176292));
#38969=CARTESIAN_POINT('Ctrl Pts',(-52.0700232223981,-83.4768219131525,
173.846041776195));
#38970=CARTESIAN_POINT('Ctrl Pts',(-51.8759398776621,-83.5917937229092,
175.490142808619));
#38971=CARTESIAN_POINT('Ctrl Pts',(-51.681856532926,-83.7067655326658,177.134243841043));
#38972=CARTESIAN_POINT('Ctrl Pts',(-52.7035342358576,-83.69212909237,178.441881219107));
#38973=CARTESIAN_POINT('Ctrl Pts',(-53.7252119387892,-83.6774926520742,
179.74951859717));
#38974=CARTESIAN_POINT('Ctrl Pts',(-55.3699873298584,-83.5964298353732,
179.954696079469));
#38975=CARTESIAN_POINT('Ctrl Pts',(-57.0147627209276,-83.5153670186722,
180.159873561769));
#38976=CARTESIAN_POINT('Ctrl Pts',(-58.3249702655766,-83.469971369612,179.142400961866));
#38977=CARTESIAN_POINT('Ctrl Pts',(-59.6351778102256,-83.4245757205517,
178.124928361964));
#38978=CARTESIAN_POINT('Ctrl Pts',(-59.8491372807957,-83.4960474401058,
176.48082732954));
#38979=CARTESIAN_POINT('Ctrl Pts',(-60.0630967513658,-83.5675191596599,
174.836726297116));
#38980=CARTESIAN_POINT('Ctrl Pts',(-59.0612951742682,-83.7685991292663,
173.529088919052));
#38981=CARTESIAN_POINT('Ctrl Pts',(-58.0594935971707,-83.9696790988728,
172.221451540989));
#38982=CARTESIAN_POINT('Ctrl Pts',(-56.4345943319355,-84.2371854448845,
172.016274058689));
#38983=CARTESIAN_POINT('Ctrl Pts',(-54.8096950667003,-84.5046917908963,
171.81109657639));
#38984=CARTESIAN_POINT('Ctrl Pts',(-53.5193636478853,-84.7365309692672,
172.828569176292));
#38985=CARTESIAN_POINT('Ctrl Pts',(-52.2290322290704,-84.9683701476381,
173.846041776195));
#38986=CARTESIAN_POINT('Ctrl Pts',(-52.0349488843343,-85.0833419573947,
175.490142808619));
#38987=CARTESIAN_POINT('Ctrl Pts',(-51.8408655395982,-85.1983137671513,
177.134243841043));
#38988=CARTESIAN_POINT('Ctrl Pts',(-52.8625432425298,-85.1836773268556,
178.441881219107));
#38989=CARTESIAN_POINT('Ctrl Pts',(-53.8842209454614,-85.1690408865598,
179.74951859717));
#38990=CARTESIAN_POINT('Ctrl Pts',(-55.5289963365306,-85.0879780698588,
179.954696079469));
#38991=CARTESIAN_POINT('Ctrl Pts',(-57.1737717275998,-85.0069152531578,
180.159873561769));
#38992=CARTESIAN_POINT('Ctrl Pts',(-58.4839792722488,-84.9615196040975,
179.142400961866));
#38993=CARTESIAN_POINT('Ctrl Pts',(-59.7941868168979,-84.9161239550373,
178.124928361964));
#38994=CARTESIAN_POINT('Ctrl Pts',(-60.008146287468,-84.9875956745914,176.48082732954));
#38995=CARTESIAN_POINT('Ctrl Pts',(-60.222105758038,-85.0590673941455,174.836726297116));
#38996=CARTESIAN_POINT('Ctrl Pts',(-59.2203041809405,-85.260147363752,173.529088919052));
#38997=CARTESIAN_POINT('Ctrl Pts',(-58.2185026038429,-85.4612273333584,
172.221451540989));
#38998=CARTESIAN_POINT('Ctrl Pts',(-56.5936033386077,-85.7287336793702,
172.016274058689));
#38999=CARTESIAN_POINT('Ctrl Pts',(-54.9687040733726,-85.9962400253819,
171.81109657639));
#39000=CARTESIAN_POINT('Ctrl Pts',(-53.6783726545576,-86.2280792037528,
172.828569176292));
#39001=CARTESIAN_POINT('Ctrl Pts',(-52.3880412357426,-86.4599183821237,
173.846041776195));
#39002=CARTESIAN_POINT('Ctrl Pts',(-52.1939578910065,-86.5748901918803,
175.490142808619));
#39003=CARTESIAN_POINT('Ctrl Pts',(-51.9998745462705,-86.689862001637,177.134243841043));
#39004=CARTESIAN_POINT('Ctrl Pts',(-53.0215522492021,-86.6752255613412,
178.441881219107));
#39005=CARTESIAN_POINT('Ctrl Pts',(-54.0432299521337,-86.6605891210454,
179.74951859717));
#39006=CARTESIAN_POINT('Ctrl Pts',(-55.6880053432029,-86.5795263043444,
179.954696079469));
#39007=CARTESIAN_POINT('Ctrl Pts',(-57.3327807342721,-86.4984634876434,
180.159873561769));
#39008=CARTESIAN_POINT('Ctrl Pts',(-58.6429882789211,-86.4530678385832,
179.142400961866));
#39009=CARTESIAN_POINT('Ctrl Pts',(-59.9531958235701,-86.4076721895229,
178.124928361964));
#39010=CARTESIAN_POINT('Ctrl Pts',(-60.1671552941402,-86.479143909077,176.48082732954));
#39011=CARTESIAN_POINT('Ctrl Pts',(-60.3811147647103,-86.5506156286311,
174.836726297116));
#39012=CARTESIAN_POINT('Ctrl Pts',(-59.3793131876127,-86.7516955982376,
173.529088919052));
#39013=CARTESIAN_POINT('Ctrl Pts',(-58.3775116105151,-86.952775567844,172.221451540989));
#39014=CARTESIAN_POINT('Ctrl Pts',(-56.7526123452799,-87.2202819138558,
172.016274058689));
#39015=CARTESIAN_POINT('Ctrl Pts',(-55.1277130800448,-87.4877882598675,
171.81109657639));
#39016=CARTESIAN_POINT('Ctrl Pts',(-53.8373816612298,-87.7196274382384,
172.828569176292));
#39017=CARTESIAN_POINT('Ctrl Pts',(-52.5470502424148,-87.9514666166093,
173.846041776195));
#39018=CARTESIAN_POINT('Ctrl Pts',(-52.3529668976787,-88.0664384263659,
175.490142808619));
#39019=CARTESIAN_POINT('Ctrl Pts',(-52.1588835529427,-88.1814102361226,
177.134243841043));
#39020=CARTESIAN_POINT('Ctrl Pts',(-53.1805612558743,-88.1667737958268,
178.441881219107));
#39021=CARTESIAN_POINT('Ctrl Pts',(-54.2022389588059,-88.152137355531,179.74951859717));
#39022=CARTESIAN_POINT('Ctrl Pts',(-55.8470143498751,-88.07107453883,179.954696079469));
#39023=CARTESIAN_POINT('Ctrl Pts',(-57.4917897409443,-87.990011722129,180.159873561769));
#39024=CARTESIAN_POINT('Ctrl Pts',(-58.8019972855933,-87.9446160730687,
179.142400961866));
#39025=CARTESIAN_POINT('Ctrl Pts',(-60.1122048302423,-87.8992204240085,
178.124928361964));
#39026=CARTESIAN_POINT('Ctrl Pts',(-60.3261643008124,-87.9706921435626,
176.48082732954));
#39027=CARTESIAN_POINT('Ctrl Pts',(-60.5401237713825,-88.0421638631167,
174.836726297116));
#39028=CARTESIAN_POINT('Ctrl Pts',(-59.5383221942849,-88.2432438327232,
173.529088919052));
#39029=CARTESIAN_POINT('Ctrl Pts',(-58.5365206171873,-88.4443238023296,
172.221451540989));
#39030=CARTESIAN_POINT('Ctrl Pts',(-56.9116213519522,-88.7118301483414,
172.016274058689));
#39031=CARTESIAN_POINT('Ctrl Pts',(-55.286722086717,-88.9793364943531,171.81109657639));
#39032=CARTESIAN_POINT('Ctrl Pts',(-53.996390667902,-89.211175672724,172.828569176292));
#39033=CARTESIAN_POINT('Ctrl Pts',(-52.706059249087,-89.4430148510949,173.846041776195));
#39034=CARTESIAN_POINT('Ctrl Pts',(-52.511975904351,-89.5579866608516,175.490142808619));
#39035=CARTESIAN_POINT('Ctrl Pts',(-52.3178925596149,-89.6729584706082,
177.134243841043));
#39036=CARTESIAN_POINT('Ctrl Pts',(-53.3395702625465,-89.6583220303124,
178.441881219107));
#39037=CARTESIAN_POINT('Ctrl Pts',(-54.3612479654781,-89.6436855900166,
179.74951859717));
#39038=CARTESIAN_POINT('Ctrl Pts',(-56.0060233565473,-89.5626227733156,
179.954696079469));
#39039=CARTESIAN_POINT('Ctrl Pts',(-57.6507987476165,-89.4815599566146,
180.159873561769));
#39040=CARTESIAN_POINT('Ctrl Pts',(-58.9610062922655,-89.4361643075543,
179.142400961866));
#39041=CARTESIAN_POINT('Ctrl Pts',(-60.2712138369146,-89.3907686584941,
178.124928361964));
#39042=CARTESIAN_POINT('Ctrl Pts',(-60.4851733074846,-89.4622403780482,
176.48082732954));
#39043=CARTESIAN_POINT('Ctrl Pts',(-60.6991327780547,-89.5337120976023,
174.836726297116));
#39044=CARTESIAN_POINT('Ctrl Pts',(-59.6973312009571,-89.7347920672087,
173.529088919052));
#39045=CARTESIAN_POINT('Ctrl Pts',(-58.6955296238596,-89.9358720368152,
172.221451540989));
#39046=CARTESIAN_POINT('Ctrl Pts',(-57.0706303586244,-90.203378382827,172.016274058689));
#39047=CARTESIAN_POINT('Ctrl Pts',(-55.4457310933893,-90.4708847288387,
171.81109657639));
#39048=CARTESIAN_POINT('Ctrl Pts',(-54.1553996745743,-90.7027239072096,
172.828569176292));
#39049=CARTESIAN_POINT('Ctrl Pts',(-52.8650682557593,-90.9345630855805,
173.846041776195));
#39050=CARTESIAN_POINT('Ctrl Pts',(-52.6709849110232,-91.0495348953371,
175.490142808619));
#39051=CARTESIAN_POINT('Ctrl Pts',(-52.4769015662871,-91.1645067050938,
177.134243841043));
#39052=CARTESIAN_POINT('Ctrl Pts',(-53.4985792692187,-91.149870264798,178.441881219107));
#39053=CARTESIAN_POINT('Ctrl Pts',(-54.5202569721503,-91.1352338245022,
179.74951859717));
#39054=CARTESIAN_POINT('Ctrl Pts',(-56.1650323632195,-91.0541710078012,
179.954696079469));
#39055=CARTESIAN_POINT('Ctrl Pts',(-57.8098077542887,-90.9731081911002,
180.159873561769));
#39056=CARTESIAN_POINT('Ctrl Pts',(-59.1200152989378,-90.92771254204,179.142400961866));
#39057=CARTESIAN_POINT('Ctrl Pts',(-60.4302228435868,-90.8823168929797,
178.124928361964));
#39058=CARTESIAN_POINT('Ctrl Pts',(-60.6441823141569,-90.9537886125338,
176.48082732954));
#39059=CARTESIAN_POINT('Ctrl Pts',(-60.858141784727,-91.0252603320879,174.836726297116));
#39060=CARTESIAN_POINT('Ctrl Pts',(-59.8563402076294,-91.2263403016943,
173.529088919052));
#39061=CARTESIAN_POINT('Ctrl Pts',(-58.8545386305318,-91.4274202713008,
172.221451540989));
#39062=CARTESIAN_POINT('Ctrl Pts',(-57.2296393652966,-91.6949266173126,
172.016274058689));
#39063=CARTESIAN_POINT('Ctrl Pts',(-55.6047401000615,-91.9624329633243,
171.81109657639));
#39064=CARTESIAN_POINT('Ctrl Pts',(-54.3144086812465,-92.1942721416952,
172.828569176292));
#39065=CARTESIAN_POINT('Ctrl Pts',(-53.0240772624315,-92.4261113200661,
173.846041776195));
#39066=CARTESIAN_POINT('Ctrl Pts',(-52.8299939176954,-92.5410831298227,
175.490142808619));
#39067=CARTESIAN_POINT('Ctrl Pts',(-52.6359105729594,-92.6560549395793,
177.134243841043));
#39068=CARTESIAN_POINT('Ctrl Pts',(-53.657588275891,-92.6414184992836,178.441881219107));
#39069=CARTESIAN_POINT('Ctrl Pts',(-54.6792659788226,-92.6267820589878,
179.74951859717));
#39070=CARTESIAN_POINT('Ctrl Pts',(-56.3240413698918,-92.5457192422868,
179.954696079469));
#39071=CARTESIAN_POINT('Ctrl Pts',(-57.968816760961,-92.4646564255858,180.159873561769));
#39072=CARTESIAN_POINT('Ctrl Pts',(-59.27902430561,-92.4192607765256,179.142400961866));
#39073=CARTESIAN_POINT('Ctrl Pts',(-60.589231850259,-92.3738651274653,178.124928361964));
#39074=CARTESIAN_POINT('Ctrl Pts',(-60.8031913208291,-92.4453368470194,
176.48082732954));
#39075=CARTESIAN_POINT('Ctrl Pts',(-61.0171507913992,-92.5168085665735,
174.836726297116));
#39076=CARTESIAN_POINT('Ctrl Pts',(-60.0153492143016,-92.71788853618,173.529088919052));
#39077=CARTESIAN_POINT('Ctrl Pts',(-59.013547637204,-92.9189685057864,172.221451540989));
#39078=CARTESIAN_POINT('Ctrl Pts',(-57.3886483719689,-93.1864748517982,
172.016274058689));
#39079=CARTESIAN_POINT('Ctrl Pts',(-55.7637491067337,-93.4539811978099,
171.81109657639));
#39080=CARTESIAN_POINT('Ctrl Pts',(-54.4734176879187,-93.6858203761808,
172.828569176292));
#39081=CARTESIAN_POINT('Ctrl Pts',(-53.1830862691037,-93.9176595545517,
173.846041776195));
#39082=CARTESIAN_POINT('Ctrl Pts',(-52.9890029243677,-94.0326313643084,
175.490142808619));
#39083=CARTESIAN_POINT('Ctrl Pts',(-52.7949195796316,-94.147603174065,177.134243841043));
#39084=CARTESIAN_POINT('Ctrl Pts',(-53.8165972825632,-94.1329667337692,
178.441881219107));
#39085=CARTESIAN_POINT('Ctrl Pts',(-54.8382749854948,-94.1183302934734,
179.74951859717));
#39086=CARTESIAN_POINT('Ctrl Pts',(-56.483050376564,-94.0372674767724,179.954696079469));
#39087=CARTESIAN_POINT('Ctrl Pts',(-58.1278257676332,-93.9562046600714,
180.159873561769));
#39088=CARTESIAN_POINT('Ctrl Pts',(-59.4380333122822,-93.9108090110112,
179.142400961866));
#39089=CARTESIAN_POINT('Ctrl Pts',(-60.7482408569312,-93.8654133619509,
178.124928361964));
#39090=CARTESIAN_POINT('Ctrl Pts',(-60.9622003275013,-93.936885081505,176.48082732954));
#39091=CARTESIAN_POINT('Ctrl Pts',(-61.1761597980714,-94.0083568010591,
174.836726297116));
#39092=CARTESIAN_POINT('Ctrl Pts',(-60.1743582209738,-94.2094367706656,
173.529088919052));
#39093=CARTESIAN_POINT('Ctrl Pts',(-59.1725566438763,-94.4105167402721,
172.221451540989));
#39094=CARTESIAN_POINT('Ctrl Pts',(-57.5476573786411,-94.6780230862838,
172.016274058689));
#39095=CARTESIAN_POINT('Ctrl Pts',(-55.9227581134059,-94.9455294322955,
171.81109657639));
#39096=CARTESIAN_POINT('Ctrl Pts',(-54.6324266945909,-95.1773686106664,
172.828569176292));
#39097=CARTESIAN_POINT('Ctrl Pts',(-53.3420952757759,-95.4092077890373,
173.846041776195));
#39098=CARTESIAN_POINT('Ctrl Pts',(-53.1480119310399,-95.5241795987939,
175.490142808619));
#39099=CARTESIAN_POINT('Ctrl Pts',(-52.9539285863038,-95.6391514085506,
177.134243841043));
#39100=CARTESIAN_POINT('Ctrl Pts',(-53.9756062892354,-95.6245149682548,
178.441881219107));
#39101=CARTESIAN_POINT('Ctrl Pts',(-54.997283992167,-95.609878527959,179.74951859717));
#39102=CARTESIAN_POINT('Ctrl Pts',(-56.6420593832362,-95.528815711258,179.954696079469));
#39103=CARTESIAN_POINT('Ctrl Pts',(-58.2868347743054,-95.447752894557,180.159873561769));
#39104=CARTESIAN_POINT('Ctrl Pts',(-59.5970423189544,-95.4023572454968,
179.142400961866));
#39105=CARTESIAN_POINT('Ctrl Pts',(-60.9072498636035,-95.3569615964365,
178.124928361964));
#39106=CARTESIAN_POINT('Ctrl Pts',(-61.1212093341735,-95.4284333159906,
176.48082732954));
#39107=CARTESIAN_POINT('Ctrl Pts',(-61.3351688047436,-95.4999050355447,
174.836726297116));
#39108=CARTESIAN_POINT('Ctrl Pts',(-60.3333672276461,-95.7009850051512,
173.529088919052));
#39109=CARTESIAN_POINT('Ctrl Pts',(-59.3315656505485,-95.9020649747577,
172.221451540989));
#39110=CARTESIAN_POINT('Ctrl Pts',(-57.7066663853133,-96.1695713207694,
172.016274058689));
#39111=CARTESIAN_POINT('Ctrl Pts',(-56.0817671200782,-96.4370776667811,
171.81109657639));
#39112=CARTESIAN_POINT('Ctrl Pts',(-54.7914357012632,-96.668916845152,172.828569176292));
#39113=CARTESIAN_POINT('Ctrl Pts',(-53.5011042824482,-96.9007560235229,
173.846041776195));
#39114=CARTESIAN_POINT('Ctrl Pts',(-53.3070209377121,-97.0157278332795,
175.490142808619));
#39115=CARTESIAN_POINT('Ctrl Pts',(-53.1129375929761,-97.1306996430362,
177.134243841043));
#39116=CARTESIAN_POINT('Ctrl Pts',(-54.1346152959077,-97.1160632027404,
178.441881219107));
#39117=CARTESIAN_POINT('Ctrl Pts',(-55.1562929988393,-97.1014267624446,
179.74951859717));
#39118=CARTESIAN_POINT('Ctrl Pts',(-56.8010683899085,-97.0203639457436,
179.954696079469));
#39119=CARTESIAN_POINT('Ctrl Pts',(-58.4458437809776,-96.9393011290426,
180.159873561769));
#39120=CARTESIAN_POINT('Ctrl Pts',(-59.7560513256267,-96.8939054799824,
179.142400961866));
#39121=CARTESIAN_POINT('Ctrl Pts',(-61.0662588702757,-96.8485098309222,
178.124928361964));
#39122=CARTESIAN_POINT('Ctrl Pts',(-61.2802183408458,-96.9199815504762,
176.48082732954));
#39123=CARTESIAN_POINT('Ctrl Pts',(-61.4941778114159,-96.9914532700303,
174.836726297116));
#39124=CARTESIAN_POINT('Ctrl Pts',(-60.4923762343183,-97.1925332396368,
173.529088919052));
#39125=CARTESIAN_POINT('Ctrl Pts',(-59.4905746572207,-97.3936132092432,
172.221451540989));
#39126=CARTESIAN_POINT('Ctrl Pts',(-57.8656753919855,-97.661119555255,172.016274058689));
#39127=CARTESIAN_POINT('Ctrl Pts',(-56.2407761267504,-97.9286259012667,
171.81109657639));
#39128=CARTESIAN_POINT('Ctrl Pts',(-54.9504447079354,-98.1604650796376,
172.828569176292));
#39129=CARTESIAN_POINT('Ctrl Pts',(-53.6601132891204,-98.3923042580085,
173.846041776195));
#39130=CARTESIAN_POINT('Ctrl Pts',(-53.4660299443843,-98.5072760677652,
175.490142808619));
#39131=CARTESIAN_POINT('Ctrl Pts',(-53.2719465996483,-98.6222478775218,
177.134243841043));
#39132=CARTESIAN_POINT('Ctrl Pts',(-54.2936243025799,-98.607611437226,178.441881219107));
#39133=CARTESIAN_POINT('Ctrl Pts',(-55.3153020055115,-98.5929749969302,
179.74951859717));
#39134=CARTESIAN_POINT('Ctrl Pts',(-56.9600773965807,-98.5119121802292,
179.954696079469));
#39135=CARTESIAN_POINT('Ctrl Pts',(-58.6048527876499,-98.4308493635282,
180.159873561769));
#39136=CARTESIAN_POINT('Ctrl Pts',(-59.9150603322989,-98.385453714468,179.142400961866));
#39137=CARTESIAN_POINT('Ctrl Pts',(-61.2252678769479,-98.3400580654078,
178.124928361964));
#39138=CARTESIAN_POINT('Ctrl Pts',(-61.439227347518,-98.4115297849618,176.48082732954));
#39139=CARTESIAN_POINT('Ctrl Pts',(-61.6531868180881,-98.4830015045159,
174.836726297116));
#39140=CARTESIAN_POINT('Ctrl Pts',(-60.6513852409905,-98.6840814741224,
173.529088919052));
#39141=CARTESIAN_POINT('Ctrl Pts',(-59.6495836638929,-98.8851614437288,
172.221451540989));
#39142=CARTESIAN_POINT('Ctrl Pts',(-58.0246843986578,-99.1526677897406,
172.016274058689));
#39143=CARTESIAN_POINT('Ctrl Pts',(-56.3997851334226,-99.4201741357523,
171.81109657639));
#39144=CARTESIAN_POINT('Ctrl Pts',(-55.1094537146076,-99.6520133141232,
172.828569176292));
#39145=CARTESIAN_POINT('Ctrl Pts',(-53.8191222957926,-99.8838524924941,
173.846041776195));
#39146=CARTESIAN_POINT('Ctrl Pts',(-53.6250389510566,-99.9988243022507,
175.490142808619));
#39147=CARTESIAN_POINT('Ctrl Pts',(-53.4309556063205,-100.113796112007,
177.134243841043));
#39148=CARTESIAN_POINT('Ctrl Pts',(-54.4526333092521,-100.099159671712,
178.441881219107));
#39149=CARTESIAN_POINT('Ctrl Pts',(-55.4743110121837,-100.084523231416,
179.74951859717));
#39150=CARTESIAN_POINT('Ctrl Pts',(-57.1190864032529,-100.003460414715,
179.954696079469));
#39151=CARTESIAN_POINT('Ctrl Pts',(-58.7638617943221,-99.9223975980138,
180.159873561769));
#39152=CARTESIAN_POINT('Ctrl Pts',(-60.0740693389711,-99.8770019489536,
179.142400961866));
#39153=CARTESIAN_POINT('Ctrl Pts',(-61.3842768836201,-99.8316062998934,
178.124928361964));
#39154=CARTESIAN_POINT('Ctrl Pts',(-61.5982363541902,-99.9030780194474,
176.48082732954));
#39155=CARTESIAN_POINT('Ctrl Pts',(-61.8121958247603,-99.9745497390015,
174.836726297116));
#39156=CARTESIAN_POINT('Ctrl Pts',(-60.8103942476627,-100.175629708608,
173.529088919052));
#39157=CARTESIAN_POINT('Ctrl Pts',(-59.8085926705652,-100.376709678214,
172.221451540989));
#39158=CARTESIAN_POINT('Ctrl Pts',(-58.18369340533,-100.644216024226,172.016274058689));
#39159=CARTESIAN_POINT('Ctrl Pts',(-56.5587941400948,-100.911722370238,
171.81109657639));
#39160=CARTESIAN_POINT('Ctrl Pts',(-55.2684627212798,-101.143561548609,
172.828569176292));
#39161=CARTESIAN_POINT('Ctrl Pts',(-53.9781313024648,-101.37540072698,173.846041776195));
#39162=CARTESIAN_POINT('Ctrl Pts',(-53.7840479577288,-101.490372536736,
175.490142808619));
#39163=CARTESIAN_POINT('Ctrl Pts',(-53.5899646129927,-101.605344346493,
177.134243841043));
#39164=CARTESIAN_POINT('Ctrl Pts',(-54.6116423159243,-101.590707906197,
178.441881219107));
#39165=CARTESIAN_POINT('Ctrl Pts',(-55.6333200188559,-101.576071465901,
179.74951859717));
#39166=CARTESIAN_POINT('Ctrl Pts',(-57.2780954099251,-101.4950086492,179.954696079469));
#39167=CARTESIAN_POINT('Ctrl Pts',(-58.9228708009943,-101.413945832499,
180.159873561769));
#39168=CARTESIAN_POINT('Ctrl Pts',(-60.2330783456433,-101.368550183439,
179.142400961866));
#39169=CARTESIAN_POINT('Ctrl Pts',(-61.5432858902924,-101.323154534379,
178.124928361964));
#39170=CARTESIAN_POINT('Ctrl Pts',(-61.7572453608625,-101.394626253933,
176.48082732954));
#39171=CARTESIAN_POINT('Ctrl Pts',(-61.9712048314325,-101.466097973487,
174.836726297116));
#39172=CARTESIAN_POINT('Ctrl Pts',(-60.969403254335,-101.667177943094,173.529088919052));
#39173=CARTESIAN_POINT('Ctrl Pts',(-59.9676016772374,-101.8682579127,172.221451540989));
#39174=CARTESIAN_POINT('Ctrl Pts',(-58.3427024120022,-102.135764258712,
172.016274058689));
#39175=CARTESIAN_POINT('Ctrl Pts',(-56.7178031467671,-102.403270604724,
171.81109657639));
#39176=CARTESIAN_POINT('Ctrl Pts',(-55.4274717279521,-102.635109783094,
172.828569176292));
#39177=CARTESIAN_POINT('Ctrl Pts',(-54.1371403091371,-102.866948961465,
173.846041776195));
#39178=CARTESIAN_POINT('Ctrl Pts',(-53.943056964401,-102.981920771222,175.490142808619));
#39179=CARTESIAN_POINT('Ctrl Pts',(-53.748973619665,-103.096892580979,177.134243841043));
#39180=CARTESIAN_POINT('Ctrl Pts',(-54.7706513225966,-103.082256140683,
178.441881219107));
#39181=CARTESIAN_POINT('Ctrl Pts',(-55.7923290255282,-103.067619700387,
179.74951859717));
#39182=CARTESIAN_POINT('Ctrl Pts',(-57.4371044165974,-102.986556883686,
179.954696079469));
#39183=CARTESIAN_POINT('Ctrl Pts',(-59.0818798076666,-102.905494066985,
180.159873561769));
#39184=CARTESIAN_POINT('Ctrl Pts',(-60.3920873523156,-102.860098417925,
179.142400961866));
#39185=CARTESIAN_POINT('Ctrl Pts',(-61.7022948969646,-102.814702768865,
178.124928361964));
#39186=CARTESIAN_POINT('Ctrl Pts',(-61.9162543675347,-102.886174488419,
176.48082732954));
#39187=CARTESIAN_POINT('Ctrl Pts',(-62.1302138381048,-102.957646207973,
174.836726297116));
#39188=CARTESIAN_POINT('Ctrl Pts',(-61.1284122610072,-103.158726177579,
173.529088919052));
#39189=CARTESIAN_POINT('Ctrl Pts',(-60.1266106839096,-103.359806147186,
172.221451540989));
#39190=CARTESIAN_POINT('Ctrl Pts',(-58.5017114186745,-103.627312493197,
172.016274058689));
#39191=CARTESIAN_POINT('Ctrl Pts',(-56.8768121534393,-103.894818839209,
171.81109657639));
#39192=CARTESIAN_POINT('Ctrl Pts',(-55.5864807346243,-104.12665801758,172.828569176292));
#39193=CARTESIAN_POINT('Ctrl Pts',(-54.2961493158093,-104.358497195951,
173.846041776195));
#39194=CARTESIAN_POINT('Ctrl Pts',(-54.1020659710732,-104.473469005708,
175.490142808619));
#39195=CARTESIAN_POINT('Ctrl Pts',(-53.9079826263372,-104.588440815464,
177.134243841043));
#39196=CARTESIAN_POINT('Ctrl Pts',(-54.9296603292688,-104.573804375168,
178.441881219107));
#39197=CARTESIAN_POINT('Ctrl Pts',(-55.9513380322004,-104.559167934873,
179.74951859717));
#39198=CARTESIAN_POINT('Ctrl Pts',(-57.5961134232696,-104.478105118172,
179.954696079469));
#39199=CARTESIAN_POINT('Ctrl Pts',(-59.2408888143388,-104.397042301471,
180.159873561769));
#39200=CARTESIAN_POINT('Ctrl Pts',(-60.5510963589878,-104.35164665241,179.142400961866));
#39201=CARTESIAN_POINT('Ctrl Pts',(-61.8613039036368,-104.30625100335,178.124928361964));
#39202=CARTESIAN_POINT('Ctrl Pts',(-62.0752633742069,-104.377722722904,
176.48082732954));
#39203=CARTESIAN_POINT('Ctrl Pts',(-62.289222844777,-104.449194442458,174.836726297116));
#39204=CARTESIAN_POINT('Ctrl Pts',(-61.2874212676794,-104.650274412065,
173.529088919052));
#39205=CARTESIAN_POINT('Ctrl Pts',(-60.2856196905818,-104.851354381671,
172.221451540989));
#39206=CARTESIAN_POINT('Ctrl Pts',(-58.6607204253467,-105.118860727683,
172.016274058689));
#39207=CARTESIAN_POINT('Ctrl Pts',(-57.0358211601115,-105.386367073695,
171.81109657639));
#39208=CARTESIAN_POINT('Ctrl Pts',(-55.7454897412965,-105.618206252066,
172.828569176292));
#39209=CARTESIAN_POINT('Ctrl Pts',(-54.4551583224815,-105.850045430437,
173.846041776195));
#39210=CARTESIAN_POINT('Ctrl Pts',(-54.2610749777455,-105.965017240193,
175.490142808619));
#39211=CARTESIAN_POINT('Ctrl Pts',(-54.0669916330094,-106.07998904995,177.134243841043));
#39212=CARTESIAN_POINT('Ctrl Pts',(-55.088669335941,-106.065352609654,178.441881219107));
#39213=CARTESIAN_POINT('Ctrl Pts',(-56.1103470388726,-106.050716169358,
179.74951859717));
#39214=CARTESIAN_POINT('Ctrl Pts',(-57.7551224299418,-105.969653352657,
179.954696079469));
#39215=CARTESIAN_POINT('Ctrl Pts',(-59.399897821011,-105.888590535956,180.159873561769));
#39216=CARTESIAN_POINT('Ctrl Pts',(-60.71010536566,-105.843194886896,179.142400961866));
#39217=CARTESIAN_POINT('Ctrl Pts',(-62.0203129103091,-105.797799237836,
178.124928361964));
#39218=CARTESIAN_POINT('Ctrl Pts',(-62.2342723808791,-105.86927095739,176.48082732954));
#39219=CARTESIAN_POINT('Ctrl Pts',(-62.4482318514492,-105.940742676944,
174.836726297116));
#39220=CARTESIAN_POINT('Ctrl Pts',(-61.4464302743516,-106.14182264655,173.529088919052));
#39221=CARTESIAN_POINT('Ctrl Pts',(-60.4446286972541,-106.342902616157,
172.221451540989));
#39222=CARTESIAN_POINT('Ctrl Pts',(-58.8197294320189,-106.610408962169,
172.016274058689));
#39223=CARTESIAN_POINT('Ctrl Pts',(-57.1948301667837,-106.87791530818,171.81109657639));
#39224=CARTESIAN_POINT('Ctrl Pts',(-55.9044987479688,-107.109754486551,
172.828569176292));
#39225=CARTESIAN_POINT('Ctrl Pts',(-54.6141673291538,-107.341593664922,
173.846041776195));
#39226=CARTESIAN_POINT('Ctrl Pts',(-54.4200839844177,-107.456565474679,
175.490142808619));
#39227=CARTESIAN_POINT('Ctrl Pts',(-54.2260006396817,-107.571537284435,
177.134243841043));
#39228=CARTESIAN_POINT('Ctrl Pts',(-55.2476783426132,-107.55690084414,178.441881219107));
#39229=CARTESIAN_POINT('Ctrl Pts',(-56.2693560455449,-107.542264403844,
179.74951859717));
#39230=CARTESIAN_POINT('Ctrl Pts',(-57.914131436614,-107.461201587143,179.954696079469));
#39231=CARTESIAN_POINT('Ctrl Pts',(-59.5589068276832,-107.380138770442,
180.159873561769));
#39232=CARTESIAN_POINT('Ctrl Pts',(-60.8691143723323,-107.334743121382,
179.142400961866));
#39233=CARTESIAN_POINT('Ctrl Pts',(-62.1793219169813,-107.289347472321,
178.124928361964));
#39234=CARTESIAN_POINT('Ctrl Pts',(-62.3932813875514,-107.360819191875,
176.48082732954));
#39235=CARTESIAN_POINT('Ctrl Pts',(-62.6072408581214,-107.43229091143,174.836726297116));
#39236=CARTESIAN_POINT('Ctrl Pts',(-61.6054392810239,-107.633370881036,
173.529088919052));
#39237=CARTESIAN_POINT('Ctrl Pts',(-60.6036377039263,-107.834450850642,
172.221451540989));
#39238=CARTESIAN_POINT('Ctrl Pts',(-58.9787384386911,-108.101957196654,
172.016274058689));
#39239=CARTESIAN_POINT('Ctrl Pts',(-57.353839173456,-108.369463542666,171.81109657639));
#39240=CARTESIAN_POINT('Ctrl Pts',(-56.063507754641,-108.601302721037,172.828569176292));
#39241=CARTESIAN_POINT('Ctrl Pts',(-54.773176335826,-108.833141899408,173.846041776195));
#39242=CARTESIAN_POINT('Ctrl Pts',(-54.5790929910899,-108.948113709164,
175.490142808619));
#39243=CARTESIAN_POINT('Ctrl Pts',(-54.3850096463539,-109.063085518921,
177.134243841043));
#39244=CARTESIAN_POINT('Ctrl Pts',(-55.4066873492855,-109.048449078625,
178.441881219107));
#39245=CARTESIAN_POINT('Ctrl Pts',(-56.4283650522171,-109.033812638329,
179.74951859717));
#39246=CARTESIAN_POINT('Ctrl Pts',(-58.0731404432863,-108.952749821628,
179.954696079469));
#39247=CARTESIAN_POINT('Ctrl Pts',(-59.7179158343555,-108.871687004927,
180.159873561769));
#39248=CARTESIAN_POINT('Ctrl Pts',(-61.0281233790045,-108.826291355867,
179.142400961866));
#39249=CARTESIAN_POINT('Ctrl Pts',(-62.3383309236535,-108.780895706807,
178.124928361964));
#39250=CARTESIAN_POINT('Ctrl Pts',(-62.5522903942236,-108.852367426361,
176.48082732954));
#39251=CARTESIAN_POINT('Ctrl Pts',(-62.7662498647937,-108.923839145915,
174.836726297116));
#39252=CARTESIAN_POINT('Ctrl Pts',(-61.7644482876961,-109.124919115522,
173.529088919052));
#39253=CARTESIAN_POINT('Ctrl Pts',(-60.7626467105985,-109.325999085128,
172.221451540989));
#39254=CARTESIAN_POINT('Ctrl Pts',(-59.1377474453634,-109.59350543114,172.016274058689));
#39255=CARTESIAN_POINT('Ctrl Pts',(-57.5128481801282,-109.861011777151,
171.81109657639));
#39256=CARTESIAN_POINT('Ctrl Pts',(-56.2225167613132,-110.092850955522,
172.828569176292));
#39257=CARTESIAN_POINT('Ctrl Pts',(-54.9321853424982,-110.324690133893,
173.846041776195));
#39258=CARTESIAN_POINT('Ctrl Pts',(-54.7381019977622,-110.43966194365,175.490142808619));
#39259=CARTESIAN_POINT('Ctrl Pts',(-54.5440186530261,-110.554633753407,
177.134243841043));
#39260=CARTESIAN_POINT('Ctrl Pts',(-55.5656963559577,-110.539997313111,
178.441881219107));
#39261=CARTESIAN_POINT('Ctrl Pts',(-56.5873740588893,-110.525360872815,
179.74951859717));
#39262=CARTESIAN_POINT('Ctrl Pts',(-58.2321494499585,-110.444298056114,
179.954696079469));
#39263=CARTESIAN_POINT('Ctrl Pts',(-59.8769248410277,-110.363235239413,
180.159873561769));
#39264=CARTESIAN_POINT('Ctrl Pts',(-61.1871323856767,-110.317839590353,
179.142400961866));
#39265=CARTESIAN_POINT('Ctrl Pts',(-62.4973399303257,-110.272443941293,
178.124928361964));
#39266=CARTESIAN_POINT('Ctrl Pts',(-62.7112994008958,-110.343915660847,
176.48082732954));
#39267=CARTESIAN_POINT('Ctrl Pts',(-62.9252588714659,-110.415387380401,
174.836726297116));
#39268=CARTESIAN_POINT('Ctrl Pts',(-61.9234572943683,-110.616467350007,
173.529088919052));
#39269=CARTESIAN_POINT('Ctrl Pts',(-60.9216557172708,-110.817547319614,
172.221451540989));
#39270=CARTESIAN_POINT('Ctrl Pts',(-59.2967564520356,-111.085053665625,
172.016274058689));
#39271=CARTESIAN_POINT('Ctrl Pts',(-57.6718571868004,-111.352560011637,
171.81109657639));
#39272=CARTESIAN_POINT('Ctrl Pts',(-56.3815257679854,-111.584399190008,
172.828569176292));
#39273=CARTESIAN_POINT('Ctrl Pts',(-55.0911943491704,-111.816238368379,
173.846041776195));
#39274=CARTESIAN_POINT('Ctrl Pts',(-54.8971110044344,-111.931210178136,
175.490142808619));
#39275=CARTESIAN_POINT('Ctrl Pts',(-54.7030276596983,-112.046181987892,
177.134243841043));
#39276=CARTESIAN_POINT('Ctrl Pts',(-55.7247053626299,-112.031545547596,
178.441881219107));
#39277=CARTESIAN_POINT('Ctrl Pts',(-56.7463830655615,-112.016909107301,
179.74951859717));
#39278=CARTESIAN_POINT('Ctrl Pts',(-58.3911584566307,-111.9358462906,179.954696079469));
#39279=CARTESIAN_POINT('Ctrl Pts',(-60.0359338476999,-111.854783473899,
180.159873561769));
#39280=CARTESIAN_POINT('Ctrl Pts',(-61.3461413923489,-111.809387824838,
179.142400961866));
#39281=CARTESIAN_POINT('Ctrl Pts',(-62.656348936998,-111.763992175778,178.124928361964));
#39282=CARTESIAN_POINT('Ctrl Pts',(-62.870308407568,-111.835463895332,176.48082732954));
#39283=CARTESIAN_POINT('Ctrl Pts',(-63.0842678781381,-111.906935614886,
174.836726297116));
#39284=CARTESIAN_POINT('Ctrl Pts',(-62.0824663010406,-112.108015584493,
173.529088919052));
#39285=CARTESIAN_POINT('Ctrl Pts',(-61.080664723943,-112.309095554099,172.221451540989));
#39286=CARTESIAN_POINT('Ctrl Pts',(-59.4557654587078,-112.576601900111,
172.016274058689));
#39287=CARTESIAN_POINT('Ctrl Pts',(-57.8308661934727,-112.844108246123,
171.81109657639));
#39288=CARTESIAN_POINT('Ctrl Pts',(-56.5405347746577,-113.075947424494,
172.828569176292));
#39289=CARTESIAN_POINT('Ctrl Pts',(-55.2502033558427,-113.307786602865,
173.846041776195));
#39290=CARTESIAN_POINT('Ctrl Pts',(-55.0561200111066,-113.422758412621,
175.490142808619));
#39291=CARTESIAN_POINT('Ctrl Pts',(-54.8620366663706,-113.537730222378,
177.134243841043));
#39292=CARTESIAN_POINT('Ctrl Pts',(-55.8837143693022,-113.523093782082,
178.441881219107));
#39293=CARTESIAN_POINT('Ctrl Pts',(-56.9053920722338,-113.508457341786,
179.74951859717));
#39294=CARTESIAN_POINT('Ctrl Pts',(-58.550167463303,-113.427394525085,179.954696079469));
#39295=CARTESIAN_POINT('Ctrl Pts',(-60.1949428543721,-113.346331708384,
180.159873561769));
#39296=CARTESIAN_POINT('Ctrl Pts',(-61.5051503990212,-113.300936059324,
179.142400961866));
#39297=CARTESIAN_POINT('Ctrl Pts',(-62.8153579436702,-113.255540410264,
178.124928361964));
#39298=CARTESIAN_POINT('Ctrl Pts',(-63.0293174142403,-113.327012129818,
176.48082732954));
#39299=CARTESIAN_POINT('Ctrl Pts',(-63.2432768848103,-113.398483849372,
174.836726297116));
#39300=CARTESIAN_POINT('Ctrl Pts',(-62.2414753077128,-113.599563818978,
173.529088919052));
#39301=CARTESIAN_POINT('Ctrl Pts',(-61.2396737306152,-113.800643788585,
172.221451540989));
#39302=CARTESIAN_POINT('Ctrl Pts',(-59.6147744653801,-114.068150134597,
172.016274058689));
#39303=CARTESIAN_POINT('Ctrl Pts',(-57.9898752001449,-114.335656480608,
171.81109657639));
#39304=CARTESIAN_POINT('Ctrl Pts',(-56.6995437813299,-114.567495658979,
172.828569176292));
#39305=CARTESIAN_POINT('Ctrl Pts',(-55.4092123625149,-114.79933483735,173.846041776195));
#39306=CARTESIAN_POINT('Ctrl Pts',(-55.2151290177788,-114.914306647107,
175.490142808619));
#39307=CARTESIAN_POINT('Ctrl Pts',(-55.0210456730428,-115.029278456863,
177.134243841043));
#39308=CARTESIAN_POINT('Ctrl Pts',(-56.0427233759744,-115.014642016568,
178.441881219107));
#39309=CARTESIAN_POINT('Ctrl Pts',(-57.064401078906,-115.000005576272,179.74951859717));
#39310=CARTESIAN_POINT('Ctrl Pts',(-58.7091764699752,-114.918942759571,
179.954696079469));
#39311=CARTESIAN_POINT('Ctrl Pts',(-60.3539518610444,-114.83787994287,180.159873561769));
#39312=CARTESIAN_POINT('Ctrl Pts',(-61.6641594056934,-114.79248429381,179.142400961866));
#39313=CARTESIAN_POINT('Ctrl Pts',(-62.9743669503424,-114.747088644749,
178.124928361964));
#39314=CARTESIAN_POINT('Ctrl Pts',(-63.1883264209125,-114.818560364303,
176.48082732954));
#39315=CARTESIAN_POINT('Ctrl Pts',(-63.4022858914826,-114.890032083858,
174.836726297116));
#39316=CARTESIAN_POINT('Ctrl Pts',(-62.400484314385,-115.091112053464,173.529088919052));
#39317=CARTESIAN_POINT('Ctrl Pts',(-61.3986827372874,-115.29219202307,172.221451540989));
#39318=CARTESIAN_POINT('Ctrl Pts',(-59.7737834720523,-115.559698369082,
172.016274058689));
#39319=CARTESIAN_POINT('Ctrl Pts',(-58.1488842068171,-115.827204715094,
171.81109657639));
#39320=CARTESIAN_POINT('Ctrl Pts',(-56.8585527880021,-116.059043893465,
172.828569176292));
#39321=CARTESIAN_POINT('Ctrl Pts',(-55.5682213691871,-116.290883071836,
173.846041776195));
#39322=CARTESIAN_POINT('Ctrl Pts',(-55.3741380244511,-116.405854881592,
175.490142808619));
#39323=CARTESIAN_POINT('Ctrl Pts',(-55.180054679715,-116.520826691349,177.134243841043));
#39324=CARTESIAN_POINT('Ctrl Pts',(-56.2017323826466,-116.506190251053,
178.441881219107));
#39325=CARTESIAN_POINT('Ctrl Pts',(-57.2234100855782,-116.491553810757,
179.74951859717));
#39326=CARTESIAN_POINT('Ctrl Pts',(-58.8681854766474,-116.410490994056,
179.954696079469));
#39327=CARTESIAN_POINT('Ctrl Pts',(-60.5129608677166,-116.329428177355,
180.159873561769));
#39328=CARTESIAN_POINT('Ctrl Pts',(-61.8231684123656,-116.284032528295,
179.142400961866));
#39329=CARTESIAN_POINT('Ctrl Pts',(-63.1333759570147,-116.238636879235,
178.124928361964));
#39330=CARTESIAN_POINT('Ctrl Pts',(-63.3473354275847,-116.310108598789,
176.48082732954));
#39331=CARTESIAN_POINT('Ctrl Pts',(-63.5612948981548,-116.381580318343,
174.836726297116));
#39332=CARTESIAN_POINT('Ctrl Pts',(-62.5594933210572,-116.58266028795,173.529088919052));
#39333=CARTESIAN_POINT('Ctrl Pts',(-61.5576917439597,-116.783740257556,
172.221451540989));
#39334=CARTESIAN_POINT('Ctrl Pts',(-59.9327924787245,-117.051246603568,
172.016274058689));
#39335=CARTESIAN_POINT('Ctrl Pts',(-58.3078932134893,-117.318752949579,
171.81109657639));
#39336=CARTESIAN_POINT('Ctrl Pts',(-57.0175617946743,-117.55059212795,172.828569176292));
#39337=CARTESIAN_POINT('Ctrl Pts',(-55.7272303758593,-117.782431306321,
173.846041776195));
#39338=CARTESIAN_POINT('Ctrl Pts',(-55.5331470311233,-117.897403116078,
175.490142808619));
#39339=CARTESIAN_POINT('Ctrl Pts',(-55.3390636863872,-118.012374925835,
177.134243841043));
#39340=CARTESIAN_POINT('Ctrl Pts',(-56.3607413893188,-117.997738485539,
178.441881219107));
#39341=CARTESIAN_POINT('Ctrl Pts',(-57.3824190922504,-117.983102045243,
179.74951859717));
#39342=CARTESIAN_POINT('Ctrl Pts',(-59.0271944833196,-117.902039228542,
179.954696079469));
#39343=CARTESIAN_POINT('Ctrl Pts',(-60.6719698743888,-117.820976411841,
180.159873561769));
#39344=CARTESIAN_POINT('Ctrl Pts',(-61.9821774190378,-117.775580762781,
179.142400961866));
#39345=CARTESIAN_POINT('Ctrl Pts',(-63.2923849636869,-117.730185113721,
178.124928361964));
#39346=CARTESIAN_POINT('Ctrl Pts',(-63.506344434257,-117.801656833275,176.48082732954));
#39347=CARTESIAN_POINT('Ctrl Pts',(-63.720303904827,-117.873128552829,174.836726297116));
#39348=CARTESIAN_POINT('Ctrl Pts',(-62.7185023277295,-118.074208522435,
173.529088919052));
#39349=CARTESIAN_POINT('Ctrl Pts',(-61.7167007506319,-118.275288492042,
172.221451540989));
#39350=CARTESIAN_POINT('Ctrl Pts',(-60.0918014853967,-118.542794838053,
172.016274058689));
#39351=CARTESIAN_POINT('Ctrl Pts',(-58.4669022201616,-118.810301184065,
171.81109657639));
#39352=CARTESIAN_POINT('Ctrl Pts',(-57.1765708013466,-119.042140362436,
172.828569176292));
#39353=CARTESIAN_POINT('Ctrl Pts',(-55.8862393825316,-119.273979540807,
173.846041776195));
#39354=CARTESIAN_POINT('Ctrl Pts',(-55.6921560377955,-119.388951350564,
175.490142808619));
#39355=CARTESIAN_POINT('Ctrl Pts',(-55.4980726930595,-119.50392316032,177.134243841043));
#39356=CARTESIAN_POINT('Ctrl Pts',(-56.5197503959911,-119.489286720024,
178.441881219107));
#39357=CARTESIAN_POINT('Ctrl Pts',(-57.5414280989227,-119.474650279729,
179.74951859717));
#39358=CARTESIAN_POINT('Ctrl Pts',(-59.1862034899919,-119.393587463028,
179.954696079469));
#39359=CARTESIAN_POINT('Ctrl Pts',(-60.8309788810611,-119.312524646327,
180.159873561769));
#39360=CARTESIAN_POINT('Ctrl Pts',(-62.1411864257101,-119.267128997266,
179.142400961866));
#39361=CARTESIAN_POINT('Ctrl Pts',(-63.4513939703591,-119.221733348206,
178.124928361964));
#39362=CARTESIAN_POINT('Ctrl Pts',(-63.6653534409292,-119.29320506776,176.48082732954));
#39363=CARTESIAN_POINT('Ctrl Pts',(-63.8793129114993,-119.364676787314,
174.836726297116));
#39364=CARTESIAN_POINT('Ctrl Pts',(-62.8775113344017,-119.565756756921,
173.529088919052));
#39365=CARTESIAN_POINT('Ctrl Pts',(-61.8757097573041,-119.766836726527,
172.221451540989));
#39366=CARTESIAN_POINT('Ctrl Pts',(-60.250810492069,-120.034343072539,172.016274058689));
#39367=CARTESIAN_POINT('Ctrl Pts',(-58.6259112268338,-120.301849418551,
171.81109657639));
#39368=CARTESIAN_POINT('Ctrl Pts',(-57.3355798080188,-120.533688596922,
172.828569176292));
#39369=CARTESIAN_POINT('Ctrl Pts',(-56.0452483892038,-120.765527775293,
173.846041776195));
#39370=CARTESIAN_POINT('Ctrl Pts',(-55.8511650444677,-120.880499585049,
175.490142808619));
#39371=CARTESIAN_POINT('Ctrl Pts',(-55.6570816997317,-120.995471394806,
177.134243841043));
#39372=CARTESIAN_POINT('Ctrl Pts',(-56.6787594026633,-120.98083495451,178.441881219107));
#39373=CARTESIAN_POINT('Ctrl Pts',(-57.7004371055949,-120.966198514214,
179.74951859717));
#39374=CARTESIAN_POINT('Ctrl Pts',(-59.3452124966641,-120.885135697513,
179.954696079469));
#39375=CARTESIAN_POINT('Ctrl Pts',(-60.9899878877333,-120.804072880812,
180.159873561769));
#39376=CARTESIAN_POINT('Ctrl Pts',(-62.3001954323823,-120.758677231752,
179.142400961866));
#39377=CARTESIAN_POINT('Ctrl Pts',(-63.6104029770313,-120.713281582692,
178.124928361964));
#39378=CARTESIAN_POINT('Ctrl Pts',(-63.8243624476014,-120.784753302246,
176.48082732954));
#39379=CARTESIAN_POINT('Ctrl Pts',(-64.0383219181715,-120.8562250218,174.836726297116));
#39380=CARTESIAN_POINT('Ctrl Pts',(-63.0365203410739,-121.057304991406,
173.529088919052));
#39381=CARTESIAN_POINT('Ctrl Pts',(-62.0347187639764,-121.258384961013,
172.221451540989));
#39382=CARTESIAN_POINT('Ctrl Pts',(-60.4098194987412,-121.525891307025,
172.016274058689));
#39383=CARTESIAN_POINT('Ctrl Pts',(-58.784920233506,-121.793397653036,171.81109657639));
#39384=CARTESIAN_POINT('Ctrl Pts',(-57.494588814691,-122.025236831407,172.828569176292));
#39385=CARTESIAN_POINT('Ctrl Pts',(-56.204257395876,-122.257076009778,173.846041776195));
#39386=CARTESIAN_POINT('Ctrl Pts',(-56.01017405114,-122.372047819535,175.490142808619));
#39387=CARTESIAN_POINT('Ctrl Pts',(-55.8160907064039,-122.487019629291,
177.134243841043));
#39388=CARTESIAN_POINT('Ctrl Pts',(-56.8377684093355,-122.472383188996,
178.441881219107));
#39389=CARTESIAN_POINT('Ctrl Pts',(-57.8594461122671,-122.4577467487,179.74951859717));
#39390=CARTESIAN_POINT('Ctrl Pts',(-59.5042215033363,-122.376683931999,
179.954696079469));
#39391=CARTESIAN_POINT('Ctrl Pts',(-61.1489968944055,-122.295621115298,
180.159873561769));
#39392=CARTESIAN_POINT('Ctrl Pts',(-62.4592044390545,-122.250225466238,
179.142400961866));
#39393=CARTESIAN_POINT('Ctrl Pts',(-63.7694119837035,-122.204829817177,
178.124928361964));
#39394=CARTESIAN_POINT('Ctrl Pts',(-63.9833714542736,-122.276301536731,
176.48082732954));
#39395=CARTESIAN_POINT('Ctrl Pts',(-64.1973309248437,-122.347773256285,
174.836726297116));
#39396=CARTESIAN_POINT('Ctrl Pts',(-63.1955293477461,-122.548853225892,
173.529088919052));
#39397=CARTESIAN_POINT('Ctrl Pts',(-62.1937277706486,-122.749933195498,
172.221451540989));
#39398=CARTESIAN_POINT('Ctrl Pts',(-60.5688285054134,-123.01743954151,172.016274058689));
#39399=CARTESIAN_POINT('Ctrl Pts',(-58.9439292401782,-123.284945887522,
171.81109657639));
#39400=CARTESIAN_POINT('Ctrl Pts',(-57.6535978213633,-123.516785065893,
172.828569176292));
#39401=CARTESIAN_POINT('Ctrl Pts',(-56.3632664025483,-123.748624244264,
173.846041776195));
#39402=CARTESIAN_POINT('Ctrl Pts',(-56.1691830578122,-123.86359605402,175.490142808619));
#39403=CARTESIAN_POINT('Ctrl Pts',(-55.9750997130761,-123.978567863777,
177.134243841043));
#39404=CARTESIAN_POINT('Ctrl Pts',(-56.9967774160077,-123.963931423481,
178.441881219107));
#39405=CARTESIAN_POINT('Ctrl Pts',(-58.0184551189394,-123.949294983185,
179.74951859717));
#39406=CARTESIAN_POINT('Ctrl Pts',(-59.6632305100085,-123.868232166484,
179.954696079469));
#39407=CARTESIAN_POINT('Ctrl Pts',(-61.3080059010777,-123.787169349783,
180.159873561769));
#39408=CARTESIAN_POINT('Ctrl Pts',(-62.6182134457268,-123.741773700723,
179.142400961866));
#39409=CARTESIAN_POINT('Ctrl Pts',(-63.9284209903758,-123.696378051663,
178.124928361964));
#39410=CARTESIAN_POINT('Ctrl Pts',(-64.1423804609459,-123.767849771217,
176.48082732954));
#39411=CARTESIAN_POINT('Ctrl Pts',(-64.3563399315159,-123.839321490771,
174.836726297116));
#39412=CARTESIAN_POINT('Ctrl Pts',(-63.3545383544184,-124.040401460378,
173.529088919052));
#39413=CARTESIAN_POINT('Ctrl Pts',(-62.3527367773208,-124.241481429984,
172.221451540989));
#39414=CARTESIAN_POINT('Ctrl Pts',(-60.7278375120856,-124.508987775996,
172.016274058689));
#39415=CARTESIAN_POINT('Ctrl Pts',(-59.1029382468505,-124.776494122007,
171.81109657639));
#39416=CARTESIAN_POINT('Ctrl Pts',(-57.8126068280355,-125.008333300378,
172.828569176292));
#39417=CARTESIAN_POINT('Ctrl Pts',(-56.5222754092205,-125.240172478749,
173.846041776195));
#39418=CARTESIAN_POINT('Ctrl Pts',(-56.3281920644844,-125.355144288506,
175.490142808619));
#39419=CARTESIAN_POINT('Ctrl Pts',(-56.1341087197484,-125.470116098263,
177.134243841043));
#39420=CARTESIAN_POINT('Ctrl Pts',(-57.15578642268,-125.455479657967,178.441881219107));
#39421=CARTESIAN_POINT('Ctrl Pts',(-58.1774641256116,-125.440843217671,
179.74951859717));
#39422=CARTESIAN_POINT('Ctrl Pts',(-59.8222395166808,-125.35978040097,179.954696079469));
#39423=CARTESIAN_POINT('Ctrl Pts',(-61.46701490775,-125.278717584269,180.159873561769));
#39424=CARTESIAN_POINT('Ctrl Pts',(-62.777222452399,-125.233321935209,179.142400961866));
#39425=CARTESIAN_POINT('Ctrl Pts',(-64.087429997048,-125.187926286149,178.124928361964));
#39426=CARTESIAN_POINT('Ctrl Pts',(-64.3013894676181,-125.259398005703,
176.48082732954));
#39427=CARTESIAN_POINT('Ctrl Pts',(-64.5153489381882,-125.330869725257,
174.836726297116));
#39428=CARTESIAN_POINT('Ctrl Pts',(-63.5135473610906,-125.531949694863,
173.529088919052));
#39429=CARTESIAN_POINT('Ctrl Pts',(-62.511745783993,-125.73302966447,172.221451540989));
#39430=CARTESIAN_POINT('Ctrl Pts',(-60.8868465187579,-126.000536010481,
172.016274058689));
#39431=CARTESIAN_POINT('Ctrl Pts',(-59.2619472535227,-126.268042356493,
171.81109657639));
#39432=CARTESIAN_POINT('Ctrl Pts',(-57.9716158347077,-126.499881534864,
172.828569176292));
#39433=CARTESIAN_POINT('Ctrl Pts',(-56.6812844158927,-126.731720713235,
173.846041776195));
#39434=CARTESIAN_POINT('Ctrl Pts',(-56.4872010711566,-126.846692522992,
175.490142808619));
#39435=CARTESIAN_POINT('Ctrl Pts',(-56.2931177264206,-126.961664332748,
177.134243841043));
#39436=CARTESIAN_POINT('Ctrl Pts',(-57.3147954293522,-126.947027892452,
178.441881219107));
#39437=CARTESIAN_POINT('Ctrl Pts',(-58.3364731322838,-126.932391452157,
179.74951859717));
#39438=CARTESIAN_POINT('Ctrl Pts',(-59.981248523353,-126.851328635456,179.954696079469));
#39439=CARTESIAN_POINT('Ctrl Pts',(-61.6260239144222,-126.770265818755,
180.159873561769));
#39440=CARTESIAN_POINT('Ctrl Pts',(-62.9362314590712,-126.724870169694,
179.142400961866));
#39441=CARTESIAN_POINT('Ctrl Pts',(-64.2464390037202,-126.679474520634,
178.124928361964));
#39442=CARTESIAN_POINT('Ctrl Pts',(-64.4603984742903,-126.750946240188,
176.48082732954));
#39443=CARTESIAN_POINT('Ctrl Pts',(-64.5291885105023,-126.7739250883,175.952232968864));
#39444=CARTESIAN_POINT('Ctrl Pts',(-64.4583706077394,-126.814016540979,
175.424797521489));
#39445=CARTESIAN_POINT('Ctrl Pts',(-50.179840660106,-67.6819454430842,175.490142424066));
#39446=CARTESIAN_POINT('Ctrl Pts',(-49.9857571569802,-67.7969172697262,
177.134244732869));
#39447=CARTESIAN_POINT('Ctrl Pts',(-51.0074356453643,-67.7822807456959,
178.441883126102));
#39448=CARTESIAN_POINT('Ctrl Pts',(-52.0291141337484,-67.7676442216657,
179.749521519335));
#39449=CARTESIAN_POINT('Ctrl Pts',(-53.6738907940049,-67.6865812696608,
179.954699160921));
#39450=CARTESIAN_POINT('Ctrl Pts',(-55.3186674542614,-67.6055183176559,
180.159876802508));
#39451=CARTESIAN_POINT('Ctrl Pts',(-56.6288760083597,-67.5601225609817,
179.142403412702));
#39452=CARTESIAN_POINT('Ctrl Pts',(-57.9390845624581,-67.5147268043074,
178.124930022896));
#39453=CARTESIAN_POINT('Ctrl Pts',(-58.1530441914179,-67.5861985069761,
176.480827714093));
#39454=CARTESIAN_POINT('Ctrl Pts',(-58.3670038203777,-67.6576702096448,
174.83672540529));
#39455=CARTESIAN_POINT('Ctrl Pts',(-57.3652014578276,-67.8587502629857,
173.529087012057));
#39456=CARTESIAN_POINT('Ctrl Pts',(-56.3633990952775,-68.0598303163267,
172.221448618824));
#39457=CARTESIAN_POINT('Ctrl Pts',(-54.7384985608551,-68.3273367976423,
172.016270977238));
#39458=CARTESIAN_POINT('Ctrl Pts',(-53.1135980264326,-68.5948432789578,
171.811093335651));
#39459=CARTESIAN_POINT('Ctrl Pts',(-51.8232655981683,-68.8266825649428,
172.828566725457));
#39460=CARTESIAN_POINT('Ctrl Pts',(-50.5329331699039,-69.0585218509277,
173.846040115263));
#39461=CARTESIAN_POINT('Ctrl Pts',(-50.3388496667782,-69.1734936775698,
175.490142424066));
#39462=CARTESIAN_POINT('Ctrl Pts',(-50.1447661636524,-69.2884655042118,
177.134244732869));
#39463=CARTESIAN_POINT('Ctrl Pts',(-51.1664446520366,-69.2738289801815,
178.441883126102));
#39464=CARTESIAN_POINT('Ctrl Pts',(-52.1881231404207,-69.2591924561513,
179.749521519335));
#39465=CARTESIAN_POINT('Ctrl Pts',(-53.8328998006771,-69.1781295041464,
179.954699160921));
#39466=CARTESIAN_POINT('Ctrl Pts',(-55.4776764609336,-69.0970665521415,
180.159876802508));
#39467=CARTESIAN_POINT('Ctrl Pts',(-56.787885015032,-69.0516707954673,179.142403412702));
#39468=CARTESIAN_POINT('Ctrl Pts',(-58.0980935691303,-69.006275038793,178.124930022896));
#39469=CARTESIAN_POINT('Ctrl Pts',(-58.3120531980901,-69.0777467414617,
176.480827714093));
#39470=CARTESIAN_POINT('Ctrl Pts',(-58.5260128270499,-69.1492184441304,
174.83672540529));
#39471=CARTESIAN_POINT('Ctrl Pts',(-57.5242104644998,-69.3502984974713,
173.529087012057));
#39472=CARTESIAN_POINT('Ctrl Pts',(-56.5224081019497,-69.5513785508123,
172.221448618824));
#39473=CARTESIAN_POINT('Ctrl Pts',(-54.8975075675273,-69.8188850321279,
172.016270977238));
#39474=CARTESIAN_POINT('Ctrl Pts',(-53.2726070331049,-70.0863915134434,
171.811093335651));
#39475=CARTESIAN_POINT('Ctrl Pts',(-51.9822746048405,-70.3182307994284,
172.828566725457));
#39476=CARTESIAN_POINT('Ctrl Pts',(-50.6919421765762,-70.5500700854134,
173.846040115263));
#39477=CARTESIAN_POINT('Ctrl Pts',(-50.4978586734504,-70.6650419120554,
175.490142424066));
#39478=CARTESIAN_POINT('Ctrl Pts',(-50.3037751703247,-70.7800137386974,
177.134244732869));
#39479=CARTESIAN_POINT('Ctrl Pts',(-51.3254536587088,-70.7653772146671,
178.441883126102));
#39480=CARTESIAN_POINT('Ctrl Pts',(-52.3471321470929,-70.7507406906369,
179.749521519335));
#39481=CARTESIAN_POINT('Ctrl Pts',(-53.9919088073493,-70.669677738632,179.954699160921));
#39482=CARTESIAN_POINT('Ctrl Pts',(-55.6366854676058,-70.5886147866271,
180.159876802508));
#39483=CARTESIAN_POINT('Ctrl Pts',(-56.9468940217042,-70.5432190299529,
179.142403412702));
#39484=CARTESIAN_POINT('Ctrl Pts',(-58.2571025758026,-70.4978232732786,
178.124930022896));
#39485=CARTESIAN_POINT('Ctrl Pts',(-58.4710622047623,-70.5692949759473,
176.480827714093));
#39486=CARTESIAN_POINT('Ctrl Pts',(-58.6850218337221,-70.640766678616,174.83672540529));
#39487=CARTESIAN_POINT('Ctrl Pts',(-57.683219471172,-70.8418467319569,173.529087012057));
#39488=CARTESIAN_POINT('Ctrl Pts',(-56.681417108622,-71.0429267852979,172.221448618824));
#39489=CARTESIAN_POINT('Ctrl Pts',(-55.0565165741995,-71.3104332666134,
172.016270977238));
#39490=CARTESIAN_POINT('Ctrl Pts',(-53.4316160397771,-71.577939747929,171.811093335651));
#39491=CARTESIAN_POINT('Ctrl Pts',(-52.1412836115127,-71.809779033914,172.828566725457));
#39492=CARTESIAN_POINT('Ctrl Pts',(-50.8509511832484,-72.0416183198989,
173.846040115263));
#39493=CARTESIAN_POINT('Ctrl Pts',(-50.6568676801226,-72.156590146541,175.490142424066));
#39494=CARTESIAN_POINT('Ctrl Pts',(-50.4627841769969,-72.271561973183,177.134244732869));
#39495=CARTESIAN_POINT('Ctrl Pts',(-51.484462665381,-72.2569254491527,178.441883126102));
#39496=CARTESIAN_POINT('Ctrl Pts',(-52.5061411537651,-72.2422889251225,
179.749521519335));
#39497=CARTESIAN_POINT('Ctrl Pts',(-54.1509178140216,-72.1612259731176,
179.954699160921));
#39498=CARTESIAN_POINT('Ctrl Pts',(-55.7956944742781,-72.0801630211127,
180.159876802508));
#39499=CARTESIAN_POINT('Ctrl Pts',(-57.1059030283764,-72.0347672644385,
179.142403412702));
#39500=CARTESIAN_POINT('Ctrl Pts',(-58.4161115824748,-71.9893715077642,
178.124930022896));
#39501=CARTESIAN_POINT('Ctrl Pts',(-58.6300712114346,-72.0608432104329,
176.480827714093));
#39502=CARTESIAN_POINT('Ctrl Pts',(-58.8440308403943,-72.1323149131016,
174.83672540529));
#39503=CARTESIAN_POINT('Ctrl Pts',(-57.8422284778443,-72.3333949664425,
173.529087012057));
#39504=CARTESIAN_POINT('Ctrl Pts',(-56.8404261152942,-72.5344750197835,
172.221448618824));
#39505=CARTESIAN_POINT('Ctrl Pts',(-55.2155255808718,-72.801981501099,172.016270977238));
#39506=CARTESIAN_POINT('Ctrl Pts',(-53.5906250464493,-73.0694879824146,
171.811093335651));
#39507=CARTESIAN_POINT('Ctrl Pts',(-52.300292618185,-73.3013272683996,172.828566725457));
#39508=CARTESIAN_POINT('Ctrl Pts',(-51.0099601899206,-73.5331665543845,
173.846040115263));
#39509=CARTESIAN_POINT('Ctrl Pts',(-50.8158766867949,-73.6481383810266,
175.490142424066));
#39510=CARTESIAN_POINT('Ctrl Pts',(-50.6217931836691,-73.7631102076686,
177.134244732869));
#39511=CARTESIAN_POINT('Ctrl Pts',(-51.6434716720532,-73.7484736836383,
178.441883126102));
#39512=CARTESIAN_POINT('Ctrl Pts',(-52.6651501604374,-73.7338371596081,
179.749521519335));
#39513=CARTESIAN_POINT('Ctrl Pts',(-54.3099268206938,-73.6527742076032,
179.954699160921));
#39514=CARTESIAN_POINT('Ctrl Pts',(-55.9547034809503,-73.5717112555984,
180.159876802508));
#39515=CARTESIAN_POINT('Ctrl Pts',(-57.2649120350486,-73.5263154989241,
179.142403412702));
#39516=CARTESIAN_POINT('Ctrl Pts',(-58.575120589147,-73.4809197422498,178.124930022896));
#39517=CARTESIAN_POINT('Ctrl Pts',(-58.7890802181068,-73.5523914449185,
176.480827714093));
#39518=CARTESIAN_POINT('Ctrl Pts',(-59.0030398470666,-73.6238631475872,
174.83672540529));
#39519=CARTESIAN_POINT('Ctrl Pts',(-58.0012374845165,-73.8249432009281,
173.529087012057));
#39520=CARTESIAN_POINT('Ctrl Pts',(-56.9994351219664,-74.0260232542691,
172.221448618824));
#39521=CARTESIAN_POINT('Ctrl Pts',(-55.374534587544,-74.2935297355847,172.016270977238));
#39522=CARTESIAN_POINT('Ctrl Pts',(-53.7496340531215,-74.5610362169002,
171.811093335651));
#39523=CARTESIAN_POINT('Ctrl Pts',(-52.4593016248572,-74.7928755028852,
172.828566725457));
#39524=CARTESIAN_POINT('Ctrl Pts',(-51.1689691965928,-75.0247147888702,
173.846040115263));
#39525=CARTESIAN_POINT('Ctrl Pts',(-50.9748856934671,-75.1396866155122,
175.490142424066));
#39526=CARTESIAN_POINT('Ctrl Pts',(-50.7808021903414,-75.2546584421542,
177.134244732869));
#39527=CARTESIAN_POINT('Ctrl Pts',(-51.8024806787255,-75.2400219181239,
178.441883126102));
#39528=CARTESIAN_POINT('Ctrl Pts',(-52.8241591671096,-75.2253853940937,
179.749521519335));
#39529=CARTESIAN_POINT('Ctrl Pts',(-54.468935827366,-75.1443224420888,179.954699160921));
#39530=CARTESIAN_POINT('Ctrl Pts',(-56.1137124876225,-75.0632594900839,
180.159876802508));
#39531=CARTESIAN_POINT('Ctrl Pts',(-57.4239210417209,-75.0178637334097,
179.142403412702));
#39532=CARTESIAN_POINT('Ctrl Pts',(-58.7341295958193,-74.9724679767354,
178.124930022896));
#39533=CARTESIAN_POINT('Ctrl Pts',(-58.948089224779,-75.0439396794041,176.480827714093));
#39534=CARTESIAN_POINT('Ctrl Pts',(-59.1620488537388,-75.1154113820728,
174.83672540529));
#39535=CARTESIAN_POINT('Ctrl Pts',(-58.1602464911887,-75.3164914354137,
173.529087012057));
#39536=CARTESIAN_POINT('Ctrl Pts',(-57.1584441286386,-75.5175714887547,
172.221448618824));
#39537=CARTESIAN_POINT('Ctrl Pts',(-55.5335435942162,-75.7850779700703,
172.016270977238));
#39538=CARTESIAN_POINT('Ctrl Pts',(-53.9086430597938,-76.0525844513858,
171.811093335651));
#39539=CARTESIAN_POINT('Ctrl Pts',(-52.6183106315294,-76.2844237373708,
172.828566725457));
#39540=CARTESIAN_POINT('Ctrl Pts',(-51.3279782032651,-76.5162630233557,
173.846040115263));
#39541=CARTESIAN_POINT('Ctrl Pts',(-51.1338947001393,-76.6312348499978,
175.490142424066));
#39542=CARTESIAN_POINT('Ctrl Pts',(-50.9398111970136,-76.7462066766398,
177.134244732869));
#39543=CARTESIAN_POINT('Ctrl Pts',(-51.9614896853977,-76.7315701526095,
178.441883126102));
#39544=CARTESIAN_POINT('Ctrl Pts',(-52.9831681737818,-76.7169336285793,
179.749521519335));
#39545=CARTESIAN_POINT('Ctrl Pts',(-54.6279448340383,-76.6358706765744,
179.954699160921));
#39546=CARTESIAN_POINT('Ctrl Pts',(-56.2727214942947,-76.5548077245695,
180.159876802508));
#39547=CARTESIAN_POINT('Ctrl Pts',(-57.5829300483931,-76.5094119678953,
179.142403412702));
#39548=CARTESIAN_POINT('Ctrl Pts',(-58.8931386024915,-76.464016211221,178.124930022896));
#39549=CARTESIAN_POINT('Ctrl Pts',(-59.1070982314513,-76.5354879138897,
176.480827714093));
#39550=CARTESIAN_POINT('Ctrl Pts',(-59.321057860411,-76.6069596165584,174.83672540529));
#39551=CARTESIAN_POINT('Ctrl Pts',(-58.319255497861,-76.8080396698993,173.529087012057));
#39552=CARTESIAN_POINT('Ctrl Pts',(-57.3174531353109,-77.0091197232403,
172.221448618824));
#39553=CARTESIAN_POINT('Ctrl Pts',(-55.6925526008884,-77.2766262045558,
172.016270977238));
#39554=CARTESIAN_POINT('Ctrl Pts',(-54.067652066466,-77.5441326858714,171.811093335651));
#39555=CARTESIAN_POINT('Ctrl Pts',(-52.7773196382016,-77.7759719718564,
172.828566725457));
#39556=CARTESIAN_POINT('Ctrl Pts',(-51.4869872099373,-78.0078112578414,
173.846040115263));
#39557=CARTESIAN_POINT('Ctrl Pts',(-51.2929037068116,-78.1227830844834,
175.490142424066));
#39558=CARTESIAN_POINT('Ctrl Pts',(-51.0988202036858,-78.2377549111254,
177.134244732869));
#39559=CARTESIAN_POINT('Ctrl Pts',(-52.1204986920699,-78.2231183870951,
178.441883126102));
#39560=CARTESIAN_POINT('Ctrl Pts',(-53.142177180454,-78.2084818630649,179.749521519335));
#39561=CARTESIAN_POINT('Ctrl Pts',(-54.7869538407105,-78.12741891106,179.954699160921));
#39562=CARTESIAN_POINT('Ctrl Pts',(-56.431730500967,-78.0463559590551,180.159876802508));
#39563=CARTESIAN_POINT('Ctrl Pts',(-57.7419390550653,-78.0009602023809,
179.142403412702));
#39564=CARTESIAN_POINT('Ctrl Pts',(-59.0521476091637,-77.9555644457066,
178.124930022896));
#39565=CARTESIAN_POINT('Ctrl Pts',(-59.2661072381235,-78.0270361483753,
176.480827714093));
#39566=CARTESIAN_POINT('Ctrl Pts',(-59.4800668670833,-78.098507851044,174.83672540529));
#39567=CARTESIAN_POINT('Ctrl Pts',(-58.4782645045332,-78.2995879043849,
173.529087012057));
#39568=CARTESIAN_POINT('Ctrl Pts',(-57.4764621419831,-78.5006679577259,
172.221448618824));
#39569=CARTESIAN_POINT('Ctrl Pts',(-55.8515616075607,-78.7681744390415,
172.016270977238));
#39570=CARTESIAN_POINT('Ctrl Pts',(-54.2266610731382,-79.035680920357,171.811093335651));
#39571=CARTESIAN_POINT('Ctrl Pts',(-52.9363286448739,-79.267520206342,172.828566725457));
#39572=CARTESIAN_POINT('Ctrl Pts',(-51.6459962166095,-79.4993594923269,
173.846040115263));
#39573=CARTESIAN_POINT('Ctrl Pts',(-51.4519127134838,-79.614331318969,175.490142424066));
#39574=CARTESIAN_POINT('Ctrl Pts',(-51.2578292103581,-79.729303145611,177.134244732869));
#39575=CARTESIAN_POINT('Ctrl Pts',(-52.2795076987422,-79.7146666215807,
178.441883126102));
#39576=CARTESIAN_POINT('Ctrl Pts',(-53.3011861871263,-79.7000300975505,
179.749521519335));
#39577=CARTESIAN_POINT('Ctrl Pts',(-54.9459628473827,-79.6189671455456,
179.954699160921));
#39578=CARTESIAN_POINT('Ctrl Pts',(-56.5907395076392,-79.5379041935407,
180.159876802508));
#39579=CARTESIAN_POINT('Ctrl Pts',(-57.9009480617376,-79.4925084368665,
179.142403412702));
#39580=CARTESIAN_POINT('Ctrl Pts',(-59.2111566158359,-79.4471126801922,
178.124930022896));
#39581=CARTESIAN_POINT('Ctrl Pts',(-59.4251162447957,-79.5185843828609,
176.480827714093));
#39582=CARTESIAN_POINT('Ctrl Pts',(-59.6390758737555,-79.5900560855296,
174.83672540529));
#39583=CARTESIAN_POINT('Ctrl Pts',(-58.6372735112054,-79.7911361388705,
173.529087012057));
#39584=CARTESIAN_POINT('Ctrl Pts',(-57.6354711486553,-79.9922161922115,
172.221448618824));
#39585=CARTESIAN_POINT('Ctrl Pts',(-56.0105706142329,-80.2597226735271,
172.016270977238));
#39586=CARTESIAN_POINT('Ctrl Pts',(-54.3856700798105,-80.5272291548426,
171.811093335651));
#39587=CARTESIAN_POINT('Ctrl Pts',(-53.0953376515461,-80.7590684408276,
172.828566725457));
#39588=CARTESIAN_POINT('Ctrl Pts',(-51.8050052232818,-80.9909077268126,
173.846040115263));
#39589=CARTESIAN_POINT('Ctrl Pts',(-51.610921720156,-81.1058795534546,175.490142424066));
#39590=CARTESIAN_POINT('Ctrl Pts',(-51.4168382170303,-81.2208513800966,
177.134244732869));
#39591=CARTESIAN_POINT('Ctrl Pts',(-52.4385167054144,-81.2062148560663,
178.441883126102));
#39592=CARTESIAN_POINT('Ctrl Pts',(-53.4601951937985,-81.1915783320361,
179.749521519335));
#39593=CARTESIAN_POINT('Ctrl Pts',(-55.104971854055,-81.1105153800312,179.954699160921));
#39594=CARTESIAN_POINT('Ctrl Pts',(-56.7497485143114,-81.0294524280263,
180.159876802508));
#39595=CARTESIAN_POINT('Ctrl Pts',(-58.0599570684098,-80.9840566713521,
179.142403412702));
#39596=CARTESIAN_POINT('Ctrl Pts',(-59.3701656225082,-80.9386609146778,
178.124930022896));
#39597=CARTESIAN_POINT('Ctrl Pts',(-59.5841252514679,-81.0101326173465,
176.480827714093));
#39598=CARTESIAN_POINT('Ctrl Pts',(-59.7980848804277,-81.0816043200152,
174.83672540529));
#39599=CARTESIAN_POINT('Ctrl Pts',(-58.7962825178776,-81.2826843733561,
173.529087012057));
#39600=CARTESIAN_POINT('Ctrl Pts',(-57.7944801553275,-81.4837644266971,
172.221448618824));
#39601=CARTESIAN_POINT('Ctrl Pts',(-56.1695796209051,-81.7512709080127,
172.016270977238));
#39602=CARTESIAN_POINT('Ctrl Pts',(-54.5446790864827,-82.0187773893282,
171.811093335651));
#39603=CARTESIAN_POINT('Ctrl Pts',(-53.2543466582183,-82.2506166753132,
172.828566725457));
#39604=CARTESIAN_POINT('Ctrl Pts',(-51.964014229954,-82.4824559612981,173.846040115263));
#39605=CARTESIAN_POINT('Ctrl Pts',(-51.7699307268282,-82.5974277879402,
175.490142424066));
#39606=CARTESIAN_POINT('Ctrl Pts',(-51.5758472237025,-82.7123996145822,
177.134244732869));
#39607=CARTESIAN_POINT('Ctrl Pts',(-52.5975257120866,-82.6977630905519,
178.441883126102));
#39608=CARTESIAN_POINT('Ctrl Pts',(-53.6192042004707,-82.6831265665217,
179.749521519335));
#39609=CARTESIAN_POINT('Ctrl Pts',(-55.2639808607272,-82.6020636145168,
179.954699160921));
#39610=CARTESIAN_POINT('Ctrl Pts',(-56.9087575209836,-82.521000662512,180.159876802508));
#39611=CARTESIAN_POINT('Ctrl Pts',(-58.218966075082,-82.4756049058377,179.142403412702));
#39612=CARTESIAN_POINT('Ctrl Pts',(-59.5291746291804,-82.4302091491634,
178.124930022896));
#39613=CARTESIAN_POINT('Ctrl Pts',(-59.7431342581402,-82.5016808518321,
176.480827714093));
#39614=CARTESIAN_POINT('Ctrl Pts',(-59.9570938870999,-82.5731525545008,
174.83672540529));
#39615=CARTESIAN_POINT('Ctrl Pts',(-58.9552915245499,-82.7742326078417,
173.529087012057));
#39616=CARTESIAN_POINT('Ctrl Pts',(-57.9534891619998,-82.9753126611827,
172.221448618824));
#39617=CARTESIAN_POINT('Ctrl Pts',(-56.3285886275773,-83.2428191424982,
172.016270977238));
#39618=CARTESIAN_POINT('Ctrl Pts',(-54.7036880931549,-83.5103256238138,
171.811093335651));
#39619=CARTESIAN_POINT('Ctrl Pts',(-53.4133556648906,-83.7421649097988,
172.828566725457));
#39620=CARTESIAN_POINT('Ctrl Pts',(-52.1230232366262,-83.9740041957837,
173.846040115263));
#39621=CARTESIAN_POINT('Ctrl Pts',(-51.9289397335005,-84.0889760224258,
175.490142424066));
#39622=CARTESIAN_POINT('Ctrl Pts',(-51.7348562303747,-84.2039478490678,
177.134244732869));
#39623=CARTESIAN_POINT('Ctrl Pts',(-52.7565347187588,-84.1893113250376,
178.441883126102));
#39624=CARTESIAN_POINT('Ctrl Pts',(-53.7782132071429,-84.1746748010073,
179.749521519335));
#39625=CARTESIAN_POINT('Ctrl Pts',(-55.4229898673994,-84.0936118490024,
179.954699160921));
#39626=CARTESIAN_POINT('Ctrl Pts',(-57.0677665276559,-84.0125488969975,
180.159876802508));
#39627=CARTESIAN_POINT('Ctrl Pts',(-58.3779750817542,-83.9671531403233,
179.142403412702));
#39628=CARTESIAN_POINT('Ctrl Pts',(-59.6881836358526,-83.921757383649,178.124930022896));
#39629=CARTESIAN_POINT('Ctrl Pts',(-59.9021432648124,-83.9932290863177,
176.480827714093));
#39630=CARTESIAN_POINT('Ctrl Pts',(-60.1161028937722,-84.0647007889864,
174.83672540529));
#39631=CARTESIAN_POINT('Ctrl Pts',(-59.1143005312221,-84.2657808423273,
173.529087012057));
#39632=CARTESIAN_POINT('Ctrl Pts',(-58.112498168672,-84.4668608956683,172.221448618824));
#39633=CARTESIAN_POINT('Ctrl Pts',(-56.4875976342496,-84.7343673769838,
172.016270977238));
#39634=CARTESIAN_POINT('Ctrl Pts',(-54.8626970998271,-85.0018738582994,
171.811093335651));
#39635=CARTESIAN_POINT('Ctrl Pts',(-53.5723646715628,-85.2337131442844,
172.828566725457));
#39636=CARTESIAN_POINT('Ctrl Pts',(-52.2820322432984,-85.4655524302694,
173.846040115263));
#39637=CARTESIAN_POINT('Ctrl Pts',(-52.0879487401727,-85.5805242569114,
175.490142424066));
#39638=CARTESIAN_POINT('Ctrl Pts',(-51.8938652370469,-85.6954960835534,
177.134244732869));
#39639=CARTESIAN_POINT('Ctrl Pts',(-52.915543725431,-85.6808595595231,178.441883126102));
#39640=CARTESIAN_POINT('Ctrl Pts',(-53.9372222138152,-85.6662230354929,
179.749521519335));
#39641=CARTESIAN_POINT('Ctrl Pts',(-55.5819988740716,-85.585160083488,179.954699160921));
#39642=CARTESIAN_POINT('Ctrl Pts',(-57.2267755343281,-85.5040971314831,
180.159876802508));
#39643=CARTESIAN_POINT('Ctrl Pts',(-58.5369840884265,-85.4587013748089,
179.142403412702));
#39644=CARTESIAN_POINT('Ctrl Pts',(-59.8471926425249,-85.4133056181346,
178.124930022896));
#39645=CARTESIAN_POINT('Ctrl Pts',(-60.0611522714846,-85.4847773208033,
176.480827714093));
#39646=CARTESIAN_POINT('Ctrl Pts',(-60.2751119004444,-85.556249023472,174.83672540529));
#39647=CARTESIAN_POINT('Ctrl Pts',(-59.2733095378943,-85.7573290768129,
173.529087012057));
#39648=CARTESIAN_POINT('Ctrl Pts',(-58.2715071753442,-85.9584091301539,
172.221448618824));
#39649=CARTESIAN_POINT('Ctrl Pts',(-56.6466066409218,-86.2259156114695,
172.016270977238));
#39650=CARTESIAN_POINT('Ctrl Pts',(-55.0217061064994,-86.493422092785,171.811093335651));
#39651=CARTESIAN_POINT('Ctrl Pts',(-53.731373678235,-86.72526137877,172.828566725457));
#39652=CARTESIAN_POINT('Ctrl Pts',(-52.4410412499707,-86.9571006647549,
173.846040115263));
#39653=CARTESIAN_POINT('Ctrl Pts',(-52.2469577468449,-87.072072491397,175.490142424066));
#39654=CARTESIAN_POINT('Ctrl Pts',(-52.0528742437192,-87.187044318039,177.134244732869));
#39655=CARTESIAN_POINT('Ctrl Pts',(-53.0745527321033,-87.1724077940087,
178.441883126102));
#39656=CARTESIAN_POINT('Ctrl Pts',(-54.0962312204874,-87.1577712699785,
179.749521519335));
#39657=CARTESIAN_POINT('Ctrl Pts',(-55.7410078807439,-87.0767083179736,
179.954699160921));
#39658=CARTESIAN_POINT('Ctrl Pts',(-57.3857845410003,-86.9956453659688,
180.159876802508));
#39659=CARTESIAN_POINT('Ctrl Pts',(-58.6959930950987,-86.9502496092945,
179.142403412702));
#39660=CARTESIAN_POINT('Ctrl Pts',(-60.0062016491971,-86.9048538526202,
178.124930022896));
#39661=CARTESIAN_POINT('Ctrl Pts',(-60.2201612781569,-86.9763255552889,
176.480827714093));
#39662=CARTESIAN_POINT('Ctrl Pts',(-60.4341209071166,-87.0477972579576,
174.83672540529));
#39663=CARTESIAN_POINT('Ctrl Pts',(-59.4323185445665,-87.2488773112985,
173.529087012057));
#39664=CARTESIAN_POINT('Ctrl Pts',(-58.4305161820165,-87.4499573646395,
172.221448618824));
#39665=CARTESIAN_POINT('Ctrl Pts',(-56.805615647594,-87.7174638459551,172.016270977238));
#39666=CARTESIAN_POINT('Ctrl Pts',(-55.1807151131716,-87.9849703272706,
171.811093335651));
#39667=CARTESIAN_POINT('Ctrl Pts',(-53.8903826849072,-88.2168096132556,
172.828566725457));
#39668=CARTESIAN_POINT('Ctrl Pts',(-52.6000502566429,-88.4486488992405,
173.846040115263));
#39669=CARTESIAN_POINT('Ctrl Pts',(-52.4059667535171,-88.5636207258826,
175.490142424066));
#39670=CARTESIAN_POINT('Ctrl Pts',(-52.2118832503914,-88.6785925525246,
177.134244732869));
#39671=CARTESIAN_POINT('Ctrl Pts',(-53.2335617387755,-88.6639560284944,
178.441883126102));
#39672=CARTESIAN_POINT('Ctrl Pts',(-54.2552402271596,-88.6493195044641,
179.749521519335));
#39673=CARTESIAN_POINT('Ctrl Pts',(-55.9000168874161,-88.5682565524592,
179.954699160921));
#39674=CARTESIAN_POINT('Ctrl Pts',(-57.5447935476725,-88.4871936004543,
180.159876802508));
#39675=CARTESIAN_POINT('Ctrl Pts',(-58.8550021017709,-88.4417978437801,
179.142403412702));
#39676=CARTESIAN_POINT('Ctrl Pts',(-60.1652106558693,-88.3964020871058,
178.124930022896));
#39677=CARTESIAN_POINT('Ctrl Pts',(-60.3791702848291,-88.4678737897745,
176.480827714093));
#39678=CARTESIAN_POINT('Ctrl Pts',(-60.5931299137889,-88.5393454924432,
174.83672540529));
#39679=CARTESIAN_POINT('Ctrl Pts',(-59.5913275512388,-88.7404255457841,
173.529087012057));
#39680=CARTESIAN_POINT('Ctrl Pts',(-58.5895251886887,-88.9415055991251,
172.221448618824));
#39681=CARTESIAN_POINT('Ctrl Pts',(-56.9646246542662,-89.2090120804406,
172.016270977238));
#39682=CARTESIAN_POINT('Ctrl Pts',(-55.3397241198438,-89.4765185617563,
171.811093335651));
#39683=CARTESIAN_POINT('Ctrl Pts',(-54.0493916915795,-89.7083578477412,
172.828566725457));
#39684=CARTESIAN_POINT('Ctrl Pts',(-52.7590592633151,-89.9401971337262,
173.846040115263));
#39685=CARTESIAN_POINT('Ctrl Pts',(-52.5649757601894,-90.0551689603682,
175.490142424066));
#39686=CARTESIAN_POINT('Ctrl Pts',(-52.3708922570636,-90.1701407870102,
177.134244732869));
#39687=CARTESIAN_POINT('Ctrl Pts',(-53.3925707454477,-90.1555042629799,
178.441883126102));
#39688=CARTESIAN_POINT('Ctrl Pts',(-54.4142492338319,-90.1408677389497,
179.749521519335));
#39689=CARTESIAN_POINT('Ctrl Pts',(-56.0590258940883,-90.0598047869448,
179.954699160921));
#39690=CARTESIAN_POINT('Ctrl Pts',(-57.7038025543448,-89.9787418349399,
180.159876802508));
#39691=CARTESIAN_POINT('Ctrl Pts',(-59.0140111084431,-89.9333460782657,
179.142403412702));
#39692=CARTESIAN_POINT('Ctrl Pts',(-60.3242196625415,-89.8879503215914,
178.124930022896));
#39693=CARTESIAN_POINT('Ctrl Pts',(-60.5381792915013,-89.9594220242601,
176.480827714093));
#39694=CARTESIAN_POINT('Ctrl Pts',(-60.7521389204611,-90.0308937269288,
174.83672540529));
#39695=CARTESIAN_POINT('Ctrl Pts',(-59.750336557911,-90.2319737802697,173.529087012057));
#39696=CARTESIAN_POINT('Ctrl Pts',(-58.7485341953609,-90.4330538336107,
172.221448618824));
#39697=CARTESIAN_POINT('Ctrl Pts',(-57.1236336609385,-90.7005603149262,
172.016270977238));
#39698=CARTESIAN_POINT('Ctrl Pts',(-55.498733126516,-90.9680667962418,171.811093335651));
#39699=CARTESIAN_POINT('Ctrl Pts',(-54.2084006982517,-91.1999060822268,
172.828566725457));
#39700=CARTESIAN_POINT('Ctrl Pts',(-52.9180682699873,-91.4317453682118,
173.846040115263));
#39701=CARTESIAN_POINT('Ctrl Pts',(-52.7239847668616,-91.5467171948538,
175.490142424066));
#39702=CARTESIAN_POINT('Ctrl Pts',(-52.5299012637359,-91.6616890214958,
177.134244732869));
#39703=CARTESIAN_POINT('Ctrl Pts',(-53.55157975212,-91.6470524974655,178.441883126102));
#39704=CARTESIAN_POINT('Ctrl Pts',(-54.5732582405041,-91.6324159734353,
179.749521519335));
#39705=CARTESIAN_POINT('Ctrl Pts',(-56.2180349007605,-91.5513530214304,
179.954699160921));
#39706=CARTESIAN_POINT('Ctrl Pts',(-57.862811561017,-91.4702900694256,180.159876802508));
#39707=CARTESIAN_POINT('Ctrl Pts',(-59.1730201151154,-91.4248943127513,
179.142403412702));
#39708=CARTESIAN_POINT('Ctrl Pts',(-60.4832286692138,-91.379498556077,178.124930022896));
#39709=CARTESIAN_POINT('Ctrl Pts',(-60.6971882981735,-91.4509702587457,
176.480827714093));
#39710=CARTESIAN_POINT('Ctrl Pts',(-60.9111479271333,-91.5224419614144,
174.83672540529));
#39711=CARTESIAN_POINT('Ctrl Pts',(-59.9093455645832,-91.7235220147553,
173.529087012057));
#39712=CARTESIAN_POINT('Ctrl Pts',(-58.9075432020331,-91.9246020680963,
172.221448618824));
#39713=CARTESIAN_POINT('Ctrl Pts',(-57.2826426676107,-92.1921085494119,
172.016270977238));
#39714=CARTESIAN_POINT('Ctrl Pts',(-55.6577421331883,-92.4596150307274,
171.811093335651));
#39715=CARTESIAN_POINT('Ctrl Pts',(-54.3674097049239,-92.6914543167124,
172.828566725457));
#39716=CARTESIAN_POINT('Ctrl Pts',(-53.0770772766596,-92.9232936026974,
173.846040115263));
#39717=CARTESIAN_POINT('Ctrl Pts',(-52.8829937735338,-93.0382654293394,
175.490142424066));
#39718=CARTESIAN_POINT('Ctrl Pts',(-52.6889102704081,-93.1532372559814,
177.134244732869));
#39719=CARTESIAN_POINT('Ctrl Pts',(-53.7105887587922,-93.1386007319512,
178.441883126102));
#39720=CARTESIAN_POINT('Ctrl Pts',(-54.7322672471763,-93.1239642079209,
179.749521519335));
#39721=CARTESIAN_POINT('Ctrl Pts',(-56.3770439074328,-93.042901255916,179.954699160921));
#39722=CARTESIAN_POINT('Ctrl Pts',(-58.0218205676892,-92.9618383039112,
180.159876802508));
#39723=CARTESIAN_POINT('Ctrl Pts',(-59.3320291217876,-92.9164425472369,
179.142403412702));
#39724=CARTESIAN_POINT('Ctrl Pts',(-60.642237675886,-92.8710467905626,178.124930022896));
#39725=CARTESIAN_POINT('Ctrl Pts',(-60.8561973048458,-92.9425184932313,
176.480827714093));
#39726=CARTESIAN_POINT('Ctrl Pts',(-61.0701569338055,-93.0139901959,174.83672540529));
#39727=CARTESIAN_POINT('Ctrl Pts',(-60.0683545712554,-93.2150702492409,
173.529087012057));
#39728=CARTESIAN_POINT('Ctrl Pts',(-59.0665522087054,-93.4161503025819,
172.221448618824));
#39729=CARTESIAN_POINT('Ctrl Pts',(-57.4416516742829,-93.6836567838974,
172.016270977238));
#39730=CARTESIAN_POINT('Ctrl Pts',(-55.8167511398605,-93.951163265213,171.811093335651));
#39731=CARTESIAN_POINT('Ctrl Pts',(-54.5264187115961,-94.183002551198,172.828566725457));
#39732=CARTESIAN_POINT('Ctrl Pts',(-53.2360862833318,-94.4148418371829,
173.846040115263));
#39733=CARTESIAN_POINT('Ctrl Pts',(-53.042002780206,-94.529813663825,175.490142424066));
#39734=CARTESIAN_POINT('Ctrl Pts',(-52.8479192770803,-94.644785490467,177.134244732869));
#39735=CARTESIAN_POINT('Ctrl Pts',(-53.8695977654644,-94.6301489664367,
178.441883126102));
#39736=CARTESIAN_POINT('Ctrl Pts',(-54.8912762538485,-94.6155124424065,
179.749521519335));
#39737=CARTESIAN_POINT('Ctrl Pts',(-56.536052914105,-94.5344494904016,179.954699160921));
#39738=CARTESIAN_POINT('Ctrl Pts',(-58.1808295743615,-94.4533865383968,
180.159876802508));
#39739=CARTESIAN_POINT('Ctrl Pts',(-59.4910381284598,-94.4079907817225,
179.142403412702));
#39740=CARTESIAN_POINT('Ctrl Pts',(-60.8012466825582,-94.3625950250483,
178.124930022896));
#39741=CARTESIAN_POINT('Ctrl Pts',(-61.015206311518,-94.4340667277169,176.480827714093));
#39742=CARTESIAN_POINT('Ctrl Pts',(-61.2291659404778,-94.5055384303856,
174.83672540529));
#39743=CARTESIAN_POINT('Ctrl Pts',(-60.2273635779277,-94.7066184837265,
173.529087012057));
#39744=CARTESIAN_POINT('Ctrl Pts',(-59.2255612153776,-94.9076985370675,
172.221448618824));
#39745=CARTESIAN_POINT('Ctrl Pts',(-57.6006606809552,-95.1752050183831,
172.016270977238));
#39746=CARTESIAN_POINT('Ctrl Pts',(-55.9757601465327,-95.4427114996986,
171.811093335651));
#39747=CARTESIAN_POINT('Ctrl Pts',(-54.6854277182684,-95.6745507856836,
172.828566725457));
#39748=CARTESIAN_POINT('Ctrl Pts',(-53.395095290004,-95.9063900716686,173.846040115263));
#39749=CARTESIAN_POINT('Ctrl Pts',(-53.2010117868783,-96.0213618983106,
175.490142424066));
#39750=CARTESIAN_POINT('Ctrl Pts',(-53.0069282837525,-96.1363337249526,
177.134244732869));
#39751=CARTESIAN_POINT('Ctrl Pts',(-54.0286067721367,-96.1216972009223,
178.441883126102));
#39752=CARTESIAN_POINT('Ctrl Pts',(-55.0502852605208,-96.1070606768921,
179.749521519335));
#39753=CARTESIAN_POINT('Ctrl Pts',(-56.6950619207772,-96.0259977248872,
179.954699160921));
#39754=CARTESIAN_POINT('Ctrl Pts',(-58.3398385810337,-95.9449347728824,
180.159876802508));
#39755=CARTESIAN_POINT('Ctrl Pts',(-59.6500471351321,-95.8995390162081,
179.142403412702));
#39756=CARTESIAN_POINT('Ctrl Pts',(-60.9602556892304,-95.8541432595338,
178.124930022896));
#39757=CARTESIAN_POINT('Ctrl Pts',(-61.1742153181902,-95.9256149622025,
176.480827714093));
#39758=CARTESIAN_POINT('Ctrl Pts',(-61.38817494715,-95.9970866648712,174.83672540529));
#39759=CARTESIAN_POINT('Ctrl Pts',(-60.3863725845999,-96.1981667182121,
173.529087012057));
#39760=CARTESIAN_POINT('Ctrl Pts',(-59.3845702220498,-96.3992467715531,
172.221448618824));
#39761=CARTESIAN_POINT('Ctrl Pts',(-57.7596696876274,-96.6667532528687,
172.016270977238));
#39762=CARTESIAN_POINT('Ctrl Pts',(-56.134769153205,-96.9342597341842,171.811093335651));
#39763=CARTESIAN_POINT('Ctrl Pts',(-54.8444367249406,-97.1660990201692,
172.828566725457));
#39764=CARTESIAN_POINT('Ctrl Pts',(-53.5541042966763,-97.3979383061541,
173.846040115263));
#39765=CARTESIAN_POINT('Ctrl Pts',(-53.3600207935505,-97.5129101327962,
175.490142424066));
#39766=CARTESIAN_POINT('Ctrl Pts',(-53.1659372904248,-97.6278819594382,
177.134244732869));
#39767=CARTESIAN_POINT('Ctrl Pts',(-54.1876157788089,-97.6132454354079,
178.441883126102));
#39768=CARTESIAN_POINT('Ctrl Pts',(-55.209294267193,-97.5986089113777,179.749521519335));
#39769=CARTESIAN_POINT('Ctrl Pts',(-56.8540709274494,-97.5175459593728,
179.954699160921));
#39770=CARTESIAN_POINT('Ctrl Pts',(-58.4988475877059,-97.436483007368,180.159876802508));
#39771=CARTESIAN_POINT('Ctrl Pts',(-59.8090561418043,-97.3910872506937,
179.142403412702));
#39772=CARTESIAN_POINT('Ctrl Pts',(-61.1192646959027,-97.3456914940194,
178.124930022896));
#39773=CARTESIAN_POINT('Ctrl Pts',(-61.3332243248624,-97.4171631966881,
176.480827714093));
#39774=CARTESIAN_POINT('Ctrl Pts',(-61.5471839538222,-97.4886348993568,
174.83672540529));
#39775=CARTESIAN_POINT('Ctrl Pts',(-60.5453815912721,-97.6897149526977,
173.529087012057));
#39776=CARTESIAN_POINT('Ctrl Pts',(-59.5435792287221,-97.8907950060387,
172.221448618824));
#39777=CARTESIAN_POINT('Ctrl Pts',(-57.9186786942996,-98.1583014873543,
172.016270977238));
#39778=CARTESIAN_POINT('Ctrl Pts',(-56.2937781598772,-98.4258079686698,
171.811093335651));
#39779=CARTESIAN_POINT('Ctrl Pts',(-55.0034457316128,-98.6576472546548,
172.828566725457));
#39780=CARTESIAN_POINT('Ctrl Pts',(-53.7131133033485,-98.8894865406397,
173.846040115263));
#39781=CARTESIAN_POINT('Ctrl Pts',(-53.5190298002227,-99.0044583672818,
175.490142424066));
#39782=CARTESIAN_POINT('Ctrl Pts',(-53.324946297097,-99.1194301939238,177.134244732869));
#39783=CARTESIAN_POINT('Ctrl Pts',(-54.3466247854811,-99.1047936698936,
178.441883126102));
#39784=CARTESIAN_POINT('Ctrl Pts',(-55.3683032738652,-99.0901571458633,
179.749521519335));
#39785=CARTESIAN_POINT('Ctrl Pts',(-57.0130799341217,-99.0090941938584,
179.954699160921));
#39786=CARTESIAN_POINT('Ctrl Pts',(-58.6578565943781,-98.9280312418536,
180.159876802508));
#39787=CARTESIAN_POINT('Ctrl Pts',(-59.9680651484765,-98.8826354851793,
179.142403412702));
#39788=CARTESIAN_POINT('Ctrl Pts',(-61.2782737025749,-98.837239728505,178.124930022896));
#39789=CARTESIAN_POINT('Ctrl Pts',(-61.4922333315347,-98.9087114311737,
176.480827714093));
#39790=CARTESIAN_POINT('Ctrl Pts',(-61.7061929604944,-98.9801831338424,
174.83672540529));
#39791=CARTESIAN_POINT('Ctrl Pts',(-60.7043905979444,-99.1812631871833,
173.529087012057));
#39792=CARTESIAN_POINT('Ctrl Pts',(-59.7025882353943,-99.3823432405243,
172.221448618824));
#39793=CARTESIAN_POINT('Ctrl Pts',(-58.0776877009718,-99.6498497218399,
172.016270977238));
#39794=CARTESIAN_POINT('Ctrl Pts',(-56.4527871665494,-99.9173562031554,
171.811093335651));
#39795=CARTESIAN_POINT('Ctrl Pts',(-55.162454738285,-100.14919548914,172.828566725457));
#39796=CARTESIAN_POINT('Ctrl Pts',(-53.8721223100207,-100.381034775125,
173.846040115263));
#39797=CARTESIAN_POINT('Ctrl Pts',(-53.678038806895,-100.496006601767,175.490142424066));
#39798=CARTESIAN_POINT('Ctrl Pts',(-53.4839553037692,-100.610978428409,
177.134244732869));
#39799=CARTESIAN_POINT('Ctrl Pts',(-54.5056337921533,-100.596341904379,
178.441883126102));
#39800=CARTESIAN_POINT('Ctrl Pts',(-55.5273122805374,-100.581705380349,
179.749521519335));
#39801=CARTESIAN_POINT('Ctrl Pts',(-57.1720889407939,-100.500642428344,
179.954699160921));
#39802=CARTESIAN_POINT('Ctrl Pts',(-58.8168656010504,-100.419579476339,
180.159876802508));
#39803=CARTESIAN_POINT('Ctrl Pts',(-60.1270741551487,-100.374183719665,
179.142403412702));
#39804=CARTESIAN_POINT('Ctrl Pts',(-61.4372827092471,-100.328787962991,
178.124930022896));
#39805=CARTESIAN_POINT('Ctrl Pts',(-61.6512423382069,-100.400259665659,
176.480827714093));
#39806=CARTESIAN_POINT('Ctrl Pts',(-61.8652019671667,-100.471731368328,
174.83672540529));
#39807=CARTESIAN_POINT('Ctrl Pts',(-60.8633996046166,-100.672811421669,
173.529087012057));
#39808=CARTESIAN_POINT('Ctrl Pts',(-59.8615972420665,-100.87389147501,172.221448618824));
#39809=CARTESIAN_POINT('Ctrl Pts',(-58.2366967076441,-101.141397956325,
172.016270977238));
#39810=CARTESIAN_POINT('Ctrl Pts',(-56.6117961732216,-101.408904437641,
171.811093335651));
#39811=CARTESIAN_POINT('Ctrl Pts',(-55.3214637449573,-101.640743723626,
172.828566725457));
#39812=CARTESIAN_POINT('Ctrl Pts',(-54.0311313166929,-101.872583009611,
173.846040115263));
#39813=CARTESIAN_POINT('Ctrl Pts',(-53.8370478135672,-101.987554836253,
175.490142424066));
#39814=CARTESIAN_POINT('Ctrl Pts',(-53.6429643104415,-102.102526662895,
177.134244732869));
#39815=CARTESIAN_POINT('Ctrl Pts',(-54.6646427988256,-102.087890138865,
178.441883126102));
#39816=CARTESIAN_POINT('Ctrl Pts',(-55.6863212872097,-102.073253614834,
179.749521519335));
#39817=CARTESIAN_POINT('Ctrl Pts',(-57.3310979474661,-101.99219066283,179.954699160921));
#39818=CARTESIAN_POINT('Ctrl Pts',(-58.9758746077226,-101.911127710825,
180.159876802508));
#39819=CARTESIAN_POINT('Ctrl Pts',(-60.286083161821,-101.865731954151,179.142403412702));
#39820=CARTESIAN_POINT('Ctrl Pts',(-61.5962917159193,-101.820336197476,
178.124930022896));
#39821=CARTESIAN_POINT('Ctrl Pts',(-61.8102513448791,-101.891807900145,
176.480827714093));
#39822=CARTESIAN_POINT('Ctrl Pts',(-62.0242109738389,-101.963279602814,
174.83672540529));
#39823=CARTESIAN_POINT('Ctrl Pts',(-61.0224086112888,-102.164359656155,
173.529087012057));
#39824=CARTESIAN_POINT('Ctrl Pts',(-60.0206062487387,-102.365439709496,
172.221448618824));
#39825=CARTESIAN_POINT('Ctrl Pts',(-58.3957057143163,-102.632946190811,
172.016270977238));
#39826=CARTESIAN_POINT('Ctrl Pts',(-56.7708051798939,-102.900452672127,
171.811093335651));
#39827=CARTESIAN_POINT('Ctrl Pts',(-55.4804727516295,-103.132291958112,
172.828566725457));
#39828=CARTESIAN_POINT('Ctrl Pts',(-54.1901403233652,-103.364131244097,
173.846040115263));
#39829=CARTESIAN_POINT('Ctrl Pts',(-53.9960568202394,-103.479103070739,
175.490142424066));
#39830=CARTESIAN_POINT('Ctrl Pts',(-53.8019733171137,-103.594074897381,
177.134244732869));
#39831=CARTESIAN_POINT('Ctrl Pts',(-54.8236518054978,-103.57943837335,178.441883126102));
#39832=CARTESIAN_POINT('Ctrl Pts',(-55.8453302938819,-103.56480184932,179.749521519335));
#39833=CARTESIAN_POINT('Ctrl Pts',(-57.4901069541384,-103.483738897315,
179.954699160921));
#39834=CARTESIAN_POINT('Ctrl Pts',(-59.1348836143948,-103.40267594531,180.159876802508));
#39835=CARTESIAN_POINT('Ctrl Pts',(-60.4450921684932,-103.357280188636,
179.142403412702));
#39836=CARTESIAN_POINT('Ctrl Pts',(-61.7553007225916,-103.311884431962,
178.124930022896));
#39837=CARTESIAN_POINT('Ctrl Pts',(-61.9692603515513,-103.383356134631,
176.480827714093));
#39838=CARTESIAN_POINT('Ctrl Pts',(-62.1832199805111,-103.454827837299,
174.83672540529));
#39839=CARTESIAN_POINT('Ctrl Pts',(-61.181417617961,-103.65590789064,173.529087012057));
#39840=CARTESIAN_POINT('Ctrl Pts',(-60.179615255411,-103.856987943981,172.221448618824));
#39841=CARTESIAN_POINT('Ctrl Pts',(-58.5547147209885,-104.124494425297,
172.016270977238));
#39842=CARTESIAN_POINT('Ctrl Pts',(-56.9298141865661,-104.392000906612,
171.811093335651));
#39843=CARTESIAN_POINT('Ctrl Pts',(-55.6394817583017,-104.623840192597,
172.828566725457));
#39844=CARTESIAN_POINT('Ctrl Pts',(-54.3491493300374,-104.855679478582,
173.846040115263));
#39845=CARTESIAN_POINT('Ctrl Pts',(-54.1550658269116,-104.970651305224,
175.490142424066));
#39846=CARTESIAN_POINT('Ctrl Pts',(-53.9609823237859,-105.085623131866,
177.134244732869));
#39847=CARTESIAN_POINT('Ctrl Pts',(-54.98266081217,-105.070986607836,178.441883126102));
#39848=CARTESIAN_POINT('Ctrl Pts',(-56.0043393005541,-105.056350083806,
179.749521519335));
#39849=CARTESIAN_POINT('Ctrl Pts',(-57.6491159608106,-104.975287131801,
179.954699160921));
#39850=CARTESIAN_POINT('Ctrl Pts',(-59.293892621067,-104.894224179796,180.159876802508));
#39851=CARTESIAN_POINT('Ctrl Pts',(-60.6041011751654,-104.848828423122,
179.142403412702));
#39852=CARTESIAN_POINT('Ctrl Pts',(-61.9143097292638,-104.803432666447,
178.124930022896));
#39853=CARTESIAN_POINT('Ctrl Pts',(-62.1282693582236,-104.874904369116,
176.480827714093));
#39854=CARTESIAN_POINT('Ctrl Pts',(-62.3422289871834,-104.946376071785,
174.83672540529));
#39855=CARTESIAN_POINT('Ctrl Pts',(-61.3404266246333,-105.147456125126,
173.529087012057));
#39856=CARTESIAN_POINT('Ctrl Pts',(-60.3386242620832,-105.348536178467,
172.221448618824));
#39857=CARTESIAN_POINT('Ctrl Pts',(-58.7137237276607,-105.616042659782,
172.016270977238));
#39858=CARTESIAN_POINT('Ctrl Pts',(-57.0888231932383,-105.883549141098,
171.811093335651));
#39859=CARTESIAN_POINT('Ctrl Pts',(-55.798490764974,-106.115388427083,172.828566725457));
#39860=CARTESIAN_POINT('Ctrl Pts',(-54.5081583367096,-106.347227713068,
173.846040115263));
#39861=CARTESIAN_POINT('Ctrl Pts',(-54.3140748335839,-106.46219953971,175.490142424066));
#39862=CARTESIAN_POINT('Ctrl Pts',(-54.1199913304581,-106.577171366352,
177.134244732869));
#39863=CARTESIAN_POINT('Ctrl Pts',(-55.1416698188422,-106.562534842322,
178.441883126102));
#39864=CARTESIAN_POINT('Ctrl Pts',(-56.1633483072264,-106.547898318291,
179.749521519335));
#39865=CARTESIAN_POINT('Ctrl Pts',(-57.8081249674828,-106.466835366286,
179.954699160921));
#39866=CARTESIAN_POINT('Ctrl Pts',(-59.4529016277393,-106.385772414282,
180.159876802508));
#39867=CARTESIAN_POINT('Ctrl Pts',(-60.7631101818376,-106.340376657607,
179.142403412702));
#39868=CARTESIAN_POINT('Ctrl Pts',(-62.073318735936,-106.294980900933,178.124930022896));
#39869=CARTESIAN_POINT('Ctrl Pts',(-62.2872783648958,-106.366452603602,
176.480827714093));
#39870=CARTESIAN_POINT('Ctrl Pts',(-62.5012379938556,-106.43792430627,174.83672540529));
#39871=CARTESIAN_POINT('Ctrl Pts',(-61.4994356313055,-106.639004359611,
173.529087012057));
#39872=CARTESIAN_POINT('Ctrl Pts',(-60.4976332687554,-106.840084412952,
172.221448618824));
#39873=CARTESIAN_POINT('Ctrl Pts',(-58.872732734333,-107.107590894268,172.016270977238));
#39874=CARTESIAN_POINT('Ctrl Pts',(-57.2478321999105,-107.375097375583,
171.811093335651));
#39875=CARTESIAN_POINT('Ctrl Pts',(-55.9574997716462,-107.606936661568,
172.828566725457));
#39876=CARTESIAN_POINT('Ctrl Pts',(-54.6671673433818,-107.838775947553,
173.846040115263));
#39877=CARTESIAN_POINT('Ctrl Pts',(-54.4730838402561,-107.953747774195,
175.490142424066));
#39878=CARTESIAN_POINT('Ctrl Pts',(-54.2790003371304,-108.068719600837,
177.134244732869));
#39879=CARTESIAN_POINT('Ctrl Pts',(-55.3006788255145,-108.054083076807,
178.441883126102));
#39880=CARTESIAN_POINT('Ctrl Pts',(-56.3223573138986,-108.039446552777,
179.749521519335));
#39881=CARTESIAN_POINT('Ctrl Pts',(-57.967133974155,-107.958383600772,179.954699160921));
#39882=CARTESIAN_POINT('Ctrl Pts',(-59.6119106344115,-107.877320648767,
180.159876802508));
#39883=CARTESIAN_POINT('Ctrl Pts',(-60.9221191885099,-107.831924892093,
179.142403412702));
#39884=CARTESIAN_POINT('Ctrl Pts',(-62.2323277426083,-107.786529135419,
178.124930022896));
#39885=CARTESIAN_POINT('Ctrl Pts',(-62.446287371568,-107.858000838087,176.480827714093));
#39886=CARTESIAN_POINT('Ctrl Pts',(-62.6602470005278,-107.929472540756,
174.83672540529));
#39887=CARTESIAN_POINT('Ctrl Pts',(-61.6584446379777,-108.130552594097,
173.529087012057));
#39888=CARTESIAN_POINT('Ctrl Pts',(-60.6566422754277,-108.331632647438,
172.221448618824));
#39889=CARTESIAN_POINT('Ctrl Pts',(-59.0317417410052,-108.599139128753,
172.016270977238));
#39890=CARTESIAN_POINT('Ctrl Pts',(-57.4068412065828,-108.866645610069,
171.811093335651));
#39891=CARTESIAN_POINT('Ctrl Pts',(-56.1165087783184,-109.098484896054,
172.828566725457));
#39892=CARTESIAN_POINT('Ctrl Pts',(-54.8261763500541,-109.330324182039,
173.846040115263));
#39893=CARTESIAN_POINT('Ctrl Pts',(-54.6320928469283,-109.445296008681,
175.490142424066));
#39894=CARTESIAN_POINT('Ctrl Pts',(-54.4380093438026,-109.560267835323,
177.134244732869));
#39895=CARTESIAN_POINT('Ctrl Pts',(-55.4596878321867,-109.545631311293,
178.441883126102));
#39896=CARTESIAN_POINT('Ctrl Pts',(-56.4813663205708,-109.530994787262,
179.749521519335));
#39897=CARTESIAN_POINT('Ctrl Pts',(-58.1261429808273,-109.449931835258,
179.954699160921));
#39898=CARTESIAN_POINT('Ctrl Pts',(-59.7709196410837,-109.368868883253,
180.159876802508));
#39899=CARTESIAN_POINT('Ctrl Pts',(-61.0811281951821,-109.323473126579,
179.142403412702));
#39900=CARTESIAN_POINT('Ctrl Pts',(-62.3913367492805,-109.278077369904,
178.124930022896));
#39901=CARTESIAN_POINT('Ctrl Pts',(-62.6052963782402,-109.349549072573,
176.480827714093));
#39902=CARTESIAN_POINT('Ctrl Pts',(-62.8192560072,-109.421020775242,174.83672540529));
#39903=CARTESIAN_POINT('Ctrl Pts',(-61.8174536446499,-109.622100828583,
173.529087012057));
#39904=CARTESIAN_POINT('Ctrl Pts',(-60.8156512820999,-109.823180881923,
172.221448618824));
#39905=CARTESIAN_POINT('Ctrl Pts',(-59.1907507476774,-110.090687363239,
172.016270977238));
#39906=CARTESIAN_POINT('Ctrl Pts',(-57.565850213255,-110.358193844555,171.811093335651));
#39907=CARTESIAN_POINT('Ctrl Pts',(-56.2755177849906,-110.59003313054,172.828566725457));
#39908=CARTESIAN_POINT('Ctrl Pts',(-54.9851853567263,-110.821872416525,
173.846040115263));
#39909=CARTESIAN_POINT('Ctrl Pts',(-54.7911018536006,-110.936844243167,
175.490142424066));
#39910=CARTESIAN_POINT('Ctrl Pts',(-54.5970183504748,-111.051816069809,
177.134244732869));
#39911=CARTESIAN_POINT('Ctrl Pts',(-55.6186968388589,-111.037179545778,
178.441883126102));
#39912=CARTESIAN_POINT('Ctrl Pts',(-56.640375327243,-111.022543021748,179.749521519335));
#39913=CARTESIAN_POINT('Ctrl Pts',(-58.2851519874995,-110.941480069743,
179.954699160921));
#39914=CARTESIAN_POINT('Ctrl Pts',(-59.929928647756,-110.860417117738,180.159876802508));
#39915=CARTESIAN_POINT('Ctrl Pts',(-61.2401372018543,-110.815021361064,
179.142403412702));
#39916=CARTESIAN_POINT('Ctrl Pts',(-62.5503457559527,-110.76962560439,178.124930022896));
#39917=CARTESIAN_POINT('Ctrl Pts',(-62.7643053849125,-110.841097307058,
176.480827714093));
#39918=CARTESIAN_POINT('Ctrl Pts',(-62.9782650138722,-110.912569009727,
174.83672540529));
#39919=CARTESIAN_POINT('Ctrl Pts',(-61.9764626513222,-111.113649063068,
173.529087012057));
#39920=CARTESIAN_POINT('Ctrl Pts',(-60.9746602887721,-111.314729116409,
172.221448618824));
#39921=CARTESIAN_POINT('Ctrl Pts',(-59.3497597543497,-111.582235597725,
172.016270977238));
#39922=CARTESIAN_POINT('Ctrl Pts',(-57.7248592199272,-111.84974207904,171.811093335651));
#39923=CARTESIAN_POINT('Ctrl Pts',(-56.4345267916629,-112.081581365025,
172.828566725457));
#39924=CARTESIAN_POINT('Ctrl Pts',(-55.1441943633985,-112.31342065101,173.846040115263));
#39925=CARTESIAN_POINT('Ctrl Pts',(-54.9501108602728,-112.428392477652,
175.490142424066));
#39926=CARTESIAN_POINT('Ctrl Pts',(-54.756027357147,-112.543364304294,177.134244732869));
#39927=CARTESIAN_POINT('Ctrl Pts',(-55.7777058455311,-112.528727780264,
178.441883126102));
#39928=CARTESIAN_POINT('Ctrl Pts',(-56.7993843339153,-112.514091256234,
179.749521519335));
#39929=CARTESIAN_POINT('Ctrl Pts',(-58.4441609941717,-112.433028304229,
179.954699160921));
#39930=CARTESIAN_POINT('Ctrl Pts',(-60.0889376544282,-112.351965352224,
180.159876802508));
#39931=CARTESIAN_POINT('Ctrl Pts',(-61.3991462085265,-112.30656959555,179.142403412702));
#39932=CARTESIAN_POINT('Ctrl Pts',(-62.7093547626249,-112.261173838875,
178.124930022896));
#39933=CARTESIAN_POINT('Ctrl Pts',(-62.9233143915847,-112.332645541544,
176.480827714093));
#39934=CARTESIAN_POINT('Ctrl Pts',(-63.1372740205445,-112.404117244213,
174.83672540529));
#39935=CARTESIAN_POINT('Ctrl Pts',(-62.1354716579944,-112.605197297554,
173.529087012057));
#39936=CARTESIAN_POINT('Ctrl Pts',(-61.1336692954443,-112.806277350895,
172.221448618824));
#39937=CARTESIAN_POINT('Ctrl Pts',(-59.5087687610219,-113.07378383221,172.016270977238));
#39938=CARTESIAN_POINT('Ctrl Pts',(-57.8838682265995,-113.341290313526,
171.811093335651));
#39939=CARTESIAN_POINT('Ctrl Pts',(-56.5935357983351,-113.573129599511,
172.828566725457));
#39940=CARTESIAN_POINT('Ctrl Pts',(-55.3032033700708,-113.804968885496,
173.846040115263));
#39941=CARTESIAN_POINT('Ctrl Pts',(-55.109119866945,-113.919940712138,175.490142424066));
#39942=CARTESIAN_POINT('Ctrl Pts',(-54.9150363638193,-114.03491253878,177.134244732869));
#39943=CARTESIAN_POINT('Ctrl Pts',(-55.9367148522034,-114.02027601475,178.441883126102));
#39944=CARTESIAN_POINT('Ctrl Pts',(-56.9583933405875,-114.005639490719,
179.749521519335));
#39945=CARTESIAN_POINT('Ctrl Pts',(-58.6031700008439,-113.924576538714,
179.954699160921));
#39946=CARTESIAN_POINT('Ctrl Pts',(-60.2479466611004,-113.84351358671,180.159876802508));
#39947=CARTESIAN_POINT('Ctrl Pts',(-61.5581552151988,-113.798117830035,
179.142403412702));
#39948=CARTESIAN_POINT('Ctrl Pts',(-62.8683637692972,-113.752722073361,
178.124930022896));
#39949=CARTESIAN_POINT('Ctrl Pts',(-63.0823233982569,-113.82419377603,176.480827714093));
#39950=CARTESIAN_POINT('Ctrl Pts',(-63.2962830272167,-113.895665478698,
174.83672540529));
#39951=CARTESIAN_POINT('Ctrl Pts',(-62.2944806646666,-114.096745532039,
173.529087012057));
#39952=CARTESIAN_POINT('Ctrl Pts',(-61.2926783021166,-114.29782558538,172.221448618824));
#39953=CARTESIAN_POINT('Ctrl Pts',(-59.6677777676941,-114.565332066696,
172.016270977238));
#39954=CARTESIAN_POINT('Ctrl Pts',(-58.0428772332717,-114.832838548011,
171.811093335651));
#39955=CARTESIAN_POINT('Ctrl Pts',(-56.7525448050073,-115.064677833996,
172.828566725457));
#39956=CARTESIAN_POINT('Ctrl Pts',(-55.462212376743,-115.296517119981,173.846040115263));
#39957=CARTESIAN_POINT('Ctrl Pts',(-55.2681288736172,-115.411488946623,
175.490142424066));
#39958=CARTESIAN_POINT('Ctrl Pts',(-55.0740453704915,-115.526460773265,
177.134244732869));
#39959=CARTESIAN_POINT('Ctrl Pts',(-56.0957238588756,-115.511824249235,
178.441883126102));
#39960=CARTESIAN_POINT('Ctrl Pts',(-57.1174023472597,-115.497187725205,
179.749521519335));
#39961=CARTESIAN_POINT('Ctrl Pts',(-58.7621790075162,-115.4161247732,179.954699160921));
#39962=CARTESIAN_POINT('Ctrl Pts',(-60.4069556677726,-115.335061821195,
180.159876802508));
#39963=CARTESIAN_POINT('Ctrl Pts',(-61.717164221871,-115.289666064521,179.142403412702));
#39964=CARTESIAN_POINT('Ctrl Pts',(-63.0273727759694,-115.244270307847,
178.124930022896));
#39965=CARTESIAN_POINT('Ctrl Pts',(-63.2413324049292,-115.315742010515,
176.480827714093));
#39966=CARTESIAN_POINT('Ctrl Pts',(-63.4552920338889,-115.387213713184,
174.83672540529));
#39967=CARTESIAN_POINT('Ctrl Pts',(-62.4534896713389,-115.588293766525,
173.529087012057));
#39968=CARTESIAN_POINT('Ctrl Pts',(-61.4516873087888,-115.789373819866,
172.221448618824));
#39969=CARTESIAN_POINT('Ctrl Pts',(-59.8267867743663,-116.056880301181,
172.016270977238));
#39970=CARTESIAN_POINT('Ctrl Pts',(-58.2018862399439,-116.324386782497,
171.811093335651));
#39971=CARTESIAN_POINT('Ctrl Pts',(-56.9115538116796,-116.556226068482,
172.828566725457));
#39972=CARTESIAN_POINT('Ctrl Pts',(-55.6212213834152,-116.788065354467,
173.846040115263));
#39973=CARTESIAN_POINT('Ctrl Pts',(-55.4271378802895,-116.903037181109,
175.490142424066));
#39974=CARTESIAN_POINT('Ctrl Pts',(-55.2330543771637,-117.018009007751,
177.134244732869));
#39975=CARTESIAN_POINT('Ctrl Pts',(-56.2547328655478,-117.003372483721,
178.441883126102));
#39976=CARTESIAN_POINT('Ctrl Pts',(-57.2764113539319,-116.98873595969,179.749521519335));
#39977=CARTESIAN_POINT('Ctrl Pts',(-58.9211880141884,-116.907673007686,
179.954699160921));
#39978=CARTESIAN_POINT('Ctrl Pts',(-60.5659646744449,-116.826610055681,
180.159876802508));
#39979=CARTESIAN_POINT('Ctrl Pts',(-61.8761732285432,-116.781214299006,
179.142403412702));
#39980=CARTESIAN_POINT('Ctrl Pts',(-63.1863817826416,-116.735818542332,
178.124930022896));
#39981=CARTESIAN_POINT('Ctrl Pts',(-63.4003414116014,-116.807290245001,
176.480827714093));
#39982=CARTESIAN_POINT('Ctrl Pts',(-63.6143010405612,-116.87876194767,174.83672540529));
#39983=CARTESIAN_POINT('Ctrl Pts',(-62.6124986780111,-117.079842001011,
173.529087012057));
#39984=CARTESIAN_POINT('Ctrl Pts',(-61.610696315461,-117.280922054351,172.221448618824));
#39985=CARTESIAN_POINT('Ctrl Pts',(-59.9857957810386,-117.548428535667,
172.016270977238));
#39986=CARTESIAN_POINT('Ctrl Pts',(-58.3608952466161,-117.815935016983,
171.811093335651));
#39987=CARTESIAN_POINT('Ctrl Pts',(-57.0705628183518,-118.047774302968,
172.828566725457));
#39988=CARTESIAN_POINT('Ctrl Pts',(-55.7802303900874,-118.279613588953,
173.846040115263));
#39989=CARTESIAN_POINT('Ctrl Pts',(-55.5861468869617,-118.394585415595,
175.490142424066));
#39990=CARTESIAN_POINT('Ctrl Pts',(-55.3920633838359,-118.509557242237,
177.134244732869));
#39991=CARTESIAN_POINT('Ctrl Pts',(-56.4137418722201,-118.494920718206,
178.441883126102));
#39992=CARTESIAN_POINT('Ctrl Pts',(-57.4354203606042,-118.480284194176,
179.749521519335));
#39993=CARTESIAN_POINT('Ctrl Pts',(-59.0801970208606,-118.399221242171,
179.954699160921));
#39994=CARTESIAN_POINT('Ctrl Pts',(-60.7249736811171,-118.318158290166,
180.159876802508));
#39995=CARTESIAN_POINT('Ctrl Pts',(-62.0351822352155,-118.272762533492,
179.142403412702));
#39996=CARTESIAN_POINT('Ctrl Pts',(-63.3453907893139,-118.227366776818,
178.124930022896));
#39997=CARTESIAN_POINT('Ctrl Pts',(-63.5593504182736,-118.298838479487,
176.480827714093));
#39998=CARTESIAN_POINT('Ctrl Pts',(-63.7733100472334,-118.370310182155,
174.83672540529));
#39999=CARTESIAN_POINT('Ctrl Pts',(-62.7715076846833,-118.571390235496,
173.529087012057));
#40000=CARTESIAN_POINT('Ctrl Pts',(-61.7697053221332,-118.772470288837,
172.221448618824));
#40001=CARTESIAN_POINT('Ctrl Pts',(-60.1448047877108,-119.039976770153,
172.016270977238));
#40002=CARTESIAN_POINT('Ctrl Pts',(-58.5199042532884,-119.307483251468,
171.811093335651));
#40003=CARTESIAN_POINT('Ctrl Pts',(-57.229571825024,-119.539322537453,172.828566725457));
#40004=CARTESIAN_POINT('Ctrl Pts',(-55.9392393967597,-119.771161823438,
173.846040115263));
#40005=CARTESIAN_POINT('Ctrl Pts',(-55.7451558936339,-119.88613365008,175.490142424066));
#40006=CARTESIAN_POINT('Ctrl Pts',(-55.5510723905082,-120.001105476722,
177.134244732869));
#40007=CARTESIAN_POINT('Ctrl Pts',(-56.5727508788923,-119.986468952692,
178.441883126102));
#40008=CARTESIAN_POINT('Ctrl Pts',(-57.5944293672764,-119.971832428662,
179.749521519335));
#40009=CARTESIAN_POINT('Ctrl Pts',(-59.2392060275328,-119.890769476657,
179.954699160921));
#40010=CARTESIAN_POINT('Ctrl Pts',(-60.8839826877893,-119.809706524652,
180.159876802508));
#40011=CARTESIAN_POINT('Ctrl Pts',(-62.1941912418877,-119.764310767978,
179.142403412702));
#40012=CARTESIAN_POINT('Ctrl Pts',(-63.5043997959861,-119.718915011303,
178.124930022896));
#40013=CARTESIAN_POINT('Ctrl Pts',(-63.7183594249458,-119.790386713972,
176.480827714093));
#40014=CARTESIAN_POINT('Ctrl Pts',(-63.9323190539056,-119.861858416641,
174.83672540529));
#40015=CARTESIAN_POINT('Ctrl Pts',(-62.9305166913555,-120.062938469982,
173.529087012057));
#40016=CARTESIAN_POINT('Ctrl Pts',(-61.9287143288055,-120.264018523323,
172.221448618824));
#40017=CARTESIAN_POINT('Ctrl Pts',(-60.303813794383,-120.531525004638,172.016270977238));
#40018=CARTESIAN_POINT('Ctrl Pts',(-58.6789132599606,-120.799031485954,
171.811093335651));
#40019=CARTESIAN_POINT('Ctrl Pts',(-57.3885808316962,-121.030870771939,
172.828566725457));
#40020=CARTESIAN_POINT('Ctrl Pts',(-56.0982484034319,-121.262710057924,
173.846040115263));
#40021=CARTESIAN_POINT('Ctrl Pts',(-55.9041649003061,-121.377681884566,
175.490142424066));
#40022=CARTESIAN_POINT('Ctrl Pts',(-55.7100813971804,-121.492653711208,
177.134244732869));
#40023=CARTESIAN_POINT('Ctrl Pts',(-56.7317598855645,-121.478017187178,
178.441883126102));
#40024=CARTESIAN_POINT('Ctrl Pts',(-57.7534383739486,-121.463380663147,
179.749521519335));
#40025=CARTESIAN_POINT('Ctrl Pts',(-59.3982150342051,-121.382317711142,
179.954699160921));
#40026=CARTESIAN_POINT('Ctrl Pts',(-61.0429916944615,-121.301254759138,
180.159876802508));
#40027=CARTESIAN_POINT('Ctrl Pts',(-62.3532002485599,-121.255859002463,
179.142403412702));
#40028=CARTESIAN_POINT('Ctrl Pts',(-63.6634088026583,-121.210463245789,
178.124930022896));
#40029=CARTESIAN_POINT('Ctrl Pts',(-63.8773684316181,-121.281934948458,
176.480827714093));
#40030=CARTESIAN_POINT('Ctrl Pts',(-64.0913280605779,-121.353406651126,
174.83672540529));
#40031=CARTESIAN_POINT('Ctrl Pts',(-63.0895256980278,-121.554486704467,
173.529087012057));
#40032=CARTESIAN_POINT('Ctrl Pts',(-62.0877233354777,-121.755566757808,
172.221448618824));
#40033=CARTESIAN_POINT('Ctrl Pts',(-60.4628228010552,-122.023073239124,
172.016270977238));
#40034=CARTESIAN_POINT('Ctrl Pts',(-58.8379222666328,-122.290579720439,
171.811093335651));
#40035=CARTESIAN_POINT('Ctrl Pts',(-57.5475898383685,-122.522419006424,
172.828566725457));
#40036=CARTESIAN_POINT('Ctrl Pts',(-56.2572574101041,-122.754258292409,
173.846040115263));
#40037=CARTESIAN_POINT('Ctrl Pts',(-56.0631739069784,-122.869230119051,
175.490142424066));
#40038=CARTESIAN_POINT('Ctrl Pts',(-55.8690904038526,-122.984201945693,
177.134244732869));
#40039=CARTESIAN_POINT('Ctrl Pts',(-56.8907688922367,-122.969565421663,
178.441883126102));
#40040=CARTESIAN_POINT('Ctrl Pts',(-57.9124473806208,-122.954928897633,
179.749521519335));
#40041=CARTESIAN_POINT('Ctrl Pts',(-59.5572240408773,-122.873865945628,
179.954699160921));
#40042=CARTESIAN_POINT('Ctrl Pts',(-61.2020007011338,-122.792802993623,
180.159876802508));
#40043=CARTESIAN_POINT('Ctrl Pts',(-62.5122092552321,-122.747407236949,
179.142403412702));
#40044=CARTESIAN_POINT('Ctrl Pts',(-63.8224178093305,-122.702011480275,
178.124930022896));
#40045=CARTESIAN_POINT('Ctrl Pts',(-64.0363774382903,-122.773483182943,
176.480827714093));
#40046=CARTESIAN_POINT('Ctrl Pts',(-64.2503370672501,-122.844954885612,
174.83672540529));
#40047=CARTESIAN_POINT('Ctrl Pts',(-63.2485347047,-123.046034938953,173.529087012057));
#40048=CARTESIAN_POINT('Ctrl Pts',(-62.2467323421499,-123.247114992294,
172.221448618824));
#40049=CARTESIAN_POINT('Ctrl Pts',(-60.6218318077275,-123.514621473609,
172.016270977238));
#40050=CARTESIAN_POINT('Ctrl Pts',(-58.996931273305,-123.782127954925,171.811093335651));
#40051=CARTESIAN_POINT('Ctrl Pts',(-57.7065988450407,-124.01396724091,172.828566725457));
#40052=CARTESIAN_POINT('Ctrl Pts',(-56.4162664167763,-124.245806526895,
173.846040115263));
#40053=CARTESIAN_POINT('Ctrl Pts',(-56.2221829136506,-124.360778353537,
175.490142424066));
#40054=CARTESIAN_POINT('Ctrl Pts',(-56.0280994105248,-124.475750180179,
177.134244732869));
#40055=CARTESIAN_POINT('Ctrl Pts',(-57.049777898909,-124.461113656149,178.441883126102));
#40056=CARTESIAN_POINT('Ctrl Pts',(-58.0714563872931,-124.446477132119,
179.749521519335));
#40057=CARTESIAN_POINT('Ctrl Pts',(-59.7162330475495,-124.365414180114,
179.954699160921));
#40058=CARTESIAN_POINT('Ctrl Pts',(-61.361009707806,-124.284351228109,180.159876802508));
#40059=CARTESIAN_POINT('Ctrl Pts',(-62.6712182619044,-124.238955471435,
179.142403412702));
#40060=CARTESIAN_POINT('Ctrl Pts',(-63.9814268160028,-124.19355971476,178.124930022896));
#40061=CARTESIAN_POINT('Ctrl Pts',(-64.1953864449625,-124.265031417429,
176.480827714093));
#40062=CARTESIAN_POINT('Ctrl Pts',(-64.4093460739223,-124.336503120098,
174.83672540529));
#40063=CARTESIAN_POINT('Ctrl Pts',(-63.4075437113722,-124.537583173439,
173.529087012057));
#40064=CARTESIAN_POINT('Ctrl Pts',(-62.4057413488222,-124.73866322678,172.221448618824));
#40065=CARTESIAN_POINT('Ctrl Pts',(-60.7808408143997,-125.006169708095,
172.016270977238));
#40066=CARTESIAN_POINT('Ctrl Pts',(-59.1559402799773,-125.273676189411,
171.811093335651));
#40067=CARTESIAN_POINT('Ctrl Pts',(-57.8656078517129,-125.505515475396,
172.828566725457));
#40068=CARTESIAN_POINT('Ctrl Pts',(-56.5752754234486,-125.737354761381,
173.846040115263));
#40069=CARTESIAN_POINT('Ctrl Pts',(-56.3811919203228,-125.852326588023,
175.490142424066));
#40070=CARTESIAN_POINT('Ctrl Pts',(-56.1871084171971,-125.967298414665,
177.134244732869));
#40071=CARTESIAN_POINT('Ctrl Pts',(-57.2087869055812,-125.952661890634,
178.441883126102));
#40072=CARTESIAN_POINT('Ctrl Pts',(-58.2304653939653,-125.938025366604,
179.749521519335));
#40073=CARTESIAN_POINT('Ctrl Pts',(-59.8752420542218,-125.856962414599,
179.954699160921));
#40074=CARTESIAN_POINT('Ctrl Pts',(-61.5200187144782,-125.775899462594,
180.159876802508));
#40075=CARTESIAN_POINT('Ctrl Pts',(-62.8302272685766,-125.73050370592,179.142403412702));
#40076=CARTESIAN_POINT('Ctrl Pts',(-64.140435822675,-125.685107949246,178.124930022896));
#40077=CARTESIAN_POINT('Ctrl Pts',(-64.3543954516348,-125.756579651915,
176.480827714093));
#40078=CARTESIAN_POINT('Ctrl Pts',(-64.5683550805945,-125.828051354583,
174.83672540529));
#40079=CARTESIAN_POINT('Ctrl Pts',(-63.5665527180444,-126.029131407924,
173.529087012057));
#40080=CARTESIAN_POINT('Ctrl Pts',(-62.5647503554944,-126.230211461265,
172.221448618824));
#40081=CARTESIAN_POINT('Ctrl Pts',(-60.9398498210719,-126.497717942581,
172.016270977238));
#40082=CARTESIAN_POINT('Ctrl Pts',(-59.3149492866495,-126.765224423896,
171.811093335651));
#40083=CARTESIAN_POINT('Ctrl Pts',(-58.0246168583851,-126.997063709881,
172.828566725457));
#40084=CARTESIAN_POINT('Ctrl Pts',(-56.7342844301208,-127.228902995866,
173.846040115263));
#40085=CARTESIAN_POINT('Ctrl Pts',(-56.5402009269951,-127.343874822508,
175.490142424066));
#40086=CARTESIAN_POINT('Ctrl Pts',(-56.3461174238693,-127.45884664915,177.134244732869));
#40087=CARTESIAN_POINT('Ctrl Pts',(-57.3677959122534,-127.44421012512,178.441883126102));
#40088=CARTESIAN_POINT('Ctrl Pts',(-58.3894744006375,-127.42957360109,179.749521519335));
#40089=CARTESIAN_POINT('Ctrl Pts',(-60.034251060894,-127.348510649085,179.954699160921));
#40090=CARTESIAN_POINT('Ctrl Pts',(-61.6790277211505,-127.26744769708,180.159876802508));
#40091=CARTESIAN_POINT('Ctrl Pts',(-62.9892362752488,-127.222051940406,
179.142403412702));
#40092=CARTESIAN_POINT('Ctrl Pts',(-64.2994448293472,-127.176656183731,
178.124930022896));
#40093=CARTESIAN_POINT('Ctrl Pts',(-64.513404458307,-127.2481278864,176.480827714093));
#40094=CARTESIAN_POINT('Ctrl Pts',(-64.7273640872667,-127.319599589069,
174.83672540529));
#40095=CARTESIAN_POINT('Ctrl Pts',(-63.7255617247167,-127.52067964241,173.529087012057));
#40096=CARTESIAN_POINT('Ctrl Pts',(-62.7237593621666,-127.721759695751,
172.221448618824));
#40097=CARTESIAN_POINT('Ctrl Pts',(-61.0988588277442,-127.989266177066,
172.016270977238));
#40098=CARTESIAN_POINT('Ctrl Pts',(-59.4739582933217,-128.256772658382,
171.811093335651));
#40099=CARTESIAN_POINT('Ctrl Pts',(-58.1836258650574,-128.488611944367,
172.828566725457));
#40100=CARTESIAN_POINT('Ctrl Pts',(-56.893293436793,-128.720451230352,173.846040115263));
#40101=CARTESIAN_POINT('Ctrl Pts',(-56.6992099336673,-128.835423056994,
175.490142424066));
#40102=CARTESIAN_POINT('Ctrl Pts',(-56.5051264305415,-128.950394883636,
177.134244732869));
#40103=CARTESIAN_POINT('Ctrl Pts',(-57.5268049189256,-128.935758359606,
178.441883126102));
#40104=CARTESIAN_POINT('Ctrl Pts',(-58.5484834073098,-128.921121835575,
179.749521519335));
#40105=CARTESIAN_POINT('Ctrl Pts',(-60.1932600675662,-128.84005888357,179.954699160921));
#40106=CARTESIAN_POINT('Ctrl Pts',(-61.8380367278227,-128.758995931566,
180.159876802508));
#40107=CARTESIAN_POINT('Ctrl Pts',(-63.1482452819211,-128.713600174891,
179.142403412702));
#40108=CARTESIAN_POINT('Ctrl Pts',(-64.4584538360194,-128.668204418217,
178.124930022896));
#40109=CARTESIAN_POINT('Ctrl Pts',(-64.6724134649792,-128.739676120886,
176.480827714093));
#40110=CARTESIAN_POINT('Ctrl Pts',(-64.886373093939,-128.811147823554,174.83672540529));
#40111=CARTESIAN_POINT('Ctrl Pts',(-63.8845707313889,-129.012227876895,
173.529087012057));
#40112=CARTESIAN_POINT('Ctrl Pts',(-62.8827683688388,-129.213307930236,
172.221448618824));
#40113=CARTESIAN_POINT('Ctrl Pts',(-61.2578678344164,-129.480814411552,
172.016270977238));
#40114=CARTESIAN_POINT('Ctrl Pts',(-59.632967299994,-129.748320892867,171.811093335651));
#40115=CARTESIAN_POINT('Ctrl Pts',(-58.3426348717296,-129.980160178852,
172.828566725457));
#40116=CARTESIAN_POINT('Ctrl Pts',(-57.0523024434653,-130.211999464837,
173.846040115263));
#40117=CARTESIAN_POINT('Ctrl Pts',(-56.8582189403395,-130.326971291479,
175.490142424066));
#40118=CARTESIAN_POINT('Ctrl Pts',(-56.6641354372138,-130.441943118121,
177.134244732869));
#40119=CARTESIAN_POINT('Ctrl Pts',(-57.6858139255979,-130.427306594091,
178.441883126102));
#40120=CARTESIAN_POINT('Ctrl Pts',(-58.707492413982,-130.412670070061,179.749521519335));
#40121=CARTESIAN_POINT('Ctrl Pts',(-60.3522690742384,-130.331607118056,
179.954699160921));
#40122=CARTESIAN_POINT('Ctrl Pts',(-61.9970457344949,-130.250544166051,
180.159876802508));
#40123=CARTESIAN_POINT('Ctrl Pts',(-63.3072542885933,-130.205148409377,
179.142403412702));
#40124=CARTESIAN_POINT('Ctrl Pts',(-64.6174628426917,-130.159752652703,
178.124930022896));
#40125=CARTESIAN_POINT('Ctrl Pts',(-64.8314224716514,-130.231224355371,
176.480827714093));
#40126=CARTESIAN_POINT('Ctrl Pts',(-65.0453821006112,-130.30269605804,174.83672540529));
#40127=CARTESIAN_POINT('Ctrl Pts',(-64.0435797380611,-130.503776111381,
173.529087012057));
#40128=CARTESIAN_POINT('Ctrl Pts',(-63.041777375511,-130.704856164722,172.221448618824));
#40129=CARTESIAN_POINT('Ctrl Pts',(-61.4168768410886,-130.972362646037,
172.016270977238));
#40130=CARTESIAN_POINT('Ctrl Pts',(-59.7919763066662,-131.239869127353,
171.811093335651));
#40131=CARTESIAN_POINT('Ctrl Pts',(-58.5016438784018,-131.471708413338,
172.828566725457));
#40132=CARTESIAN_POINT('Ctrl Pts',(-57.2113114501375,-131.703547699323,
173.846040115263));
#40133=CARTESIAN_POINT('Ctrl Pts',(-57.0172279470117,-131.818519525965,
175.490142424066));
#40134=CARTESIAN_POINT('Ctrl Pts',(-56.823144443886,-131.933491352607,177.134244732869));
#40135=CARTESIAN_POINT('Ctrl Pts',(-57.8448229322701,-131.918854828577,
178.441883126102));
#40136=CARTESIAN_POINT('Ctrl Pts',(-58.8665014206542,-131.904218304546,
179.749521519335));
#40137=CARTESIAN_POINT('Ctrl Pts',(-60.5112780809107,-131.823155352542,
179.954699160921));
#40138=CARTESIAN_POINT('Ctrl Pts',(-61.5752386421509,-131.770717969403,
180.087422906321));
#40139=CARTESIAN_POINT('Ctrl Pts',(-62.5639794549305,-131.730759788555,
179.67061371833));
#40140=CARTESIAN_POINT('Ctrl Pts',(-51.1930600664641,-67.8253476561165,
175.613978758287));
#40141=CARTESIAN_POINT('Ctrl Pts',(-51.049982232031,-67.9348819377124,176.847053256227));
#40142=CARTESIAN_POINT('Ctrl Pts',(-51.8187242395064,-67.9472101323889,
177.827780274605));
#40143=CARTESIAN_POINT('Ctrl Pts',(-52.5874662469819,-67.9595383270654,
178.808507292983));
#40144=CARTESIAN_POINT('Ctrl Pts',(-53.8235310368257,-67.9220467910073,
178.96239024542));
#40145=CARTESIAN_POINT('Ctrl Pts',(-55.0595958266696,-67.8845552549492,
179.116273197858));
#40146=CARTESIAN_POINT('Ctrl Pts',(-56.0447349914363,-67.8738140669319,
178.353169537834));
#40147=CARTESIAN_POINT('Ctrl Pts',(-57.029874156203,-67.8630728789146,177.590065877811));
#40148=CARTESIAN_POINT('Ctrl Pts',(-57.1928281164701,-67.9399821266294,
176.356991379871));
#40149=CARTESIAN_POINT('Ctrl Pts',(-57.3557820767372,-68.0168913743442,
175.123916881932));
#40150=CARTESIAN_POINT('Ctrl Pts',(-56.6069161950958,-68.1910067089784,
174.143189863554));
#40151=CARTESIAN_POINT('Ctrl Pts',(-55.8580503134544,-68.3651220436126,
173.162462845176));
#40152=CARTESIAN_POINT('Ctrl Pts',(-54.6418616494445,-68.5890571089814,
173.008579892738));
#40153=CARTESIAN_POINT('Ctrl Pts',(-53.4256729854347,-68.8129921743502,
172.854696940301));
#40154=CARTESIAN_POINT('Ctrl Pts',(-52.460409946502,-69.0101768916782,173.617800600325));
#40155=CARTESIAN_POINT('Ctrl Pts',(-51.4951469075694,-69.2073616090062,
174.380904260348));
#40156=CARTESIAN_POINT('Ctrl Pts',(-51.3520690731363,-69.3168958906021,
175.613978758287));
#40157=CARTESIAN_POINT('Ctrl Pts',(-51.2089912387032,-69.426430172198,176.847053256227));
#40158=CARTESIAN_POINT('Ctrl Pts',(-51.9777332461786,-69.4387583668745,
177.827780274605));
#40159=CARTESIAN_POINT('Ctrl Pts',(-52.7464752536541,-69.451086561551,178.808507292983));
#40160=CARTESIAN_POINT('Ctrl Pts',(-53.9825400434979,-69.4135950254929,
178.96239024542));
#40161=CARTESIAN_POINT('Ctrl Pts',(-55.2186048333418,-69.3761034894348,
179.116273197858));
#40162=CARTESIAN_POINT('Ctrl Pts',(-56.2037439981085,-69.3653623014175,
178.353169537834));
#40163=CARTESIAN_POINT('Ctrl Pts',(-57.1888831628752,-69.3546211134002,
177.590065877811));
#40164=CARTESIAN_POINT('Ctrl Pts',(-57.3518371231423,-69.431530361115,176.356991379871));
#40165=CARTESIAN_POINT('Ctrl Pts',(-57.5147910834094,-69.5084396088298,
175.123916881932));
#40166=CARTESIAN_POINT('Ctrl Pts',(-56.765925201768,-69.682554943464,174.143189863554));
#40167=CARTESIAN_POINT('Ctrl Pts',(-56.0170593201266,-69.8566702780982,
173.162462845176));
#40168=CARTESIAN_POINT('Ctrl Pts',(-54.8008706561167,-70.080605343467,173.008579892738));
#40169=CARTESIAN_POINT('Ctrl Pts',(-53.5846819921069,-70.3045404088358,
172.854696940301));
#40170=CARTESIAN_POINT('Ctrl Pts',(-52.6194189531743,-70.5017251261638,
173.617800600325));
#40171=CARTESIAN_POINT('Ctrl Pts',(-51.6541559142416,-70.6989098434918,
174.380904260348));
#40172=CARTESIAN_POINT('Ctrl Pts',(-51.5110780798085,-70.8084441250877,
175.613978758287));
#40173=CARTESIAN_POINT('Ctrl Pts',(-51.3680002453754,-70.9179784066836,
176.847053256227));
#40174=CARTESIAN_POINT('Ctrl Pts',(-52.1367422528509,-70.9303066013601,
177.827780274605));
#40175=CARTESIAN_POINT('Ctrl Pts',(-52.9054842603263,-70.9426347960366,
178.808507292983));
#40176=CARTESIAN_POINT('Ctrl Pts',(-54.1415490501702,-70.9051432599785,
178.96239024542));
#40177=CARTESIAN_POINT('Ctrl Pts',(-55.377613840014,-70.8676517239204,179.116273197858));
#40178=CARTESIAN_POINT('Ctrl Pts',(-56.3627530047807,-70.8569105359031,
178.353169537834));
#40179=CARTESIAN_POINT('Ctrl Pts',(-57.3478921695474,-70.8461693478859,
177.590065877811));
#40180=CARTESIAN_POINT('Ctrl Pts',(-57.5108461298145,-70.9230785956006,
176.356991379871));
#40181=CARTESIAN_POINT('Ctrl Pts',(-57.6738000900816,-70.9999878433154,
175.123916881932));
#40182=CARTESIAN_POINT('Ctrl Pts',(-56.9249342084402,-71.1741031779496,
174.143189863554));
#40183=CARTESIAN_POINT('Ctrl Pts',(-56.1760683267988,-71.3482185125838,
173.162462845176));
#40184=CARTESIAN_POINT('Ctrl Pts',(-54.959879662789,-71.5721535779526,173.008579892738));
#40185=CARTESIAN_POINT('Ctrl Pts',(-53.7436909987791,-71.7960886433214,
172.854696940301));
#40186=CARTESIAN_POINT('Ctrl Pts',(-52.7784279598465,-71.9932733606494,
173.617800600325));
#40187=CARTESIAN_POINT('Ctrl Pts',(-51.8131649209138,-72.1904580779774,
174.380904260348));
#40188=CARTESIAN_POINT('Ctrl Pts',(-51.6700870864807,-72.2999923595733,
175.613978758287));
#40189=CARTESIAN_POINT('Ctrl Pts',(-51.5270092520476,-72.4095266411692,
176.847053256227));
#40190=CARTESIAN_POINT('Ctrl Pts',(-52.2957512595231,-72.4218548358457,
177.827780274605));
#40191=CARTESIAN_POINT('Ctrl Pts',(-53.0644932669986,-72.4341830305222,
178.808507292983));
#40192=CARTESIAN_POINT('Ctrl Pts',(-54.3005580568424,-72.3966914944641,
178.96239024542));
#40193=CARTESIAN_POINT('Ctrl Pts',(-55.5366228466863,-72.359199958406,179.116273197858));
#40194=CARTESIAN_POINT('Ctrl Pts',(-56.5217620114529,-72.3484587703887,
178.353169537834));
#40195=CARTESIAN_POINT('Ctrl Pts',(-57.5069011762196,-72.3377175823714,
177.590065877811));
#40196=CARTESIAN_POINT('Ctrl Pts',(-57.6698551364867,-72.4146268300862,
176.356991379871));
#40197=CARTESIAN_POINT('Ctrl Pts',(-57.8328090967539,-72.491536077801,175.123916881932));
#40198=CARTESIAN_POINT('Ctrl Pts',(-57.0839432151125,-72.6656514124352,
174.143189863554));
#40199=CARTESIAN_POINT('Ctrl Pts',(-56.335077333471,-72.8397667470694,173.162462845176));
#40200=CARTESIAN_POINT('Ctrl Pts',(-55.1188886694612,-73.0637018124382,
173.008579892738));
#40201=CARTESIAN_POINT('Ctrl Pts',(-53.9027000054514,-73.287636877807,172.854696940301));
#40202=CARTESIAN_POINT('Ctrl Pts',(-52.9374369665187,-73.484821595135,173.617800600325));
#40203=CARTESIAN_POINT('Ctrl Pts',(-51.9721739275861,-73.682006312463,174.380904260348));
#40204=CARTESIAN_POINT('Ctrl Pts',(-51.829096093153,-73.7915405940589,175.613978758287));
#40205=CARTESIAN_POINT('Ctrl Pts',(-51.6860182587199,-73.9010748756548,
176.847053256227));
#40206=CARTESIAN_POINT('Ctrl Pts',(-52.4547602661953,-73.9134030703313,
177.827780274605));
#40207=CARTESIAN_POINT('Ctrl Pts',(-53.2235022736708,-73.9257312650078,
178.808507292983));
#40208=CARTESIAN_POINT('Ctrl Pts',(-54.4595670635146,-73.8882397289497,
178.96239024542));
#40209=CARTESIAN_POINT('Ctrl Pts',(-55.6956318533585,-73.8507481928916,
179.116273197858));
#40210=CARTESIAN_POINT('Ctrl Pts',(-56.6807710181252,-73.8400070048743,
178.353169537834));
#40211=CARTESIAN_POINT('Ctrl Pts',(-57.6659101828918,-73.829265816857,177.590065877811));
#40212=CARTESIAN_POINT('Ctrl Pts',(-57.828864143159,-73.9061750645718,176.356991379871));
#40213=CARTESIAN_POINT('Ctrl Pts',(-57.9918181034261,-73.9830843122866,
175.123916881932));
#40214=CARTESIAN_POINT('Ctrl Pts',(-57.2429522217847,-74.1571996469208,
174.143189863554));
#40215=CARTESIAN_POINT('Ctrl Pts',(-56.4940863401433,-74.3313149815551,
173.162462845176));
#40216=CARTESIAN_POINT('Ctrl Pts',(-55.2778976761334,-74.5552500469238,
173.008579892738));
#40217=CARTESIAN_POINT('Ctrl Pts',(-54.0617090121236,-74.7791851122926,
172.854696940301));
#40218=CARTESIAN_POINT('Ctrl Pts',(-53.0964459731909,-74.9763698296206,
173.617800600325));
#40219=CARTESIAN_POINT('Ctrl Pts',(-52.1311829342583,-75.1735545469486,
174.380904260348));
#40220=CARTESIAN_POINT('Ctrl Pts',(-51.9881050998252,-75.2830888285445,
175.613978758287));
#40221=CARTESIAN_POINT('Ctrl Pts',(-51.8450272653921,-75.3926231101404,
176.847053256227));
#40222=CARTESIAN_POINT('Ctrl Pts',(-52.6137692728675,-75.4049513048169,
177.827780274605));
#40223=CARTESIAN_POINT('Ctrl Pts',(-53.382511280343,-75.4172794994934,178.808507292983));
#40224=CARTESIAN_POINT('Ctrl Pts',(-54.6185760701869,-75.3797879634353,
178.96239024542));
#40225=CARTESIAN_POINT('Ctrl Pts',(-55.8546408600307,-75.3422964273772,
179.116273197858));
#40226=CARTESIAN_POINT('Ctrl Pts',(-56.8397800247974,-75.3315552393599,
178.353169537834));
#40227=CARTESIAN_POINT('Ctrl Pts',(-57.8249191895641,-75.3208140513426,
177.590065877811));
#40228=CARTESIAN_POINT('Ctrl Pts',(-57.9878731498312,-75.3977232990574,
176.356991379871));
#40229=CARTESIAN_POINT('Ctrl Pts',(-58.1508271100983,-75.4746325467722,
175.123916881932));
#40230=CARTESIAN_POINT('Ctrl Pts',(-57.4019612284569,-75.6487478814064,
174.143189863554));
#40231=CARTESIAN_POINT('Ctrl Pts',(-56.6530953468155,-75.8228632160406,
173.162462845176));
#40232=CARTESIAN_POINT('Ctrl Pts',(-55.4369066828056,-76.0467982814094,
173.008579892738));
#40233=CARTESIAN_POINT('Ctrl Pts',(-54.2207180187958,-76.2707333467782,
172.854696940301));
#40234=CARTESIAN_POINT('Ctrl Pts',(-53.2554549798632,-76.4679180641062,
173.617800600325));
#40235=CARTESIAN_POINT('Ctrl Pts',(-52.2901919409305,-76.6651027814342,
174.380904260348));
#40236=CARTESIAN_POINT('Ctrl Pts',(-52.1471141064974,-76.7746370630301,
175.613978758287));
#40237=CARTESIAN_POINT('Ctrl Pts',(-52.0040362720643,-76.884171344626,176.847053256227));
#40238=CARTESIAN_POINT('Ctrl Pts',(-52.7727782795398,-76.8964995393025,
177.827780274605));
#40239=CARTESIAN_POINT('Ctrl Pts',(-53.5415202870152,-76.9088277339789,
178.808507292983));
#40240=CARTESIAN_POINT('Ctrl Pts',(-54.7775850768591,-76.8713361979209,
178.96239024542));
#40241=CARTESIAN_POINT('Ctrl Pts',(-56.013649866703,-76.8338446618628,179.116273197858));
#40242=CARTESIAN_POINT('Ctrl Pts',(-56.9987890314696,-76.8231034738455,
178.353169537834));
#40243=CARTESIAN_POINT('Ctrl Pts',(-57.9839281962363,-76.8123622858282,
177.590065877811));
#40244=CARTESIAN_POINT('Ctrl Pts',(-58.1468821565034,-76.8892715335431,
176.356991379871));
#40245=CARTESIAN_POINT('Ctrl Pts',(-58.3098361167706,-76.9661807812578,
175.123916881932));
#40246=CARTESIAN_POINT('Ctrl Pts',(-57.5609702351291,-77.140296115892,174.143189863554));
#40247=CARTESIAN_POINT('Ctrl Pts',(-56.8121043534877,-77.3144114505262,
173.162462845176));
#40248=CARTESIAN_POINT('Ctrl Pts',(-55.5959156894779,-77.538346515895,173.008579892738));
#40249=CARTESIAN_POINT('Ctrl Pts',(-54.379727025468,-77.7622815812638,172.854696940301));
#40250=CARTESIAN_POINT('Ctrl Pts',(-53.4144639865354,-77.9594662985918,
173.617800600325));
#40251=CARTESIAN_POINT('Ctrl Pts',(-52.4492009476028,-78.1566510159198,
174.380904260348));
#40252=CARTESIAN_POINT('Ctrl Pts',(-52.3061231131696,-78.2661852975157,
175.613978758287));
#40253=CARTESIAN_POINT('Ctrl Pts',(-52.1630452787365,-78.3757195791116,
176.847053256227));
#40254=CARTESIAN_POINT('Ctrl Pts',(-52.931787286212,-78.3880477737881,177.827780274605));
#40255=CARTESIAN_POINT('Ctrl Pts',(-53.7005292936875,-78.4003759684646,
178.808507292983));
#40256=CARTESIAN_POINT('Ctrl Pts',(-54.9365940835313,-78.3628844324065,
178.96239024542));
#40257=CARTESIAN_POINT('Ctrl Pts',(-56.1726588733752,-78.3253928963484,
179.116273197858));
#40258=CARTESIAN_POINT('Ctrl Pts',(-57.1577980381419,-78.3146517083311,
178.353169537834));
#40259=CARTESIAN_POINT('Ctrl Pts',(-58.1429372029085,-78.3039105203139,
177.590065877811));
#40260=CARTESIAN_POINT('Ctrl Pts',(-58.3058911631757,-78.3808197680286,
176.356991379871));
#40261=CARTESIAN_POINT('Ctrl Pts',(-58.4688451234428,-78.4577290157434,
175.123916881932));
#40262=CARTESIAN_POINT('Ctrl Pts',(-57.7199792418014,-78.6318443503776,
174.143189863554));
#40263=CARTESIAN_POINT('Ctrl Pts',(-56.9711133601599,-78.8059596850118,
173.162462845176));
#40264=CARTESIAN_POINT('Ctrl Pts',(-55.7549246961501,-79.0298947503806,
173.008579892738));
#40265=CARTESIAN_POINT('Ctrl Pts',(-54.5387360321403,-79.2538298157494,
172.854696940301));
#40266=CARTESIAN_POINT('Ctrl Pts',(-53.5734729932076,-79.4510145330774,
173.617800600325));
#40267=CARTESIAN_POINT('Ctrl Pts',(-52.608209954275,-79.6481992504054,174.380904260348));
#40268=CARTESIAN_POINT('Ctrl Pts',(-52.4651321198419,-79.7577335320013,
175.613978758287));
#40269=CARTESIAN_POINT('Ctrl Pts',(-52.3220542854088,-79.8672678135972,
176.847053256227));
#40270=CARTESIAN_POINT('Ctrl Pts',(-53.0907962928842,-79.8795960082737,
177.827780274605));
#40271=CARTESIAN_POINT('Ctrl Pts',(-53.8595383003597,-79.8919242029502,
178.808507292983));
#40272=CARTESIAN_POINT('Ctrl Pts',(-55.0956030902035,-79.8544326668921,
178.96239024542));
#40273=CARTESIAN_POINT('Ctrl Pts',(-56.3316678800474,-79.816941130834,179.116273197858));
#40274=CARTESIAN_POINT('Ctrl Pts',(-57.3168070448141,-79.8061999428167,
178.353169537834));
#40275=CARTESIAN_POINT('Ctrl Pts',(-58.3019462095808,-79.7954587547994,
177.590065877811));
#40276=CARTESIAN_POINT('Ctrl Pts',(-58.4649001698479,-79.8723680025142,
176.356991379871));
#40277=CARTESIAN_POINT('Ctrl Pts',(-58.627854130115,-79.949277250229,175.123916881932));
#40278=CARTESIAN_POINT('Ctrl Pts',(-57.8789882484736,-80.1233925848632,
174.143189863554));
#40279=CARTESIAN_POINT('Ctrl Pts',(-57.1301223668322,-80.2975079194974,
173.162462845176));
#40280=CARTESIAN_POINT('Ctrl Pts',(-55.9139337028223,-80.5214429848662,
173.008579892738));
#40281=CARTESIAN_POINT('Ctrl Pts',(-54.6977450388125,-80.745378050235,172.854696940301));
#40282=CARTESIAN_POINT('Ctrl Pts',(-53.7324819998798,-80.942562767563,173.617800600325));
#40283=CARTESIAN_POINT('Ctrl Pts',(-52.7672189609472,-81.139747484891,174.380904260348));
#40284=CARTESIAN_POINT('Ctrl Pts',(-52.6241411265141,-81.2492817664869,
175.613978758287));
#40285=CARTESIAN_POINT('Ctrl Pts',(-52.481063292081,-81.3588160480828,176.847053256227));
#40286=CARTESIAN_POINT('Ctrl Pts',(-53.2498052995565,-81.3711442427593,
177.827780274605));
#40287=CARTESIAN_POINT('Ctrl Pts',(-54.0185473070319,-81.3834724374358,
178.808507292983));
#40288=CARTESIAN_POINT('Ctrl Pts',(-55.2546120968758,-81.3459809013777,
178.96239024542));
#40289=CARTESIAN_POINT('Ctrl Pts',(-56.4906768867196,-81.3084893653196,
179.116273197858));
#40290=CARTESIAN_POINT('Ctrl Pts',(-57.4758160514863,-81.2977481773023,
178.353169537834));
#40291=CARTESIAN_POINT('Ctrl Pts',(-58.460955216253,-81.287006989285,177.590065877811));
#40292=CARTESIAN_POINT('Ctrl Pts',(-58.6239091765201,-81.3639162369998,
176.356991379871));
#40293=CARTESIAN_POINT('Ctrl Pts',(-58.7868631367872,-81.4408254847146,
175.123916881932));
#40294=CARTESIAN_POINT('Ctrl Pts',(-58.0379972551458,-81.6149408193488,
174.143189863554));
#40295=CARTESIAN_POINT('Ctrl Pts',(-57.2891313735044,-81.789056153983,173.162462845176));
#40296=CARTESIAN_POINT('Ctrl Pts',(-56.0729427094946,-82.0129912193518,
173.008579892738));
#40297=CARTESIAN_POINT('Ctrl Pts',(-54.8567540454847,-82.2369262847206,
172.854696940301));
#40298=CARTESIAN_POINT('Ctrl Pts',(-53.8914910065521,-82.4341110020486,
173.617800600325));
#40299=CARTESIAN_POINT('Ctrl Pts',(-52.9262279676194,-82.6312957193766,
174.380904260348));
#40300=CARTESIAN_POINT('Ctrl Pts',(-52.7831501331863,-82.7408300009725,
175.613978758287));
#40301=CARTESIAN_POINT('Ctrl Pts',(-52.6400722987532,-82.8503642825684,
176.847053256227));
#40302=CARTESIAN_POINT('Ctrl Pts',(-53.4088143062287,-82.8626924772449,
177.827780274605));
#40303=CARTESIAN_POINT('Ctrl Pts',(-54.1775563137041,-82.8750206719214,
178.808507292983));
#40304=CARTESIAN_POINT('Ctrl Pts',(-55.413621103548,-82.8375291358633,178.96239024542));
#40305=CARTESIAN_POINT('Ctrl Pts',(-56.6496858933919,-82.8000375998052,
179.116273197858));
#40306=CARTESIAN_POINT('Ctrl Pts',(-57.6348250581585,-82.7892964117879,
178.353169537834));
#40307=CARTESIAN_POINT('Ctrl Pts',(-58.6199642229252,-82.7785552237706,
177.590065877811));
#40308=CARTESIAN_POINT('Ctrl Pts',(-58.7829181831923,-82.8554644714854,
176.356991379871));
#40309=CARTESIAN_POINT('Ctrl Pts',(-58.9458721434595,-82.9323737192003,
175.123916881932));
#40310=CARTESIAN_POINT('Ctrl Pts',(-58.197006261818,-83.1064890538344,174.143189863554));
#40311=CARTESIAN_POINT('Ctrl Pts',(-57.4481403801766,-83.2806043884686,
173.162462845176));
#40312=CARTESIAN_POINT('Ctrl Pts',(-56.2319517161668,-83.5045394538374,
173.008579892738));
#40313=CARTESIAN_POINT('Ctrl Pts',(-55.0157630521569,-83.7284745192062,
172.854696940301));
#40314=CARTESIAN_POINT('Ctrl Pts',(-54.0505000132243,-83.9256592365342,
173.617800600325));
#40315=CARTESIAN_POINT('Ctrl Pts',(-53.0852369742917,-84.1228439538622,
174.380904260348));
#40316=CARTESIAN_POINT('Ctrl Pts',(-52.9421591398586,-84.2323782354581,
175.613978758287));
#40317=CARTESIAN_POINT('Ctrl Pts',(-52.7990813054255,-84.341912517054,176.847053256227));
#40318=CARTESIAN_POINT('Ctrl Pts',(-53.5678233129009,-84.3542407117305,
177.827780274605));
#40319=CARTESIAN_POINT('Ctrl Pts',(-54.3365653203764,-84.3665689064069,
178.808507292983));
#40320=CARTESIAN_POINT('Ctrl Pts',(-55.5726301102202,-84.3290773703489,
178.96239024542));
#40321=CARTESIAN_POINT('Ctrl Pts',(-56.8086949000641,-84.2915858342908,
179.116273197858));
#40322=CARTESIAN_POINT('Ctrl Pts',(-57.7938340648308,-84.2808446462735,
178.353169537834));
#40323=CARTESIAN_POINT('Ctrl Pts',(-58.7789732295974,-84.2701034582562,
177.590065877811));
#40324=CARTESIAN_POINT('Ctrl Pts',(-58.9419271898646,-84.347012705971,176.356991379871));
#40325=CARTESIAN_POINT('Ctrl Pts',(-59.1048811501317,-84.4239219536858,
175.123916881932));
#40326=CARTESIAN_POINT('Ctrl Pts',(-58.3560152684903,-84.59803728832,174.143189863554));
#40327=CARTESIAN_POINT('Ctrl Pts',(-57.6071493868488,-84.7721526229542,
173.162462845176));
#40328=CARTESIAN_POINT('Ctrl Pts',(-56.390960722839,-84.996087688323,173.008579892738));
#40329=CARTESIAN_POINT('Ctrl Pts',(-55.1747720588292,-85.2200227536918,
172.854696940301));
#40330=CARTESIAN_POINT('Ctrl Pts',(-54.2095090198965,-85.4172074710198,
173.617800600325));
#40331=CARTESIAN_POINT('Ctrl Pts',(-53.2442459809639,-85.6143921883478,
174.380904260348));
#40332=CARTESIAN_POINT('Ctrl Pts',(-53.1011681465308,-85.7239264699437,
175.613978758287));
#40333=CARTESIAN_POINT('Ctrl Pts',(-52.9580903120977,-85.8334607515396,
176.847053256227));
#40334=CARTESIAN_POINT('Ctrl Pts',(-53.7268323195731,-85.8457889462161,
177.827780274605));
#40335=CARTESIAN_POINT('Ctrl Pts',(-54.4955743270486,-85.8581171408926,
178.808507292983));
#40336=CARTESIAN_POINT('Ctrl Pts',(-55.7316391168925,-85.8206256048345,
178.96239024542));
#40337=CARTESIAN_POINT('Ctrl Pts',(-56.9677039067363,-85.7831340687764,
179.116273197858));
#40338=CARTESIAN_POINT('Ctrl Pts',(-57.952843071503,-85.7723928807591,178.353169537834));
#40339=CARTESIAN_POINT('Ctrl Pts',(-58.9379822362697,-85.7616516927418,
177.590065877811));
#40340=CARTESIAN_POINT('Ctrl Pts',(-59.1009361965368,-85.8385609404566,
176.356991379871));
#40341=CARTESIAN_POINT('Ctrl Pts',(-59.2638901568039,-85.9154701881714,
175.123916881932));
#40342=CARTESIAN_POINT('Ctrl Pts',(-58.5150242751625,-86.0895855228056,
174.143189863554));
#40343=CARTESIAN_POINT('Ctrl Pts',(-57.7661583935211,-86.2637008574398,
173.162462845176));
#40344=CARTESIAN_POINT('Ctrl Pts',(-56.5499697295112,-86.4876359228086,
173.008579892738));
#40345=CARTESIAN_POINT('Ctrl Pts',(-55.3337810655014,-86.7115709881774,
172.854696940301));
#40346=CARTESIAN_POINT('Ctrl Pts',(-54.3685180265688,-86.9087557055054,
173.617800600325));
#40347=CARTESIAN_POINT('Ctrl Pts',(-53.4032549876361,-87.1059404228334,
174.380904260348));
#40348=CARTESIAN_POINT('Ctrl Pts',(-53.260177153203,-87.2154747044293,175.613978758287));
#40349=CARTESIAN_POINT('Ctrl Pts',(-53.1170993187699,-87.3250089860252,
176.847053256227));
#40350=CARTESIAN_POINT('Ctrl Pts',(-53.8858413262454,-87.3373371807017,
177.827780274605));
#40351=CARTESIAN_POINT('Ctrl Pts',(-54.6545833337208,-87.3496653753782,
178.808507292983));
#40352=CARTESIAN_POINT('Ctrl Pts',(-55.8906481235647,-87.3121738393201,
178.96239024542));
#40353=CARTESIAN_POINT('Ctrl Pts',(-57.1267129134086,-87.274682303262,179.116273197858));
#40354=CARTESIAN_POINT('Ctrl Pts',(-58.1118520781752,-87.2639411152447,
178.353169537834));
#40355=CARTESIAN_POINT('Ctrl Pts',(-59.0969912429419,-87.2531999272274,
177.590065877811));
#40356=CARTESIAN_POINT('Ctrl Pts',(-59.259945203209,-87.3301091749422,176.356991379871));
#40357=CARTESIAN_POINT('Ctrl Pts',(-59.4228991634762,-87.407018422657,175.123916881932));
#40358=CARTESIAN_POINT('Ctrl Pts',(-58.6740332818347,-87.5811337572912,
174.143189863554));
#40359=CARTESIAN_POINT('Ctrl Pts',(-57.9251674001933,-87.7552490919254,
173.162462845176));
#40360=CARTESIAN_POINT('Ctrl Pts',(-56.7089787361835,-87.9791841572942,
173.008579892738));
#40361=CARTESIAN_POINT('Ctrl Pts',(-55.4927900721736,-88.203119222663,172.854696940301));
#40362=CARTESIAN_POINT('Ctrl Pts',(-54.527527033241,-88.400303939991,173.617800600325));
#40363=CARTESIAN_POINT('Ctrl Pts',(-53.5622639943083,-88.597488657319,174.380904260348));
#40364=CARTESIAN_POINT('Ctrl Pts',(-53.4191861598752,-88.7070229389149,
175.613978758287));
#40365=CARTESIAN_POINT('Ctrl Pts',(-53.2761083254422,-88.8165572205108,
176.847053256227));
#40366=CARTESIAN_POINT('Ctrl Pts',(-54.0448503329176,-88.8288854151873,
177.827780274605));
#40367=CARTESIAN_POINT('Ctrl Pts',(-54.813592340393,-88.8412136098638,178.808507292983));
#40368=CARTESIAN_POINT('Ctrl Pts',(-56.0496571302369,-88.8037220738057,
178.96239024542));
#40369=CARTESIAN_POINT('Ctrl Pts',(-57.2857219200808,-88.7662305377476,
179.116273197858));
#40370=CARTESIAN_POINT('Ctrl Pts',(-58.2708610848475,-88.7554893497303,
178.353169537834));
#40371=CARTESIAN_POINT('Ctrl Pts',(-59.2560002496141,-88.7447481617131,
177.590065877811));
#40372=CARTESIAN_POINT('Ctrl Pts',(-59.4189542098812,-88.8216574094278,
176.356991379871));
#40373=CARTESIAN_POINT('Ctrl Pts',(-59.5819081701484,-88.8985666571426,
175.123916881932));
#40374=CARTESIAN_POINT('Ctrl Pts',(-58.833042288507,-89.0726819917768,174.143189863554));
#40375=CARTESIAN_POINT('Ctrl Pts',(-58.0841764068655,-89.246797326411,173.162462845176));
#40376=CARTESIAN_POINT('Ctrl Pts',(-56.8679877428557,-89.4707323917798,
173.008579892738));
#40377=CARTESIAN_POINT('Ctrl Pts',(-55.6517990788459,-89.6946674571486,
172.854696940301));
#40378=CARTESIAN_POINT('Ctrl Pts',(-54.6865360399132,-89.8918521744766,
173.617800600325));
#40379=CARTESIAN_POINT('Ctrl Pts',(-53.7212730009806,-90.0890368918046,
174.380904260348));
#40380=CARTESIAN_POINT('Ctrl Pts',(-53.5781951665475,-90.1985711734005,
175.613978758287));
#40381=CARTESIAN_POINT('Ctrl Pts',(-53.4351173321144,-90.3081054549964,
176.847053256227));
#40382=CARTESIAN_POINT('Ctrl Pts',(-54.2038593395898,-90.3204336496729,
177.827780274605));
#40383=CARTESIAN_POINT('Ctrl Pts',(-54.9726013470653,-90.3327618443494,
178.808507292983));
#40384=CARTESIAN_POINT('Ctrl Pts',(-56.2086661369091,-90.2952703082913,
178.96239024542));
#40385=CARTESIAN_POINT('Ctrl Pts',(-57.444730926753,-90.2577787722332,179.116273197858));
#40386=CARTESIAN_POINT('Ctrl Pts',(-58.4298700915197,-90.2470375842159,
178.353169537834));
#40387=CARTESIAN_POINT('Ctrl Pts',(-59.4150092562863,-90.2362963961987,
177.590065877811));
#40388=CARTESIAN_POINT('Ctrl Pts',(-59.5779632165535,-90.3132056439134,
176.356991379871));
#40389=CARTESIAN_POINT('Ctrl Pts',(-59.7409171768206,-90.3901148916282,
175.123916881932));
#40390=CARTESIAN_POINT('Ctrl Pts',(-58.9920512951792,-90.5642302262624,
174.143189863554));
#40391=CARTESIAN_POINT('Ctrl Pts',(-58.2431854135378,-90.7383455608967,
173.162462845176));
#40392=CARTESIAN_POINT('Ctrl Pts',(-57.0269967495279,-90.9622806262654,
173.008579892738));
#40393=CARTESIAN_POINT('Ctrl Pts',(-55.8108080855181,-91.1862156916342,
172.854696940301));
#40394=CARTESIAN_POINT('Ctrl Pts',(-54.8455450465854,-91.3834004089622,
173.617800600325));
#40395=CARTESIAN_POINT('Ctrl Pts',(-53.8802820076528,-91.5805851262902,
174.380904260348));
#40396=CARTESIAN_POINT('Ctrl Pts',(-53.7372041732197,-91.6901194078861,
175.613978758287));
#40397=CARTESIAN_POINT('Ctrl Pts',(-53.5941263387866,-91.799653689482,176.847053256227));
#40398=CARTESIAN_POINT('Ctrl Pts',(-54.362868346262,-91.8119818841585,177.827780274605));
#40399=CARTESIAN_POINT('Ctrl Pts',(-55.1316103537375,-91.824310078835,178.808507292983));
#40400=CARTESIAN_POINT('Ctrl Pts',(-56.3676751435814,-91.7868185427769,
178.96239024542));
#40401=CARTESIAN_POINT('Ctrl Pts',(-57.6037399334252,-91.7493270067188,
179.116273197858));
#40402=CARTESIAN_POINT('Ctrl Pts',(-58.5888790981919,-91.7385858187015,
178.353169537834));
#40403=CARTESIAN_POINT('Ctrl Pts',(-59.5740182629586,-91.7278446306843,
177.590065877811));
#40404=CARTESIAN_POINT('Ctrl Pts',(-59.7369722232257,-91.804753878399,176.356991379871));
#40405=CARTESIAN_POINT('Ctrl Pts',(-59.8999261834928,-91.8816631261138,
175.123916881932));
#40406=CARTESIAN_POINT('Ctrl Pts',(-59.1510603018514,-92.055778460748,174.143189863554));
#40407=CARTESIAN_POINT('Ctrl Pts',(-58.40219442021,-92.2298937953823,173.162462845176));
#40408=CARTESIAN_POINT('Ctrl Pts',(-57.1860057562002,-92.453828860751,173.008579892738));
#40409=CARTESIAN_POINT('Ctrl Pts',(-55.9698170921903,-92.6777639261198,
172.854696940301));
#40410=CARTESIAN_POINT('Ctrl Pts',(-55.0045540532577,-92.8749486434478,
173.617800600325));
#40411=CARTESIAN_POINT('Ctrl Pts',(-54.039291014325,-93.0721333607758,174.380904260348));
#40412=CARTESIAN_POINT('Ctrl Pts',(-53.8962131798919,-93.1816676423717,
175.613978758287));
#40413=CARTESIAN_POINT('Ctrl Pts',(-53.7531353454588,-93.2912019239676,
176.847053256227));
#40414=CARTESIAN_POINT('Ctrl Pts',(-54.5218773529343,-93.3035301186441,
177.827780274605));
#40415=CARTESIAN_POINT('Ctrl Pts',(-55.2906193604097,-93.3158583133206,
178.808507292983));
#40416=CARTESIAN_POINT('Ctrl Pts',(-56.5266841502536,-93.2783667772625,
178.96239024542));
#40417=CARTESIAN_POINT('Ctrl Pts',(-57.7627489400975,-93.2408752412044,
179.116273197858));
#40418=CARTESIAN_POINT('Ctrl Pts',(-58.7478881048641,-93.2301340531871,
178.353169537834));
#40419=CARTESIAN_POINT('Ctrl Pts',(-59.7330272696308,-93.2193928651699,
177.590065877811));
#40420=CARTESIAN_POINT('Ctrl Pts',(-59.8959812298979,-93.2963021128846,
176.356991379871));
#40421=CARTESIAN_POINT('Ctrl Pts',(-60.0589351901651,-93.3732113605994,
175.123916881932));
#40422=CARTESIAN_POINT('Ctrl Pts',(-59.3100693085236,-93.5473266952337,
174.143189863554));
#40423=CARTESIAN_POINT('Ctrl Pts',(-58.5612034268822,-93.7214420298679,
173.162462845176));
#40424=CARTESIAN_POINT('Ctrl Pts',(-57.3450147628724,-93.9453770952366,
173.008579892738));
#40425=CARTESIAN_POINT('Ctrl Pts',(-56.1288260988625,-94.1693121606054,
172.854696940301));
#40426=CARTESIAN_POINT('Ctrl Pts',(-55.1635630599299,-94.3664968779334,
173.617800600325));
#40427=CARTESIAN_POINT('Ctrl Pts',(-54.1983000209973,-94.5636815952613,
174.380904260348));
#40428=CARTESIAN_POINT('Ctrl Pts',(-54.0552221865641,-94.6732158768573,
175.613978758287));
#40429=CARTESIAN_POINT('Ctrl Pts',(-53.9121443521311,-94.7827501584532,
176.847053256227));
#40430=CARTESIAN_POINT('Ctrl Pts',(-54.6808863596065,-94.7950783531297,
177.827780274605));
#40431=CARTESIAN_POINT('Ctrl Pts',(-55.4496283670819,-94.8074065478062,
178.808507292983));
#40432=CARTESIAN_POINT('Ctrl Pts',(-56.6856931569258,-94.7699150117481,
178.96239024542));
#40433=CARTESIAN_POINT('Ctrl Pts',(-57.9217579467697,-94.73242347569,179.116273197858));
#40434=CARTESIAN_POINT('Ctrl Pts',(-58.9068971115363,-94.7216822876727,
178.353169537834));
#40435=CARTESIAN_POINT('Ctrl Pts',(-59.892036276303,-94.7109410996555,177.590065877811));
#40436=CARTESIAN_POINT('Ctrl Pts',(-60.0549902365702,-94.7878503473702,
176.356991379871));
#40437=CARTESIAN_POINT('Ctrl Pts',(-60.2179441968373,-94.864759595085,175.123916881932));
#40438=CARTESIAN_POINT('Ctrl Pts',(-59.4690783151959,-95.0388749297192,
174.143189863554));
#40439=CARTESIAN_POINT('Ctrl Pts',(-58.7202124335545,-95.2129902643534,
173.162462845176));
#40440=CARTESIAN_POINT('Ctrl Pts',(-57.5040237695446,-95.4369253297222,
173.008579892738));
#40441=CARTESIAN_POINT('Ctrl Pts',(-56.2878351055348,-95.660860395091,172.854696940301));
#40442=CARTESIAN_POINT('Ctrl Pts',(-55.3225720666021,-95.858045112419,173.617800600325));
#40443=CARTESIAN_POINT('Ctrl Pts',(-54.3573090276695,-96.055229829747,174.380904260348));
#40444=CARTESIAN_POINT('Ctrl Pts',(-54.2142311932364,-96.1647641113429,
175.613978758287));
#40445=CARTESIAN_POINT('Ctrl Pts',(-54.0711533588033,-96.2742983929388,
176.847053256227));
#40446=CARTESIAN_POINT('Ctrl Pts',(-54.8398953662787,-96.2866265876153,
177.827780274605));
#40447=CARTESIAN_POINT('Ctrl Pts',(-55.6086373737542,-96.2989547822918,
178.808507292983));
#40448=CARTESIAN_POINT('Ctrl Pts',(-56.844702163598,-96.2614632462337,178.96239024542));
#40449=CARTESIAN_POINT('Ctrl Pts',(-58.0807669534419,-96.2239717101756,
179.116273197858));
#40450=CARTESIAN_POINT('Ctrl Pts',(-59.0659061182086,-96.2132305221583,
178.353169537834));
#40451=CARTESIAN_POINT('Ctrl Pts',(-60.0510452829753,-96.202489334141,177.590065877811));
#40452=CARTESIAN_POINT('Ctrl Pts',(-60.2139992432424,-96.2793985818558,
176.356991379871));
#40453=CARTESIAN_POINT('Ctrl Pts',(-60.3769532035095,-96.3563078295706,
175.123916881932));
#40454=CARTESIAN_POINT('Ctrl Pts',(-59.6280873218681,-96.5304231642048,
174.143189863554));
#40455=CARTESIAN_POINT('Ctrl Pts',(-58.8792214402267,-96.7045384988391,
173.162462845176));
#40456=CARTESIAN_POINT('Ctrl Pts',(-57.6630327762168,-96.9284735642078,
173.008579892738));
#40457=CARTESIAN_POINT('Ctrl Pts',(-56.446844112207,-97.1524086295766,172.854696940301));
#40458=CARTESIAN_POINT('Ctrl Pts',(-55.4815810732743,-97.3495933469046,
173.617800600325));
#40459=CARTESIAN_POINT('Ctrl Pts',(-54.5163180343417,-97.5467780642326,
174.380904260348));
#40460=CARTESIAN_POINT('Ctrl Pts',(-54.3732401999086,-97.6563123458285,
175.613978758287));
#40461=CARTESIAN_POINT('Ctrl Pts',(-54.2301623654755,-97.7658466274244,
176.847053256227));
#40462=CARTESIAN_POINT('Ctrl Pts',(-54.9989043729509,-97.7781748221009,
177.827780274605));
#40463=CARTESIAN_POINT('Ctrl Pts',(-55.7676463804264,-97.7905030167774,
178.808507292983));
#40464=CARTESIAN_POINT('Ctrl Pts',(-57.0037111702703,-97.7530114807193,
178.96239024542));
#40465=CARTESIAN_POINT('Ctrl Pts',(-58.2397759601141,-97.7155199446612,
179.116273197858));
#40466=CARTESIAN_POINT('Ctrl Pts',(-59.2249151248808,-97.7047787566439,
178.353169537834));
#40467=CARTESIAN_POINT('Ctrl Pts',(-60.2100542896475,-97.6940375686266,
177.590065877811));
#40468=CARTESIAN_POINT('Ctrl Pts',(-60.3730082499146,-97.7709468163415,
176.356991379871));
#40469=CARTESIAN_POINT('Ctrl Pts',(-60.5359622101818,-97.8478560640562,
175.123916881932));
#40470=CARTESIAN_POINT('Ctrl Pts',(-59.7870963285403,-98.0219713986905,
174.143189863554));
#40471=CARTESIAN_POINT('Ctrl Pts',(-59.0382304468989,-98.1960867333247,
173.162462845176));
#40472=CARTESIAN_POINT('Ctrl Pts',(-57.8220417828891,-98.4200217986935,
173.008579892738));
#40473=CARTESIAN_POINT('Ctrl Pts',(-56.6058531188792,-98.6439568640622,
172.854696940301));
#40474=CARTESIAN_POINT('Ctrl Pts',(-55.6405900799466,-98.8411415813902,
173.617800600325));
#40475=CARTESIAN_POINT('Ctrl Pts',(-54.6753270410139,-99.0383262987182,
174.380904260348));
#40476=CARTESIAN_POINT('Ctrl Pts',(-54.5322492065808,-99.1478605803141,
175.613978758287));
#40477=CARTESIAN_POINT('Ctrl Pts',(-54.3891713721477,-99.25739486191,176.847053256227));
#40478=CARTESIAN_POINT('Ctrl Pts',(-55.1579133796232,-99.2697230565865,
177.827780274605));
#40479=CARTESIAN_POINT('Ctrl Pts',(-55.9266553870986,-99.282051251263,178.808507292983));
#40480=CARTESIAN_POINT('Ctrl Pts',(-57.1627201769425,-99.2445597152049,
178.96239024542));
#40481=CARTESIAN_POINT('Ctrl Pts',(-58.3987849667864,-99.2070681791468,
179.116273197858));
#40482=CARTESIAN_POINT('Ctrl Pts',(-59.383924131553,-99.1963269911295,178.353169537834));
#40483=CARTESIAN_POINT('Ctrl Pts',(-60.3690632963197,-99.1855858031122,
177.590065877811));
#40484=CARTESIAN_POINT('Ctrl Pts',(-60.5320172565868,-99.2624950508271,
176.356991379871));
#40485=CARTESIAN_POINT('Ctrl Pts',(-60.694971216854,-99.3394042985418,175.123916881932));
#40486=CARTESIAN_POINT('Ctrl Pts',(-59.9461053352125,-99.513519633176,174.143189863554));
#40487=CARTESIAN_POINT('Ctrl Pts',(-59.1972394535711,-99.6876349678102,
173.162462845176));
#40488=CARTESIAN_POINT('Ctrl Pts',(-57.9810507895613,-99.9115700331791,
173.008579892738));
#40489=CARTESIAN_POINT('Ctrl Pts',(-56.7648621255514,-100.135505098548,
172.854696940301));
#40490=CARTESIAN_POINT('Ctrl Pts',(-55.7995990866188,-100.332689815876,
173.617800600325));
#40491=CARTESIAN_POINT('Ctrl Pts',(-54.8343360476862,-100.529874533204,
174.380904260348));
#40492=CARTESIAN_POINT('Ctrl Pts',(-54.6912582132531,-100.6394088148,175.613978758287));
#40493=CARTESIAN_POINT('Ctrl Pts',(-54.54818037882,-100.748943096396,176.847053256227));
#40494=CARTESIAN_POINT('Ctrl Pts',(-55.3169223862954,-100.761271291072,
177.827780274605));
#40495=CARTESIAN_POINT('Ctrl Pts',(-56.0856643937708,-100.773599485749,
178.808507292983));
#40496=CARTESIAN_POINT('Ctrl Pts',(-57.3217291836147,-100.73610794969,178.96239024542));
#40497=CARTESIAN_POINT('Ctrl Pts',(-58.5577939734586,-100.698616413632,
179.116273197858));
#40498=CARTESIAN_POINT('Ctrl Pts',(-59.5429331382253,-100.687875225615,
178.353169537834));
#40499=CARTESIAN_POINT('Ctrl Pts',(-60.5280723029919,-100.677134037598,
177.590065877811));
#40500=CARTESIAN_POINT('Ctrl Pts',(-60.6910262632591,-100.754043285313,
176.356991379871));
#40501=CARTESIAN_POINT('Ctrl Pts',(-60.8539802235262,-100.830952533027,
175.123916881932));
#40502=CARTESIAN_POINT('Ctrl Pts',(-60.1051143418848,-101.005067867662,
174.143189863554));
#40503=CARTESIAN_POINT('Ctrl Pts',(-59.3562484602434,-101.179183202296,
173.162462845176));
#40504=CARTESIAN_POINT('Ctrl Pts',(-58.1400597962335,-101.403118267665,
173.008579892738));
#40505=CARTESIAN_POINT('Ctrl Pts',(-56.9238711322237,-101.627053333033,
172.854696940301));
#40506=CARTESIAN_POINT('Ctrl Pts',(-55.958608093291,-101.824238050361,173.617800600325));
#40507=CARTESIAN_POINT('Ctrl Pts',(-54.9933450543584,-102.021422767689,
174.380904260348));
#40508=CARTESIAN_POINT('Ctrl Pts',(-54.8502672199253,-102.130957049285,
175.613978758287));
#40509=CARTESIAN_POINT('Ctrl Pts',(-54.7071893854922,-102.240491330881,
176.847053256227));
#40510=CARTESIAN_POINT('Ctrl Pts',(-55.4759313929676,-102.252819525558,
177.827780274605));
#40511=CARTESIAN_POINT('Ctrl Pts',(-56.2446734004431,-102.265147720234,
178.808507292983));
#40512=CARTESIAN_POINT('Ctrl Pts',(-57.480738190287,-102.227656184176,178.96239024542));
#40513=CARTESIAN_POINT('Ctrl Pts',(-58.7168029801308,-102.190164648118,
179.116273197858));
#40514=CARTESIAN_POINT('Ctrl Pts',(-59.7019421448975,-102.179423460101,
178.353169537834));
#40515=CARTESIAN_POINT('Ctrl Pts',(-60.6870813096642,-102.168682272083,
177.590065877811));
#40516=CARTESIAN_POINT('Ctrl Pts',(-60.8500352699313,-102.245591519798,
176.356991379871));
#40517=CARTESIAN_POINT('Ctrl Pts',(-61.0129892301984,-102.322500767513,
175.123916881932));
#40518=CARTESIAN_POINT('Ctrl Pts',(-60.264123348557,-102.496616102147,174.143189863554));
#40519=CARTESIAN_POINT('Ctrl Pts',(-59.5152574669156,-102.670731436781,
173.162462845176));
#40520=CARTESIAN_POINT('Ctrl Pts',(-58.2990688029057,-102.89466650215,173.008579892738));
#40521=CARTESIAN_POINT('Ctrl Pts',(-57.0828801388959,-103.118601567519,
172.854696940301));
#40522=CARTESIAN_POINT('Ctrl Pts',(-56.1176170999633,-103.315786284847,
173.617800600325));
#40523=CARTESIAN_POINT('Ctrl Pts',(-55.1523540610306,-103.512971002175,
174.380904260348));
#40524=CARTESIAN_POINT('Ctrl Pts',(-55.0092762265975,-103.622505283771,
175.613978758287));
#40525=CARTESIAN_POINT('Ctrl Pts',(-54.8661983921644,-103.732039565367,
176.847053256227));
#40526=CARTESIAN_POINT('Ctrl Pts',(-55.6349403996399,-103.744367760043,
177.827780274605));
#40527=CARTESIAN_POINT('Ctrl Pts',(-56.4036824071153,-103.75669595472,178.808507292983));
#40528=CARTESIAN_POINT('Ctrl Pts',(-57.6397471969592,-103.719204418662,
178.96239024542));
#40529=CARTESIAN_POINT('Ctrl Pts',(-58.8758119868031,-103.681712882604,
179.116273197858));
#40530=CARTESIAN_POINT('Ctrl Pts',(-59.8609511515697,-103.670971694586,
178.353169537834));
#40531=CARTESIAN_POINT('Ctrl Pts',(-60.8460903163364,-103.660230506569,
177.590065877811));
#40532=CARTESIAN_POINT('Ctrl Pts',(-61.0090442766035,-103.737139754284,
176.356991379871));
#40533=CARTESIAN_POINT('Ctrl Pts',(-61.1719982368707,-103.814049001999,
175.123916881932));
#40534=CARTESIAN_POINT('Ctrl Pts',(-60.4231323552292,-103.988164336633,
174.143189863554));
#40535=CARTESIAN_POINT('Ctrl Pts',(-59.6742664735878,-104.162279671267,
173.162462845176));
#40536=CARTESIAN_POINT('Ctrl Pts',(-58.458077809578,-104.386214736636,173.008579892738));
#40537=CARTESIAN_POINT('Ctrl Pts',(-57.2418891455681,-104.610149802005,
172.854696940301));
#40538=CARTESIAN_POINT('Ctrl Pts',(-56.2766261066355,-104.807334519333,
173.617800600325));
#40539=CARTESIAN_POINT('Ctrl Pts',(-55.3113630677028,-105.004519236661,
174.380904260348));
#40540=CARTESIAN_POINT('Ctrl Pts',(-55.1682852332697,-105.114053518257,
175.613978758287));
#40541=CARTESIAN_POINT('Ctrl Pts',(-55.0252073988366,-105.223587799852,
176.847053256227));
#40542=CARTESIAN_POINT('Ctrl Pts',(-55.7939494063121,-105.235915994529,
177.827780274605));
#40543=CARTESIAN_POINT('Ctrl Pts',(-56.5626914137875,-105.248244189205,
178.808507292983));
#40544=CARTESIAN_POINT('Ctrl Pts',(-57.7987562036314,-105.210752653147,
178.96239024542));
#40545=CARTESIAN_POINT('Ctrl Pts',(-59.0348209934753,-105.173261117089,
179.116273197858));
#40546=CARTESIAN_POINT('Ctrl Pts',(-60.0199601582419,-105.162519929072,
178.353169537834));
#40547=CARTESIAN_POINT('Ctrl Pts',(-61.0050993230086,-105.151778741055,
177.590065877811));
#40548=CARTESIAN_POINT('Ctrl Pts',(-61.1680532832757,-105.228687988769,
176.356991379871));
#40549=CARTESIAN_POINT('Ctrl Pts',(-61.3310072435429,-105.305597236484,
175.123916881932));
#40550=CARTESIAN_POINT('Ctrl Pts',(-60.5821413619014,-105.479712571118,
174.143189863554));
#40551=CARTESIAN_POINT('Ctrl Pts',(-59.83327548026,-105.653827905753,173.162462845176));
#40552=CARTESIAN_POINT('Ctrl Pts',(-58.6170868162502,-105.877762971121,
173.008579892738));
#40553=CARTESIAN_POINT('Ctrl Pts',(-57.4008981522404,-106.10169803649,172.854696940301));
#40554=CARTESIAN_POINT('Ctrl Pts',(-56.4356351133077,-106.298882753818,
173.617800600325));
#40555=CARTESIAN_POINT('Ctrl Pts',(-55.4703720743751,-106.496067471146,
174.380904260348));
#40556=CARTESIAN_POINT('Ctrl Pts',(-55.327294239942,-106.605601752742,175.613978758287));
#40557=CARTESIAN_POINT('Ctrl Pts',(-55.1842164055089,-106.715136034338,
176.847053256227));
#40558=CARTESIAN_POINT('Ctrl Pts',(-55.9529584129843,-106.727464229014,
177.827780274605));
#40559=CARTESIAN_POINT('Ctrl Pts',(-56.7217004204598,-106.739792423691,
178.808507292983));
#40560=CARTESIAN_POINT('Ctrl Pts',(-57.9577652103036,-106.702300887633,
178.96239024542));
#40561=CARTESIAN_POINT('Ctrl Pts',(-59.1938300001475,-106.664809351575,
179.116273197858));
#40562=CARTESIAN_POINT('Ctrl Pts',(-60.1789691649142,-106.654068163558,
178.353169537834));
#40563=CARTESIAN_POINT('Ctrl Pts',(-61.1641083296808,-106.64332697554,177.590065877811));
#40564=CARTESIAN_POINT('Ctrl Pts',(-61.327062289948,-106.720236223255,176.356991379871));
#40565=CARTESIAN_POINT('Ctrl Pts',(-61.4900162502151,-106.79714547097,175.123916881932));
#40566=CARTESIAN_POINT('Ctrl Pts',(-60.7411503685737,-106.971260805604,
174.143189863554));
#40567=CARTESIAN_POINT('Ctrl Pts',(-59.9922844869323,-107.145376140238,
173.162462845176));
#40568=CARTESIAN_POINT('Ctrl Pts',(-58.7760958229224,-107.369311205607,
173.008579892738));
#40569=CARTESIAN_POINT('Ctrl Pts',(-57.5599071589126,-107.593246270976,
172.854696940301));
#40570=CARTESIAN_POINT('Ctrl Pts',(-56.5946441199799,-107.790430988304,
173.617800600325));
#40571=CARTESIAN_POINT('Ctrl Pts',(-55.6293810810473,-107.987615705632,
174.380904260348));
#40572=CARTESIAN_POINT('Ctrl Pts',(-55.4863032466142,-108.097149987228,
175.613978758287));
#40573=CARTESIAN_POINT('Ctrl Pts',(-55.3432254121811,-108.206684268824,
176.847053256227));
#40574=CARTESIAN_POINT('Ctrl Pts',(-56.1119674196565,-108.2190124635,177.827780274605));
#40575=CARTESIAN_POINT('Ctrl Pts',(-56.880709427132,-108.231340658177,178.808507292983));
#40576=CARTESIAN_POINT('Ctrl Pts',(-58.1167742169759,-108.193849122118,
178.96239024542));
#40577=CARTESIAN_POINT('Ctrl Pts',(-59.3528390068197,-108.15635758606,179.116273197858));
#40578=CARTESIAN_POINT('Ctrl Pts',(-60.3379781715864,-108.145616398043,
178.353169537834));
#40579=CARTESIAN_POINT('Ctrl Pts',(-61.3231173363531,-108.134875210026,
177.590065877811));
#40580=CARTESIAN_POINT('Ctrl Pts',(-61.4860712966202,-108.211784457741,
176.356991379871));
#40581=CARTESIAN_POINT('Ctrl Pts',(-61.6490252568873,-108.288693705455,
175.123916881932));
#40582=CARTESIAN_POINT('Ctrl Pts',(-60.9001593752459,-108.46280904009,174.143189863554));
#40583=CARTESIAN_POINT('Ctrl Pts',(-60.1512934936045,-108.636924374724,
173.162462845176));
#40584=CARTESIAN_POINT('Ctrl Pts',(-58.9351048295946,-108.860859440093,
173.008579892738));
#40585=CARTESIAN_POINT('Ctrl Pts',(-57.7189161655848,-109.084794505461,
172.854696940301));
#40586=CARTESIAN_POINT('Ctrl Pts',(-56.7536531266522,-109.281979222789,
173.617800600325));
#40587=CARTESIAN_POINT('Ctrl Pts',(-55.7883900877195,-109.479163940117,
174.380904260348));
#40588=CARTESIAN_POINT('Ctrl Pts',(-55.6453122532864,-109.588698221713,
175.613978758287));
#40589=CARTESIAN_POINT('Ctrl Pts',(-55.5022344188533,-109.698232503309,
176.847053256227));
#40590=CARTESIAN_POINT('Ctrl Pts',(-56.2709764263288,-109.710560697986,
177.827780274605));
#40591=CARTESIAN_POINT('Ctrl Pts',(-57.0397184338042,-109.722888892662,
178.808507292983));
#40592=CARTESIAN_POINT('Ctrl Pts',(-58.2757832236481,-109.685397356604,
178.96239024542));
#40593=CARTESIAN_POINT('Ctrl Pts',(-59.511848013492,-109.647905820546,179.116273197858));
#40594=CARTESIAN_POINT('Ctrl Pts',(-60.4969871782586,-109.637164632529,
178.353169537834));
#40595=CARTESIAN_POINT('Ctrl Pts',(-61.4821263430253,-109.626423444511,
177.590065877811));
#40596=CARTESIAN_POINT('Ctrl Pts',(-61.6450803032924,-109.703332692226,
176.356991379871));
#40597=CARTESIAN_POINT('Ctrl Pts',(-61.8080342635596,-109.780241939941,
175.123916881932));
#40598=CARTESIAN_POINT('Ctrl Pts',(-61.0591683819181,-109.954357274575,
174.143189863554));
#40599=CARTESIAN_POINT('Ctrl Pts',(-60.3103025002767,-110.128472609209,
173.162462845176));
#40600=CARTESIAN_POINT('Ctrl Pts',(-59.0941138362669,-110.352407674578,
173.008579892738));
#40601=CARTESIAN_POINT('Ctrl Pts',(-57.877925172257,-110.576342739947,172.854696940301));
#40602=CARTESIAN_POINT('Ctrl Pts',(-56.9126621333244,-110.773527457275,
173.617800600325));
#40603=CARTESIAN_POINT('Ctrl Pts',(-55.9473990943918,-110.970712174603,
174.380904260348));
#40604=CARTESIAN_POINT('Ctrl Pts',(-55.8043212599587,-111.080246456199,
175.613978758287));
#40605=CARTESIAN_POINT('Ctrl Pts',(-55.6612434255256,-111.189780737795,
176.847053256227));
#40606=CARTESIAN_POINT('Ctrl Pts',(-56.429985433001,-111.202108932471,177.827780274605));
#40607=CARTESIAN_POINT('Ctrl Pts',(-57.1987274404764,-111.214437127148,
178.808507292983));
#40608=CARTESIAN_POINT('Ctrl Pts',(-58.4347922303203,-111.17694559109,178.96239024542));
#40609=CARTESIAN_POINT('Ctrl Pts',(-59.6708570201642,-111.139454055032,
179.116273197858));
#40610=CARTESIAN_POINT('Ctrl Pts',(-60.6559961849309,-111.128712867014,
178.353169537834));
#40611=CARTESIAN_POINT('Ctrl Pts',(-61.6411353496975,-111.117971678997,
177.590065877811));
#40612=CARTESIAN_POINT('Ctrl Pts',(-61.8040893099646,-111.194880926712,
176.356991379871));
#40613=CARTESIAN_POINT('Ctrl Pts',(-61.9670432702318,-111.271790174427,
175.123916881932));
#40614=CARTESIAN_POINT('Ctrl Pts',(-61.2181773885904,-111.445905509061,
174.143189863554));
#40615=CARTESIAN_POINT('Ctrl Pts',(-60.4693115069489,-111.620020843695,
173.162462845176));
#40616=CARTESIAN_POINT('Ctrl Pts',(-59.2531228429391,-111.843955909064,
173.008579892738));
#40617=CARTESIAN_POINT('Ctrl Pts',(-58.0369341789293,-112.067890974433,
172.854696940301));
#40618=CARTESIAN_POINT('Ctrl Pts',(-57.0716711399966,-112.265075691761,
173.617800600325));
#40619=CARTESIAN_POINT('Ctrl Pts',(-56.106408101064,-112.462260409089,174.380904260348));
#40620=CARTESIAN_POINT('Ctrl Pts',(-55.9633302666309,-112.571794690684,
175.613978758287));
#40621=CARTESIAN_POINT('Ctrl Pts',(-55.8202524321978,-112.68132897228,176.847053256227));
#40622=CARTESIAN_POINT('Ctrl Pts',(-56.5889944396732,-112.693657166957,
177.827780274605));
#40623=CARTESIAN_POINT('Ctrl Pts',(-57.3577364471487,-112.705985361633,
178.808507292983));
#40624=CARTESIAN_POINT('Ctrl Pts',(-58.5938012369925,-112.668493825575,
178.96239024542));
#40625=CARTESIAN_POINT('Ctrl Pts',(-59.8298660268364,-112.631002289517,
179.116273197858));
#40626=CARTESIAN_POINT('Ctrl Pts',(-60.8150051916031,-112.6202611015,178.353169537834));
#40627=CARTESIAN_POINT('Ctrl Pts',(-61.8001443563698,-112.609519913483,
177.590065877811));
#40628=CARTESIAN_POINT('Ctrl Pts',(-61.9630983166369,-112.686429161197,
176.356991379871));
#40629=CARTESIAN_POINT('Ctrl Pts',(-62.126052276904,-112.763338408912,175.123916881932));
#40630=CARTESIAN_POINT('Ctrl Pts',(-61.3771863952626,-112.937453743546,
174.143189863554));
#40631=CARTESIAN_POINT('Ctrl Pts',(-60.6283205136212,-113.111569078181,
173.162462845176));
#40632=CARTESIAN_POINT('Ctrl Pts',(-59.4121318496113,-113.335504143549,
173.008579892738));
#40633=CARTESIAN_POINT('Ctrl Pts',(-58.1959431856015,-113.559439208918,
172.854696940301));
#40634=CARTESIAN_POINT('Ctrl Pts',(-57.2306801466688,-113.756623926246,
173.617800600325));
#40635=CARTESIAN_POINT('Ctrl Pts',(-56.2654171077362,-113.953808643574,
174.380904260348));
#40636=CARTESIAN_POINT('Ctrl Pts',(-56.1223392733031,-114.06334292517,175.613978758287));
#40637=CARTESIAN_POINT('Ctrl Pts',(-55.97926143887,-114.172877206766,176.847053256227));
#40638=CARTESIAN_POINT('Ctrl Pts',(-56.7480034463455,-114.185205401443,
177.827780274605));
#40639=CARTESIAN_POINT('Ctrl Pts',(-57.5167454538209,-114.197533596119,
178.808507292983));
#40640=CARTESIAN_POINT('Ctrl Pts',(-58.7528102436648,-114.160042060061,
178.96239024542));
#40641=CARTESIAN_POINT('Ctrl Pts',(-59.9888750335086,-114.122550524003,
179.116273197858));
#40642=CARTESIAN_POINT('Ctrl Pts',(-60.9740141982753,-114.111809335986,
178.353169537834));
#40643=CARTESIAN_POINT('Ctrl Pts',(-61.959153363042,-114.101068147968,177.590065877811));
#40644=CARTESIAN_POINT('Ctrl Pts',(-62.1221073233091,-114.177977395683,
176.356991379871));
#40645=CARTESIAN_POINT('Ctrl Pts',(-62.2850612835762,-114.254886643398,
175.123916881932));
#40646=CARTESIAN_POINT('Ctrl Pts',(-61.5361954019348,-114.429001978032,
174.143189863554));
#40647=CARTESIAN_POINT('Ctrl Pts',(-60.7873295202934,-114.603117312666,
173.162462845176));
#40648=CARTESIAN_POINT('Ctrl Pts',(-59.5711408562835,-114.827052378035,
173.008579892738));
#40649=CARTESIAN_POINT('Ctrl Pts',(-58.3549521922737,-115.050987443404,
172.854696940301));
#40650=CARTESIAN_POINT('Ctrl Pts',(-57.3896891533411,-115.248172160732,
173.617800600325));
#40651=CARTESIAN_POINT('Ctrl Pts',(-56.4244261144084,-115.44535687806,174.380904260348));
#40652=CARTESIAN_POINT('Ctrl Pts',(-56.2813482799753,-115.554891159656,
175.613978758287));
#40653=CARTESIAN_POINT('Ctrl Pts',(-56.1382704455422,-115.664425441252,
176.847053256227));
#40654=CARTESIAN_POINT('Ctrl Pts',(-56.9070124530177,-115.676753635928,
177.827780274605));
#40655=CARTESIAN_POINT('Ctrl Pts',(-57.6757544604931,-115.689081830605,
178.808507292983));
#40656=CARTESIAN_POINT('Ctrl Pts',(-58.911819250337,-115.651590294547,178.96239024542));
#40657=CARTESIAN_POINT('Ctrl Pts',(-60.1478840401809,-115.614098758488,
179.116273197858));
#40658=CARTESIAN_POINT('Ctrl Pts',(-61.1330232049475,-115.603357570471,
178.353169537834));
#40659=CARTESIAN_POINT('Ctrl Pts',(-62.1181623697142,-115.592616382454,
177.590065877811));
#40660=CARTESIAN_POINT('Ctrl Pts',(-62.2811163299813,-115.669525630169,
176.356991379871));
#40661=CARTESIAN_POINT('Ctrl Pts',(-62.4440702902485,-115.746434877883,
175.123916881932));
#40662=CARTESIAN_POINT('Ctrl Pts',(-61.695204408607,-115.920550212518,174.143189863554));
#40663=CARTESIAN_POINT('Ctrl Pts',(-60.9463385269656,-116.094665547152,
173.162462845176));
#40664=CARTESIAN_POINT('Ctrl Pts',(-59.7301498629558,-116.318600612521,
173.008579892738));
#40665=CARTESIAN_POINT('Ctrl Pts',(-58.5139611989459,-116.542535677889,
172.854696940301));
#40666=CARTESIAN_POINT('Ctrl Pts',(-57.5486981600133,-116.739720395217,
173.617800600325));
#40667=CARTESIAN_POINT('Ctrl Pts',(-56.5834351210807,-116.936905112545,
174.380904260348));
#40668=CARTESIAN_POINT('Ctrl Pts',(-56.4403572866476,-117.046439394141,
175.613978758287));
#40669=CARTESIAN_POINT('Ctrl Pts',(-56.2972794522145,-117.155973675737,
176.847053256227));
#40670=CARTESIAN_POINT('Ctrl Pts',(-57.0660214596899,-117.168301870414,
177.827780274605));
#40671=CARTESIAN_POINT('Ctrl Pts',(-57.8347634671653,-117.18063006509,178.808507292983));
#40672=CARTESIAN_POINT('Ctrl Pts',(-59.0708282570092,-117.143138529032,
178.96239024542));
#40673=CARTESIAN_POINT('Ctrl Pts',(-60.3068930468531,-117.105646992974,
179.116273197858));
#40674=CARTESIAN_POINT('Ctrl Pts',(-61.2920322116198,-117.094905804957,
178.353169537834));
#40675=CARTESIAN_POINT('Ctrl Pts',(-62.2771713763864,-117.084164616939,
177.590065877811));
#40676=CARTESIAN_POINT('Ctrl Pts',(-62.4401253366536,-117.161073864654,
176.356991379871));
#40677=CARTESIAN_POINT('Ctrl Pts',(-62.6030792969207,-117.237983112369,
175.123916881932));
#40678=CARTESIAN_POINT('Ctrl Pts',(-61.8542134152793,-117.412098447003,
174.143189863554));
#40679=CARTESIAN_POINT('Ctrl Pts',(-61.1053475336379,-117.586213781637,
173.162462845176));
#40680=CARTESIAN_POINT('Ctrl Pts',(-59.889158869628,-117.810148847006,173.008579892738));
#40681=CARTESIAN_POINT('Ctrl Pts',(-58.6729702056182,-118.034083912375,
172.854696940301));
#40682=CARTESIAN_POINT('Ctrl Pts',(-57.7077071666855,-118.231268629703,
173.617800600325));
#40683=CARTESIAN_POINT('Ctrl Pts',(-56.7424441277529,-118.428453347031,
174.380904260348));
#40684=CARTESIAN_POINT('Ctrl Pts',(-56.5993662933198,-118.537987628627,
175.613978758287));
#40685=CARTESIAN_POINT('Ctrl Pts',(-56.4562884588867,-118.647521910223,
176.847053256227));
#40686=CARTESIAN_POINT('Ctrl Pts',(-57.2250304663621,-118.659850104899,
177.827780274605));
#40687=CARTESIAN_POINT('Ctrl Pts',(-57.9937724738376,-118.672178299576,
178.808507292983));
#40688=CARTESIAN_POINT('Ctrl Pts',(-59.2298372636814,-118.634686763518,
178.96239024542));
#40689=CARTESIAN_POINT('Ctrl Pts',(-60.4659020535253,-118.59719522746,179.116273197858));
#40690=CARTESIAN_POINT('Ctrl Pts',(-61.451041218292,-118.586454039442,178.353169537834));
#40691=CARTESIAN_POINT('Ctrl Pts',(-62.4361803830587,-118.575712851425,
177.590065877811));
#40692=CARTESIAN_POINT('Ctrl Pts',(-62.5991343433258,-118.65262209914,176.356991379871));
#40693=CARTESIAN_POINT('Ctrl Pts',(-62.7620883035929,-118.729531346855,
175.123916881932));
#40694=CARTESIAN_POINT('Ctrl Pts',(-62.0132224219515,-118.903646681489,
174.143189863554));
#40695=CARTESIAN_POINT('Ctrl Pts',(-61.2643565403101,-119.077762016123,
173.162462845176));
#40696=CARTESIAN_POINT('Ctrl Pts',(-60.0481678763002,-119.301697081492,
173.008579892738));
#40697=CARTESIAN_POINT('Ctrl Pts',(-58.8319792122904,-119.525632146861,
172.854696940301));
#40698=CARTESIAN_POINT('Ctrl Pts',(-57.8667161733577,-119.722816864189,
173.617800600325));
#40699=CARTESIAN_POINT('Ctrl Pts',(-56.9014531344251,-119.920001581517,
174.380904260348));
#40700=CARTESIAN_POINT('Ctrl Pts',(-56.758375299992,-120.029535863112,175.613978758287));
#40701=CARTESIAN_POINT('Ctrl Pts',(-56.6152974655589,-120.139070144708,
176.847053256227));
#40702=CARTESIAN_POINT('Ctrl Pts',(-57.3840394730344,-120.151398339385,
177.827780274605));
#40703=CARTESIAN_POINT('Ctrl Pts',(-58.1527814805098,-120.163726534061,
178.808507292983));
#40704=CARTESIAN_POINT('Ctrl Pts',(-59.3888462703537,-120.126234998003,
178.96239024542));
#40705=CARTESIAN_POINT('Ctrl Pts',(-60.6249110601976,-120.088743461945,
179.116273197858));
#40706=CARTESIAN_POINT('Ctrl Pts',(-61.6100502249642,-120.078002273928,
178.353169537834));
#40707=CARTESIAN_POINT('Ctrl Pts',(-62.5951893897309,-120.067261085911,
177.590065877811));
#40708=CARTESIAN_POINT('Ctrl Pts',(-62.758143349998,-120.144170333625,176.356991379871));
#40709=CARTESIAN_POINT('Ctrl Pts',(-62.9210973102652,-120.22107958134,175.123916881932));
#40710=CARTESIAN_POINT('Ctrl Pts',(-62.1722314286237,-120.395194915974,
174.143189863554));
#40711=CARTESIAN_POINT('Ctrl Pts',(-61.4233655469823,-120.569310250609,
173.162462845176));
#40712=CARTESIAN_POINT('Ctrl Pts',(-60.2071768829725,-120.793245315977,
173.008579892738));
#40713=CARTESIAN_POINT('Ctrl Pts',(-58.9909882189626,-121.017180381346,
172.854696940301));
#40714=CARTESIAN_POINT('Ctrl Pts',(-58.02572518003,-121.214365098674,173.617800600325));
#40715=CARTESIAN_POINT('Ctrl Pts',(-57.0604621410973,-121.411549816002,
174.380904260348));
#40716=CARTESIAN_POINT('Ctrl Pts',(-56.9173843066642,-121.521084097598,
175.613978758287));
#40717=CARTESIAN_POINT('Ctrl Pts',(-56.7743064722311,-121.630618379194,
176.847053256227));
#40718=CARTESIAN_POINT('Ctrl Pts',(-57.5430484797066,-121.64294657387,177.827780274605));
#40719=CARTESIAN_POINT('Ctrl Pts',(-58.3117904871821,-121.655274768547,
178.808507292983));
#40720=CARTESIAN_POINT('Ctrl Pts',(-59.5478552770259,-121.617783232489,
178.96239024542));
#40721=CARTESIAN_POINT('Ctrl Pts',(-60.7839200668698,-121.580291696431,
179.116273197858));
#40722=CARTESIAN_POINT('Ctrl Pts',(-61.7690592316364,-121.569550508414,
178.353169537834));
#40723=CARTESIAN_POINT('Ctrl Pts',(-62.7541983964031,-121.558809320396,
177.590065877811));
#40724=CARTESIAN_POINT('Ctrl Pts',(-62.9171523566702,-121.635718568111,
176.356991379871));
#40725=CARTESIAN_POINT('Ctrl Pts',(-63.0801063169374,-121.712627815826,
175.123916881932));
#40726=CARTESIAN_POINT('Ctrl Pts',(-62.331240435296,-121.88674315046,174.143189863554));
#40727=CARTESIAN_POINT('Ctrl Pts',(-61.5823745536545,-122.060858485094,
173.162462845176));
#40728=CARTESIAN_POINT('Ctrl Pts',(-60.3661858896447,-122.284793550463,
173.008579892738));
#40729=CARTESIAN_POINT('Ctrl Pts',(-59.1499972256349,-122.508728615832,
172.854696940301));
#40730=CARTESIAN_POINT('Ctrl Pts',(-58.1847341867022,-122.70591333316,173.617800600325));
#40731=CARTESIAN_POINT('Ctrl Pts',(-57.2194711477696,-122.903098050488,
174.380904260348));
#40732=CARTESIAN_POINT('Ctrl Pts',(-57.0763933133365,-123.012632332084,
175.613978758287));
#40733=CARTESIAN_POINT('Ctrl Pts',(-56.9333154789034,-123.12216661368,176.847053256227));
#40734=CARTESIAN_POINT('Ctrl Pts',(-57.7020574863788,-123.134494808356,
177.827780274605));
#40735=CARTESIAN_POINT('Ctrl Pts',(-58.4707994938543,-123.146823003033,
178.808507292983));
#40736=CARTESIAN_POINT('Ctrl Pts',(-59.7068642836981,-123.109331466974,
178.96239024542));
#40737=CARTESIAN_POINT('Ctrl Pts',(-60.942929073542,-123.071839930916,179.116273197858));
#40738=CARTESIAN_POINT('Ctrl Pts',(-61.9280682383087,-123.061098742899,
178.353169537834));
#40739=CARTESIAN_POINT('Ctrl Pts',(-62.9132074030754,-123.050357554882,
177.590065877811));
#40740=CARTESIAN_POINT('Ctrl Pts',(-63.0761613633425,-123.127266802597,
176.356991379871));
#40741=CARTESIAN_POINT('Ctrl Pts',(-63.2391153236096,-123.204176050311,
175.123916881932));
#40742=CARTESIAN_POINT('Ctrl Pts',(-62.4902494419682,-123.378291384946,
174.143189863554));
#40743=CARTESIAN_POINT('Ctrl Pts',(-61.7413835603268,-123.55240671958,173.162462845176));
#40744=CARTESIAN_POINT('Ctrl Pts',(-60.5251948963169,-123.776341784949,
173.008579892738));
#40745=CARTESIAN_POINT('Ctrl Pts',(-59.3090062323071,-124.000276850317,
172.854696940301));
#40746=CARTESIAN_POINT('Ctrl Pts',(-58.3437431933744,-124.197461567645,
173.617800600325));
#40747=CARTESIAN_POINT('Ctrl Pts',(-57.3784801544418,-124.394646284973,
174.380904260348));
#40748=CARTESIAN_POINT('Ctrl Pts',(-57.2354023200087,-124.504180566569,
175.613978758287));
#40749=CARTESIAN_POINT('Ctrl Pts',(-57.0923244855756,-124.613714848165,
176.847053256227));
#40750=CARTESIAN_POINT('Ctrl Pts',(-57.861066493051,-124.626043042842,177.827780274605));
#40751=CARTESIAN_POINT('Ctrl Pts',(-58.6298085005265,-124.638371237518,
178.808507292983));
#40752=CARTESIAN_POINT('Ctrl Pts',(-59.8658732903704,-124.60087970146,178.96239024542));
#40753=CARTESIAN_POINT('Ctrl Pts',(-61.1019380802142,-124.563388165402,
179.116273197858));
#40754=CARTESIAN_POINT('Ctrl Pts',(-62.0870772449809,-124.552646977385,
178.353169537834));
#40755=CARTESIAN_POINT('Ctrl Pts',(-63.0722164097476,-124.541905789367,
177.590065877811));
#40756=CARTESIAN_POINT('Ctrl Pts',(-63.2351703700147,-124.618815037082,
176.356991379871));
#40757=CARTESIAN_POINT('Ctrl Pts',(-63.3981243302818,-124.695724284797,
175.123916881932));
#40758=CARTESIAN_POINT('Ctrl Pts',(-62.6492584486404,-124.869839619431,
174.143189863554));
#40759=CARTESIAN_POINT('Ctrl Pts',(-61.900392566999,-125.043954954065,173.162462845176));
#40760=CARTESIAN_POINT('Ctrl Pts',(-60.6842039029891,-125.267890019434,
173.008579892738));
#40761=CARTESIAN_POINT('Ctrl Pts',(-59.4680152389793,-125.491825084803,
172.854696940301));
#40762=CARTESIAN_POINT('Ctrl Pts',(-58.5027522000467,-125.689009802131,
173.617800600325));
#40763=CARTESIAN_POINT('Ctrl Pts',(-57.537489161114,-125.886194519459,174.380904260348));
#40764=CARTESIAN_POINT('Ctrl Pts',(-57.3944113266809,-125.995728801055,
175.613978758287));
#40765=CARTESIAN_POINT('Ctrl Pts',(-57.2513334922478,-126.105263082651,
176.847053256227));
#40766=CARTESIAN_POINT('Ctrl Pts',(-58.0200754997233,-126.117591277327,
177.827780274605));
#40767=CARTESIAN_POINT('Ctrl Pts',(-58.7888175071987,-126.129919472004,
178.808507292983));
#40768=CARTESIAN_POINT('Ctrl Pts',(-60.0248822970426,-126.092427935946,
178.96239024542));
#40769=CARTESIAN_POINT('Ctrl Pts',(-61.2609470868864,-126.054936399888,
179.116273197858));
#40770=CARTESIAN_POINT('Ctrl Pts',(-62.2460862516531,-126.04419521187,178.353169537834));
#40771=CARTESIAN_POINT('Ctrl Pts',(-63.2312254164198,-126.033454023853,
177.590065877811));
#40772=CARTESIAN_POINT('Ctrl Pts',(-63.3941793766869,-126.110363271568,
176.356991379871));
#40773=CARTESIAN_POINT('Ctrl Pts',(-63.5571333369541,-126.187272519283,
175.123916881932));
#40774=CARTESIAN_POINT('Ctrl Pts',(-62.8082674553126,-126.361387853917,
174.143189863554));
#40775=CARTESIAN_POINT('Ctrl Pts',(-62.0594015736712,-126.535503188551,
173.162462845176));
#40776=CARTESIAN_POINT('Ctrl Pts',(-60.8432129096614,-126.75943825392,173.008579892738));
#40777=CARTESIAN_POINT('Ctrl Pts',(-59.6270242456515,-126.983373319289,
172.854696940301));
#40778=CARTESIAN_POINT('Ctrl Pts',(-58.6617612067189,-127.180558036617,
173.617800600325));
#40779=CARTESIAN_POINT('Ctrl Pts',(-57.6964981677863,-127.377742753945,
174.380904260348));
#40780=CARTESIAN_POINT('Ctrl Pts',(-57.5534203333531,-127.487277035541,
175.613978758287));
#40781=CARTESIAN_POINT('Ctrl Pts',(-57.41034249892,-127.596811317136,176.847053256227));
#40782=CARTESIAN_POINT('Ctrl Pts',(-58.1790845063955,-127.609139511813,
177.827780274605));
#40783=CARTESIAN_POINT('Ctrl Pts',(-58.947826513871,-127.621467706489,178.808507292983));
#40784=CARTESIAN_POINT('Ctrl Pts',(-60.1838913037148,-127.583976170431,
178.96239024542));
#40785=CARTESIAN_POINT('Ctrl Pts',(-61.4199560935587,-127.546484634373,
179.116273197858));
#40786=CARTESIAN_POINT('Ctrl Pts',(-62.4050952583254,-127.535743446356,
178.353169537834));
#40787=CARTESIAN_POINT('Ctrl Pts',(-63.390234423092,-127.525002258339,177.590065877811));
#40788=CARTESIAN_POINT('Ctrl Pts',(-63.5531883833591,-127.601911506053,
176.356991379871));
#40789=CARTESIAN_POINT('Ctrl Pts',(-63.7161423436263,-127.678820753768,
175.123916881932));
#40790=CARTESIAN_POINT('Ctrl Pts',(-62.9672764619849,-127.852936088402,
174.143189863554));
#40791=CARTESIAN_POINT('Ctrl Pts',(-62.2184105803435,-128.027051423037,
173.162462845176));
#40792=CARTESIAN_POINT('Ctrl Pts',(-61.0022219163336,-128.250986488405,
173.008579892738));
#40793=CARTESIAN_POINT('Ctrl Pts',(-59.7860332523238,-128.474921553774,
172.854696940301));
#40794=CARTESIAN_POINT('Ctrl Pts',(-58.8207702133911,-128.672106271102,
173.617800600325));
#40795=CARTESIAN_POINT('Ctrl Pts',(-57.8555071744585,-128.86929098843,174.380904260348));
#40796=CARTESIAN_POINT('Ctrl Pts',(-57.7124293400254,-128.978825270026,
175.613978758287));
#40797=CARTESIAN_POINT('Ctrl Pts',(-57.5693515055923,-129.088359551622,
176.847053256227));
#40798=CARTESIAN_POINT('Ctrl Pts',(-58.3380935130677,-129.100687746298,
177.827780274605));
#40799=CARTESIAN_POINT('Ctrl Pts',(-59.1068355205432,-129.113015940975,
178.808507292983));
#40800=CARTESIAN_POINT('Ctrl Pts',(-60.342900310387,-129.075524404917,178.96239024542));
#40801=CARTESIAN_POINT('Ctrl Pts',(-61.5789651002309,-129.038032868859,
179.116273197858));
#40802=CARTESIAN_POINT('Ctrl Pts',(-62.5641042649976,-129.027291680842,
178.353169537834));
#40803=CARTESIAN_POINT('Ctrl Pts',(-63.5492434297643,-129.016550492824,
177.590065877811));
#40804=CARTESIAN_POINT('Ctrl Pts',(-63.7121973900314,-129.093459740539,
176.356991379871));
#40805=CARTESIAN_POINT('Ctrl Pts',(-63.8751513502985,-129.170368988254,
175.123916881932));
#40806=CARTESIAN_POINT('Ctrl Pts',(-63.1262854686571,-129.344484322888,
174.143189863554));
#40807=CARTESIAN_POINT('Ctrl Pts',(-62.3774195870157,-129.518599657522,
173.162462845176));
#40808=CARTESIAN_POINT('Ctrl Pts',(-61.1612309230058,-129.742534722891,
173.008579892738));
#40809=CARTESIAN_POINT('Ctrl Pts',(-59.945042258996,-129.96646978826,172.854696940301));
#40810=CARTESIAN_POINT('Ctrl Pts',(-58.9797792200633,-130.163654505588,
173.617800600325));
#40811=CARTESIAN_POINT('Ctrl Pts',(-58.0145161811307,-130.360839222916,
174.380904260348));
#40812=CARTESIAN_POINT('Ctrl Pts',(-57.8714383466976,-130.470373504512,
175.613978758287));
#40813=CARTESIAN_POINT('Ctrl Pts',(-57.7283605122645,-130.579907786108,
176.847053256227));
#40814=CARTESIAN_POINT('Ctrl Pts',(-58.4971025197399,-130.592235980784,
177.827780274605));
#40815=CARTESIAN_POINT('Ctrl Pts',(-59.2658445272154,-130.604564175461,
178.808507292983));
#40816=CARTESIAN_POINT('Ctrl Pts',(-60.5019093170593,-130.567072639403,
178.96239024542));
#40817=CARTESIAN_POINT('Ctrl Pts',(-61.7379741069031,-130.529581103344,
179.116273197858));
#40818=CARTESIAN_POINT('Ctrl Pts',(-62.7231132716698,-130.518839915327,
178.353169537834));
#40819=CARTESIAN_POINT('Ctrl Pts',(-63.7082524364365,-130.50809872731,177.590065877811));
#40820=CARTESIAN_POINT('Ctrl Pts',(-63.8712063967036,-130.585007975025,
176.356991379871));
#40821=CARTESIAN_POINT('Ctrl Pts',(-64.0341603569708,-130.661917222739,
175.123916881932));
#40822=CARTESIAN_POINT('Ctrl Pts',(-63.2852944753293,-130.836032557374,
174.143189863554));
#40823=CARTESIAN_POINT('Ctrl Pts',(-62.5364285936879,-131.010147892008,
173.162462845176));
#40824=CARTESIAN_POINT('Ctrl Pts',(-61.3202399296781,-131.234082957377,
173.008579892738));
#40825=CARTESIAN_POINT('Ctrl Pts',(-60.1040512656682,-131.458018022745,
172.854696940301));
#40826=CARTESIAN_POINT('Ctrl Pts',(-59.1387882267356,-131.655202740073,
173.617800600325));
#40827=CARTESIAN_POINT('Ctrl Pts',(-58.1735251878029,-131.852387457401,
174.380904260348));
#40828=CARTESIAN_POINT('Ctrl Pts',(-58.0304473533698,-131.961921738997,
175.613978758287));
#40829=CARTESIAN_POINT('Ctrl Pts',(-57.8873695189367,-132.071456020593,
176.847053256227));
#40830=CARTESIAN_POINT('Ctrl Pts',(-58.6561115264122,-132.08378421527,177.827780274605));
#40831=CARTESIAN_POINT('Ctrl Pts',(-59.4248535338876,-132.096112409946,
178.808507292983));
#40832=CARTESIAN_POINT('Ctrl Pts',(-60.6609183237315,-132.058620873888,
178.96239024542));
#40833=CARTESIAN_POINT('Ctrl Pts',(-61.4604944724631,-132.034368635448,
179.061932874153));
#40834=CARTESIAN_POINT('Ctrl Pts',(-62.203773450631,-132.020578326074,178.749326549433));
#40835=CARTESIAN_POINT('Ctrl Pts',(-52.6515183282542,-67.7327195975386,
179.686725372378));
#40836=CARTESIAN_POINT('Ctrl Pts',(-53.1450794947509,-67.7126445084354,
179.888729463648));
#40837=CARTESIAN_POINT('Ctrl Pts',(-53.673891258688,-67.6865820008601,179.954696079469));
#40838=CARTESIAN_POINT('Ctrl Pts',(-55.3186666497572,-67.6055191841591,
180.159873561769));
#40839=CARTESIAN_POINT('Ctrl Pts',(-56.6288741944062,-67.5601235350989,
179.142400961866));
#40840=CARTESIAN_POINT('Ctrl Pts',(-57.9390817390552,-67.5147278860387,
178.124928361964));
#40841=CARTESIAN_POINT('Ctrl Pts',(-58.1530412096253,-67.5861996055927,
176.48082732954));
#40842=CARTESIAN_POINT('Ctrl Pts',(-58.3670006801954,-67.6576713251468,
174.836726297116));
#40843=CARTESIAN_POINT('Ctrl Pts',(-57.3651991030978,-67.8587512947533,
173.529088919052));
#40844=CARTESIAN_POINT('Ctrl Pts',(-56.3633975260002,-68.0598312643598,
172.221451540989));
#40845=CARTESIAN_POINT('Ctrl Pts',(-54.7384982607651,-68.3273376103715,
172.016274058689));
#40846=CARTESIAN_POINT('Ctrl Pts',(-53.1135989955299,-68.5948439563832,
171.81109657639));
#40847=CARTESIAN_POINT('Ctrl Pts',(-51.8232675767149,-68.8266831347541,
172.828569176292));
#40848=CARTESIAN_POINT('Ctrl Pts',(-50.5329361578999,-69.0585223131251,
173.846041776195));
#40849=CARTESIAN_POINT('Ctrl Pts',(-50.3388528131639,-69.1734941228817,
175.490142808619));
#40850=CARTESIAN_POINT('Ctrl Pts',(-50.1447694684278,-69.2884659326383,
177.134243841043));
#40851=CARTESIAN_POINT('Ctrl Pts',(-51.1664471713594,-69.2738294923425,
178.441881219107));
#40852=CARTESIAN_POINT('Ctrl Pts',(-52.188124874291,-69.2591930520467,179.74951859717));
#40853=CARTESIAN_POINT('Ctrl Pts',(-53.8329002653602,-69.1781302353457,
179.954696079469));
#40854=CARTESIAN_POINT('Ctrl Pts',(-55.4776756564294,-69.0970674186447,
180.159873561769));
#40855=CARTESIAN_POINT('Ctrl Pts',(-56.7878832010784,-69.0516717695845,
179.142400961866));
#40856=CARTESIAN_POINT('Ctrl Pts',(-58.0980907457274,-69.0062761205243,
178.124928361964));
#40857=CARTESIAN_POINT('Ctrl Pts',(-58.3120502162975,-69.0777478400783,
176.48082732954));
#40858=CARTESIAN_POINT('Ctrl Pts',(-58.5260096868676,-69.1492195596324,
174.836726297116));
#40859=CARTESIAN_POINT('Ctrl Pts',(-57.52420810977,-69.3502995292389,173.529088919052));
#40860=CARTESIAN_POINT('Ctrl Pts',(-56.5224065326725,-69.5513794988454,
172.221451540989));
#40861=CARTESIAN_POINT('Ctrl Pts',(-54.8975072674373,-69.8188858448571,
172.016274058689));
#40862=CARTESIAN_POINT('Ctrl Pts',(-53.2726080022022,-70.0863921908688,
171.81109657639));
#40863=CARTESIAN_POINT('Ctrl Pts',(-51.9822765833872,-70.3182313692397,
172.828569176292));
#40864=CARTESIAN_POINT('Ctrl Pts',(-50.6919451645722,-70.5500705476106,
173.846041776195));
#40865=CARTESIAN_POINT('Ctrl Pts',(-50.4978618198361,-70.6650423573673,
175.490142808619));
#40866=CARTESIAN_POINT('Ctrl Pts',(-50.3037784751,-70.7800141671239,177.134243841043));
#40867=CARTESIAN_POINT('Ctrl Pts',(-51.3254561780316,-70.7653777268281,
178.441881219107));
#40868=CARTESIAN_POINT('Ctrl Pts',(-52.3471338809632,-70.7507412865323,
179.74951859717));
#40869=CARTESIAN_POINT('Ctrl Pts',(-53.9919092720324,-70.6696784698313,
179.954696079469));
#40870=CARTESIAN_POINT('Ctrl Pts',(-55.6366846631016,-70.5886156531303,
180.159873561769));
#40871=CARTESIAN_POINT('Ctrl Pts',(-56.9468922077507,-70.5432200040701,
179.142400961866));
#40872=CARTESIAN_POINT('Ctrl Pts',(-58.2570997523997,-70.4978243550099,
178.124928361964));
#40873=CARTESIAN_POINT('Ctrl Pts',(-58.4710592229698,-70.5692960745639,
176.48082732954));
#40874=CARTESIAN_POINT('Ctrl Pts',(-58.6850186935399,-70.640767794118,174.836726297116));
#40875=CARTESIAN_POINT('Ctrl Pts',(-57.6832171164423,-70.8418477637245,
173.529088919052));
#40876=CARTESIAN_POINT('Ctrl Pts',(-56.6814155393447,-71.042927733331,172.221451540989));
#40877=CARTESIAN_POINT('Ctrl Pts',(-55.0565162741095,-71.3104340793427,
172.016274058689));
#40878=CARTESIAN_POINT('Ctrl Pts',(-53.4316170088744,-71.5779404253544,
171.81109657639));
#40879=CARTESIAN_POINT('Ctrl Pts',(-52.1412855900594,-71.8097796037253,
172.828569176292));
#40880=CARTESIAN_POINT('Ctrl Pts',(-50.8509541712444,-72.0416187820962,
173.846041776195));
#40881=CARTESIAN_POINT('Ctrl Pts',(-50.6568708265083,-72.1565905918529,
175.490142808619));
#40882=CARTESIAN_POINT('Ctrl Pts',(-50.4627874817723,-72.2715624016095,
177.134243841043));
#40883=CARTESIAN_POINT('Ctrl Pts',(-51.4844651847039,-72.2569259613137,
178.441881219107));
#40884=CARTESIAN_POINT('Ctrl Pts',(-52.5061428876355,-72.242289521018,179.74951859717));
#40885=CARTESIAN_POINT('Ctrl Pts',(-54.1509182787047,-72.1612267043169,
179.954696079469));
#40886=CARTESIAN_POINT('Ctrl Pts',(-55.7956936697739,-72.0801638876159,
180.159873561769));
#40887=CARTESIAN_POINT('Ctrl Pts',(-57.1059012144229,-72.0347682385557,
179.142400961866));
#40888=CARTESIAN_POINT('Ctrl Pts',(-58.4161087590719,-71.9893725894955,
178.124928361964));
#40889=CARTESIAN_POINT('Ctrl Pts',(-58.630068229642,-72.0608443090495,176.48082732954));
#40890=CARTESIAN_POINT('Ctrl Pts',(-58.8440277002121,-72.1323160286036,
174.836726297116));
#40891=CARTESIAN_POINT('Ctrl Pts',(-57.8422261231145,-72.3333959982101,
173.529088919052));
#40892=CARTESIAN_POINT('Ctrl Pts',(-56.8404245460169,-72.5344759678166,
172.221451540989));
#40893=CARTESIAN_POINT('Ctrl Pts',(-55.2155252807818,-72.8019823138283,
172.016274058689));
#40894=CARTESIAN_POINT('Ctrl Pts',(-53.5906260155466,-73.06948865984,171.81109657639));
#40895=CARTESIAN_POINT('Ctrl Pts',(-52.3002945967316,-73.3013278382109,
172.828569176292));
#40896=CARTESIAN_POINT('Ctrl Pts',(-51.0099631779166,-73.5331670165818,
173.846041776195));
#40897=CARTESIAN_POINT('Ctrl Pts',(-50.8158798331806,-73.6481388263385,
175.490142808619));
#40898=CARTESIAN_POINT('Ctrl Pts',(-50.6217964884445,-73.7631106360951,
177.134243841043));
#40899=CARTESIAN_POINT('Ctrl Pts',(-51.6434741913761,-73.7484741957993,
178.441881219107));
#40900=CARTESIAN_POINT('Ctrl Pts',(-52.6651518943077,-73.7338377555035,
179.74951859717));
#40901=CARTESIAN_POINT('Ctrl Pts',(-54.3099272853769,-73.6527749388025,
179.954696079469));
#40902=CARTESIAN_POINT('Ctrl Pts',(-55.9547026764461,-73.5717121221015,
180.159873561769));
#40903=CARTESIAN_POINT('Ctrl Pts',(-57.2649102210951,-73.5263164730413,
179.142400961866));
#40904=CARTESIAN_POINT('Ctrl Pts',(-58.5751177657441,-73.4809208239811,
178.124928361964));
#40905=CARTESIAN_POINT('Ctrl Pts',(-58.7890772363142,-73.5523925435351,
176.48082732954));
#40906=CARTESIAN_POINT('Ctrl Pts',(-59.0030367068843,-73.6238642630892,
174.836726297116));
#40907=CARTESIAN_POINT('Ctrl Pts',(-58.0012351297867,-73.8249442326957,
173.529088919052));
#40908=CARTESIAN_POINT('Ctrl Pts',(-56.9994335526892,-74.0260242023022,
172.221451540989));
#40909=CARTESIAN_POINT('Ctrl Pts',(-55.374534287454,-74.2935305483139,172.016274058689));
#40910=CARTESIAN_POINT('Ctrl Pts',(-53.7496350222188,-74.5610368943256,
171.81109657639));
#40911=CARTESIAN_POINT('Ctrl Pts',(-52.4593036034038,-74.7928760726965,
172.828569176292));
#40912=CARTESIAN_POINT('Ctrl Pts',(-51.1689721845888,-75.0247152510674,
173.846041776195));
#40913=CARTESIAN_POINT('Ctrl Pts',(-50.9748888398528,-75.1396870608241,
175.490142808619));
#40914=CARTESIAN_POINT('Ctrl Pts',(-50.7808054951167,-75.2546588705807,
177.134243841043));
#40915=CARTESIAN_POINT('Ctrl Pts',(-51.8024831980483,-75.2400224302849,
178.441881219107));
#40916=CARTESIAN_POINT('Ctrl Pts',(-52.8241609009799,-75.2253859899891,
179.74951859717));
#40917=CARTESIAN_POINT('Ctrl Pts',(-54.4689362920491,-75.1443231732881,
179.954696079469));
#40918=CARTESIAN_POINT('Ctrl Pts',(-56.1137116831183,-75.0632603565871,
180.159873561769));
#40919=CARTESIAN_POINT('Ctrl Pts',(-57.4239192277673,-75.0178647075269,
179.142400961866));
#40920=CARTESIAN_POINT('Ctrl Pts',(-58.7341267724164,-74.9724690584667,
178.124928361964));
#40921=CARTESIAN_POINT('Ctrl Pts',(-58.9480862429864,-75.0439407780207,
176.48082732954));
#40922=CARTESIAN_POINT('Ctrl Pts',(-59.1620457135565,-75.1154124975748,
174.836726297116));
#40923=CARTESIAN_POINT('Ctrl Pts',(-58.1602441364589,-75.3164924671813,
173.529088919052));
#40924=CARTESIAN_POINT('Ctrl Pts',(-57.1584425593614,-75.5175724367878,
172.221451540989));
#40925=CARTESIAN_POINT('Ctrl Pts',(-55.5335432941262,-75.7850787827995,
172.016274058689));
#40926=CARTESIAN_POINT('Ctrl Pts',(-53.9086440288911,-76.0525851288112,
171.81109657639));
#40927=CARTESIAN_POINT('Ctrl Pts',(-52.6183126100761,-76.2844243071821,
172.828569176292));
#40928=CARTESIAN_POINT('Ctrl Pts',(-51.3279811912611,-76.5162634855531,
173.846041776195));
#40929=CARTESIAN_POINT('Ctrl Pts',(-51.133897846525,-76.6312352953097,175.490142808619));
#40930=CARTESIAN_POINT('Ctrl Pts',(-50.939814501789,-76.7462071050663,177.134243841043));
#40931=CARTESIAN_POINT('Ctrl Pts',(-51.9614922047205,-76.7315706647705,
178.441881219107));
#40932=CARTESIAN_POINT('Ctrl Pts',(-52.9831699076522,-76.7169342244747,
179.74951859717));
#40933=CARTESIAN_POINT('Ctrl Pts',(-54.6279452987213,-76.6358714077737,
179.954696079469));
#40934=CARTESIAN_POINT('Ctrl Pts',(-56.2727206897905,-76.5548085910727,
180.159873561769));
#40935=CARTESIAN_POINT('Ctrl Pts',(-57.5829282344396,-76.5094129420125,
179.142400961866));
#40936=CARTESIAN_POINT('Ctrl Pts',(-58.8931357790886,-76.4640172929522,
178.124928361964));
#40937=CARTESIAN_POINT('Ctrl Pts',(-59.1070952496587,-76.5354890125063,
176.48082732954));
#40938=CARTESIAN_POINT('Ctrl Pts',(-59.3210547202288,-76.6069607320604,
174.836726297116));
#40939=CARTESIAN_POINT('Ctrl Pts',(-58.3192531431312,-76.8080407016669,
173.529088919052));
#40940=CARTESIAN_POINT('Ctrl Pts',(-57.3174515660336,-77.0091206712734,
172.221451540989));
#40941=CARTESIAN_POINT('Ctrl Pts',(-55.6925523007984,-77.2766270172851,
172.016274058689));
#40942=CARTESIAN_POINT('Ctrl Pts',(-54.0676530355633,-77.5441333632968,
171.81109657639));
#40943=CARTESIAN_POINT('Ctrl Pts',(-52.7773216167483,-77.7759725416677,
172.828569176292));
#40944=CARTESIAN_POINT('Ctrl Pts',(-51.4869901979333,-78.0078117200386,
173.846041776195));
#40945=CARTESIAN_POINT('Ctrl Pts',(-51.2929068531972,-78.1227835297953,
175.490142808619));
#40946=CARTESIAN_POINT('Ctrl Pts',(-51.0988235084612,-78.2377553395519,
177.134243841043));
#40947=CARTESIAN_POINT('Ctrl Pts',(-52.1205012113928,-78.2231188992561,
178.441881219107));
#40948=CARTESIAN_POINT('Ctrl Pts',(-53.1421789143244,-78.2084824589603,
179.74951859717));
#40949=CARTESIAN_POINT('Ctrl Pts',(-54.7869543053936,-78.1274196422593,
179.954696079469));
#40950=CARTESIAN_POINT('Ctrl Pts',(-56.4317296964628,-78.0463568255583,
180.159873561769));
#40951=CARTESIAN_POINT('Ctrl Pts',(-57.7419372411118,-78.0009611764981,
179.142400961866));
#40952=CARTESIAN_POINT('Ctrl Pts',(-59.0521447857608,-77.9555655274379,
178.124928361964));
#40953=CARTESIAN_POINT('Ctrl Pts',(-59.2661042563309,-78.0270372469919,
176.48082732954));
#40954=CARTESIAN_POINT('Ctrl Pts',(-59.480063726901,-78.098508966546,174.836726297116));
#40955=CARTESIAN_POINT('Ctrl Pts',(-58.4782621498034,-78.2995889361525,
173.529088919052));
#40956=CARTESIAN_POINT('Ctrl Pts',(-57.4764605727058,-78.500668905759,172.221451540989));
#40957=CARTESIAN_POINT('Ctrl Pts',(-55.8515613074707,-78.7681752517707,
172.016274058689));
#40958=CARTESIAN_POINT('Ctrl Pts',(-54.2266620422355,-79.0356815977824,
171.81109657639));
#40959=CARTESIAN_POINT('Ctrl Pts',(-52.9363306234205,-79.2675207761533,
172.828569176292));
#40960=CARTESIAN_POINT('Ctrl Pts',(-51.6459992046055,-79.4993599545243,
173.846041776195));
#40961=CARTESIAN_POINT('Ctrl Pts',(-51.4519158598695,-79.6143317642809,
175.490142808619));
#40962=CARTESIAN_POINT('Ctrl Pts',(-51.2578325151334,-79.7293035740375,
177.134243841043));
#40963=CARTESIAN_POINT('Ctrl Pts',(-52.279510218065,-79.7146671337417,178.441881219107));
#40964=CARTESIAN_POINT('Ctrl Pts',(-53.3011879209966,-79.7000306934459,
179.74951859717));
#40965=CARTESIAN_POINT('Ctrl Pts',(-54.9459633120658,-79.6189678767449,
179.954696079469));
#40966=CARTESIAN_POINT('Ctrl Pts',(-56.590738703135,-79.5379050600439,180.159873561769));
#40967=CARTESIAN_POINT('Ctrl Pts',(-57.900946247784,-79.4925094109837,179.142400961866));
#40968=CARTESIAN_POINT('Ctrl Pts',(-59.211153792433,-79.4471137619235,178.124928361964));
#40969=CARTESIAN_POINT('Ctrl Pts',(-59.4251132630031,-79.5185854814775,
176.48082732954));
#40970=CARTESIAN_POINT('Ctrl Pts',(-59.6390727335732,-79.5900572010316,
174.836726297116));
#40971=CARTESIAN_POINT('Ctrl Pts',(-58.6372711564756,-79.7911371706381,
173.529088919052));
#40972=CARTESIAN_POINT('Ctrl Pts',(-57.6354695793781,-79.9922171402446,
172.221451540989));
#40973=CARTESIAN_POINT('Ctrl Pts',(-56.0105703141429,-80.2597234862563,
172.016274058689));
#40974=CARTESIAN_POINT('Ctrl Pts',(-54.3856710489078,-80.527229832268,171.81109657639));
#40975=CARTESIAN_POINT('Ctrl Pts',(-53.0953396300927,-80.7590690106389,
172.828569176292));
#40976=CARTESIAN_POINT('Ctrl Pts',(-51.8050082112778,-80.9909081890099,
173.846041776195));
#40977=CARTESIAN_POINT('Ctrl Pts',(-51.6109248665417,-81.1058799987665,
175.490142808619));
#40978=CARTESIAN_POINT('Ctrl Pts',(-51.4168415218056,-81.2208518085231,
177.134243841043));
#40979=CARTESIAN_POINT('Ctrl Pts',(-52.4385192247372,-81.2062153682273,
178.441881219107));
#40980=CARTESIAN_POINT('Ctrl Pts',(-53.4601969276688,-81.1915789279315,
179.74951859717));
#40981=CARTESIAN_POINT('Ctrl Pts',(-55.104972318738,-81.1105161112305,179.954696079469));
#40982=CARTESIAN_POINT('Ctrl Pts',(-56.7497477098072,-81.0294532945295,
180.159873561769));
#40983=CARTESIAN_POINT('Ctrl Pts',(-58.0599552544562,-80.9840576454693,
179.142400961866));
#40984=CARTESIAN_POINT('Ctrl Pts',(-59.3701627991053,-80.9386619964091,
178.124928361964));
#40985=CARTESIAN_POINT('Ctrl Pts',(-59.5841222696753,-81.0101337159631,
176.48082732954));
#40986=CARTESIAN_POINT('Ctrl Pts',(-59.7980817402454,-81.0816054355172,
174.836726297116));
#40987=CARTESIAN_POINT('Ctrl Pts',(-58.7962801631479,-81.2826854051237,
173.529088919052));
#40988=CARTESIAN_POINT('Ctrl Pts',(-57.7944785860503,-81.4837653747302,
172.221451540989));
#40989=CARTESIAN_POINT('Ctrl Pts',(-56.1695793208151,-81.7512717207419,
172.016274058689));
#40990=CARTESIAN_POINT('Ctrl Pts',(-54.54468005558,-82.0187780667536,171.81109657639));
#40991=CARTESIAN_POINT('Ctrl Pts',(-53.254348636765,-82.2506172451245,172.828569176292));
#40992=CARTESIAN_POINT('Ctrl Pts',(-51.96401721795,-82.4824564234954,173.846041776195));
#40993=CARTESIAN_POINT('Ctrl Pts',(-51.7699338732139,-82.5974282332521,
175.490142808619));
#40994=CARTESIAN_POINT('Ctrl Pts',(-51.5758505284779,-82.7124000430087,
177.134243841043));
#40995=CARTESIAN_POINT('Ctrl Pts',(-52.5975282314095,-82.6977636027129,
178.441881219107));
#40996=CARTESIAN_POINT('Ctrl Pts',(-53.6192059343411,-82.6831271624172,
179.74951859717));
#40997=CARTESIAN_POINT('Ctrl Pts',(-55.2639813254103,-82.6020643457161,
179.954696079469));
#40998=CARTESIAN_POINT('Ctrl Pts',(-56.9087567164794,-82.5210015290151,
180.159873561769));
#40999=CARTESIAN_POINT('Ctrl Pts',(-58.2189642611285,-82.4756058799549,
179.142400961866));
#41000=CARTESIAN_POINT('Ctrl Pts',(-59.5291718057775,-82.4302102308947,
178.124928361964));
#41001=CARTESIAN_POINT('Ctrl Pts',(-59.7431312763476,-82.5016819504488,
176.48082732954));
#41002=CARTESIAN_POINT('Ctrl Pts',(-59.9570907469177,-82.5731536700028,
174.836726297116));
#41003=CARTESIAN_POINT('Ctrl Pts',(-58.9552891698201,-82.7742336396093,
173.529088919052));
#41004=CARTESIAN_POINT('Ctrl Pts',(-57.9534875927225,-82.9753136092158,
172.221451540989));
#41005=CARTESIAN_POINT('Ctrl Pts',(-56.3285883274873,-83.2428199552275,
172.016274058689));
#41006=CARTESIAN_POINT('Ctrl Pts',(-54.7036890622522,-83.5103263012392,
171.81109657639));
#41007=CARTESIAN_POINT('Ctrl Pts',(-53.4133576434372,-83.7421654796101,
172.828569176292));
#41008=CARTESIAN_POINT('Ctrl Pts',(-52.1230262246222,-83.9740046579811,
173.846041776195));
#41009=CARTESIAN_POINT('Ctrl Pts',(-51.9289428798862,-84.0889764677377,
175.490142808619));
#41010=CARTESIAN_POINT('Ctrl Pts',(-51.7348595351501,-84.2039482774943,
177.134243841043));
#41011=CARTESIAN_POINT('Ctrl Pts',(-52.7565372380817,-84.1893118371985,
178.441881219107));
#41012=CARTESIAN_POINT('Ctrl Pts',(-53.7782149410133,-84.1746753969028,
179.74951859717));
#41013=CARTESIAN_POINT('Ctrl Pts',(-55.4229903320825,-84.0936125802018,
179.954696079469));
#41014=CARTESIAN_POINT('Ctrl Pts',(-57.0677657231517,-84.0125497635007,
180.159873561769));
#41015=CARTESIAN_POINT('Ctrl Pts',(-58.3779732678007,-83.9671541144405,
179.142400961866));
#41016=CARTESIAN_POINT('Ctrl Pts',(-59.6881808124497,-83.9217584653803,
178.124928361964));
#41017=CARTESIAN_POINT('Ctrl Pts',(-59.9021402830198,-83.9932301849343,
176.48082732954));
#41018=CARTESIAN_POINT('Ctrl Pts',(-60.1160997535899,-84.0647019044884,
174.836726297116));
#41019=CARTESIAN_POINT('Ctrl Pts',(-59.1142981764923,-84.2657818740949,
173.529088919052));
#41020=CARTESIAN_POINT('Ctrl Pts',(-58.1124965993947,-84.4668618437014,
172.221451540989));
#41021=CARTESIAN_POINT('Ctrl Pts',(-56.4875973341596,-84.7343681897131,
172.016274058689));
#41022=CARTESIAN_POINT('Ctrl Pts',(-54.8626980689244,-85.0018745357248,
171.81109657639));
#41023=CARTESIAN_POINT('Ctrl Pts',(-53.5723666501094,-85.2337137140957,
172.828569176292));
#41024=CARTESIAN_POINT('Ctrl Pts',(-52.2820352312944,-85.4655528924667,
173.846041776195));
#41025=CARTESIAN_POINT('Ctrl Pts',(-52.0879518865584,-85.5805247022233,
175.490142808619));
#41026=CARTESIAN_POINT('Ctrl Pts',(-51.8938685418223,-85.6954965119799,
177.134243841043));
#41027=CARTESIAN_POINT('Ctrl Pts',(-52.9155462447539,-85.6808600716841,
178.441881219107));
#41028=CARTESIAN_POINT('Ctrl Pts',(-53.9372239476855,-85.6662236313884,
179.74951859717));
#41029=CARTESIAN_POINT('Ctrl Pts',(-55.5819993387547,-85.5851608146873,
179.954696079469));
#41030=CARTESIAN_POINT('Ctrl Pts',(-57.2267747298239,-85.5040979979863,
180.159873561769));
#41031=CARTESIAN_POINT('Ctrl Pts',(-58.5369822744729,-85.4587023489261,
179.142400961866));
#41032=CARTESIAN_POINT('Ctrl Pts',(-59.847189819122,-85.4133066998659,178.124928361964));
#41033=CARTESIAN_POINT('Ctrl Pts',(-60.061149289692,-85.4847784194199,176.48082732954));
#41034=CARTESIAN_POINT('Ctrl Pts',(-60.2751087602621,-85.556250138974,174.836726297116));
#41035=CARTESIAN_POINT('Ctrl Pts',(-59.2733071831645,-85.7573301085805,
173.529088919052));
#41036=CARTESIAN_POINT('Ctrl Pts',(-58.271505606067,-85.958410078187,172.221451540989));
#41037=CARTESIAN_POINT('Ctrl Pts',(-56.6466063408318,-86.2259164241987,
172.016274058689));
#41038=CARTESIAN_POINT('Ctrl Pts',(-55.0217070755966,-86.4934227702104,
171.81109657639));
#41039=CARTESIAN_POINT('Ctrl Pts',(-53.7313756567816,-86.7252619485813,
172.828569176292));
#41040=CARTESIAN_POINT('Ctrl Pts',(-52.4410442379667,-86.9571011269523,
173.846041776195));
#41041=CARTESIAN_POINT('Ctrl Pts',(-52.2469608932306,-87.0720729367089,
175.490142808619));
#41042=CARTESIAN_POINT('Ctrl Pts',(-52.0528775484945,-87.1870447464655,
177.134243841043));
#41043=CARTESIAN_POINT('Ctrl Pts',(-53.0745552514261,-87.1724083061697,
178.441881219107));
#41044=CARTESIAN_POINT('Ctrl Pts',(-54.0962329543578,-87.157771865874,179.74951859717));
#41045=CARTESIAN_POINT('Ctrl Pts',(-55.7410083454269,-87.0767090491729,
179.954696079469));
#41046=CARTESIAN_POINT('Ctrl Pts',(-57.3857837364961,-86.9956462324719,
180.159873561769));
#41047=CARTESIAN_POINT('Ctrl Pts',(-58.6959912811452,-86.9502505834117,
179.142400961866));
#41048=CARTESIAN_POINT('Ctrl Pts',(-60.0061988257942,-86.9048549343515,
178.124928361964));
#41049=CARTESIAN_POINT('Ctrl Pts',(-60.2201582963643,-86.9763266539055,
176.48082732954));
#41050=CARTESIAN_POINT('Ctrl Pts',(-60.4341177669343,-87.0477983734596,
174.836726297116));
#41051=CARTESIAN_POINT('Ctrl Pts',(-59.4323161898368,-87.2488783430661,
173.529088919052));
#41052=CARTESIAN_POINT('Ctrl Pts',(-58.4305146127392,-87.4499583126726,
172.221451540989));
#41053=CARTESIAN_POINT('Ctrl Pts',(-56.805615347504,-87.7174646586843,172.016274058689));
#41054=CARTESIAN_POINT('Ctrl Pts',(-55.1807160822689,-87.984971004696,171.81109657639));
#41055=CARTESIAN_POINT('Ctrl Pts',(-53.8903846634539,-88.2168101830669,
172.828569176292));
#41056=CARTESIAN_POINT('Ctrl Pts',(-52.6000532446389,-88.4486493614378,
173.846041776195));
#41057=CARTESIAN_POINT('Ctrl Pts',(-52.4059698999028,-88.5636211711945,
175.490142808619));
#41058=CARTESIAN_POINT('Ctrl Pts',(-52.2118865551668,-88.6785929809511,
177.134243841043));
#41059=CARTESIAN_POINT('Ctrl Pts',(-53.2335642580984,-88.6639565406553,
178.441881219107));
#41060=CARTESIAN_POINT('Ctrl Pts',(-54.25524196103,-88.6493201003596,179.74951859717));
#41061=CARTESIAN_POINT('Ctrl Pts',(-55.9000173520992,-88.5682572836585,
179.954696079469));
#41062=CARTESIAN_POINT('Ctrl Pts',(-57.5447927431684,-88.4871944669575,
180.159873561769));
#41063=CARTESIAN_POINT('Ctrl Pts',(-58.8550002878174,-88.4417988178973,
179.142400961866));
#41064=CARTESIAN_POINT('Ctrl Pts',(-60.1652078324664,-88.3964031688371,
178.124928361964));
#41065=CARTESIAN_POINT('Ctrl Pts',(-60.3791673030365,-88.4678748883911,
176.48082732954));
#41066=CARTESIAN_POINT('Ctrl Pts',(-60.5931267736066,-88.5393466079452,
174.836726297116));
#41067=CARTESIAN_POINT('Ctrl Pts',(-59.591325196509,-88.7404265775517,173.529088919052));
#41068=CARTESIAN_POINT('Ctrl Pts',(-58.5895236194114,-88.9415065471582,
172.221451540989));
#41069=CARTESIAN_POINT('Ctrl Pts',(-56.9646243541763,-89.2090128931699,
172.016274058689));
#41070=CARTESIAN_POINT('Ctrl Pts',(-55.3397250889411,-89.4765192391816,
171.81109657639));
#41071=CARTESIAN_POINT('Ctrl Pts',(-54.0493936701261,-89.7083584175525,
172.828569176292));
#41072=CARTESIAN_POINT('Ctrl Pts',(-52.7590622513111,-89.9401975959235,
173.846041776195));
#41073=CARTESIAN_POINT('Ctrl Pts',(-52.5649789065751,-90.0551694056801,
175.490142808619));
#41074=CARTESIAN_POINT('Ctrl Pts',(-52.370895561839,-90.1701412154367,177.134243841043));
#41075=CARTESIAN_POINT('Ctrl Pts',(-53.3925732647706,-90.1555047751409,
178.441881219107));
#41076=CARTESIAN_POINT('Ctrl Pts',(-54.4142509677022,-90.1408683348452,
179.74951859717));
#41077=CARTESIAN_POINT('Ctrl Pts',(-56.0590263587714,-90.0598055181441,
179.954696079469));
#41078=CARTESIAN_POINT('Ctrl Pts',(-57.7038017498406,-89.9787427014431,
180.159873561769));
#41079=CARTESIAN_POINT('Ctrl Pts',(-59.0140092944896,-89.9333470523829,
179.142400961866));
#41080=CARTESIAN_POINT('Ctrl Pts',(-60.3242168391386,-89.8879514033227,
178.124928361964));
#41081=CARTESIAN_POINT('Ctrl Pts',(-60.5381763097087,-89.9594231228767,
176.48082732954));
#41082=CARTESIAN_POINT('Ctrl Pts',(-60.7521357802788,-90.0308948424308,
174.836726297116));
#41083=CARTESIAN_POINT('Ctrl Pts',(-59.7503342031812,-90.2319748120373,
173.529088919052));
#41084=CARTESIAN_POINT('Ctrl Pts',(-58.7485326260837,-90.4330547816438,
172.221451540989));
#41085=CARTESIAN_POINT('Ctrl Pts',(-57.1236333608485,-90.7005611276555,
172.016274058689));
#41086=CARTESIAN_POINT('Ctrl Pts',(-55.4987340956133,-90.9680674736672,
171.81109657639));
#41087=CARTESIAN_POINT('Ctrl Pts',(-54.2084026767983,-91.1999066520381,
172.828569176292));
#41088=CARTESIAN_POINT('Ctrl Pts',(-52.9180712579833,-91.4317458304091,
173.846041776195));
#41089=CARTESIAN_POINT('Ctrl Pts',(-52.7239879132473,-91.5467176401657,
175.490142808619));
#41090=CARTESIAN_POINT('Ctrl Pts',(-52.5299045685112,-91.6616894499223,
177.134243841043));
#41091=CARTESIAN_POINT('Ctrl Pts',(-53.5515822714428,-91.6470530096265,
178.441881219107));
#41092=CARTESIAN_POINT('Ctrl Pts',(-54.5732599743744,-91.6324165693307,
179.74951859717));
#41093=CARTESIAN_POINT('Ctrl Pts',(-56.2180353654436,-91.5513537526297,
179.954696079469));
#41094=CARTESIAN_POINT('Ctrl Pts',(-57.8628107565128,-91.4702909359287,
180.159873561769));
#41095=CARTESIAN_POINT('Ctrl Pts',(-59.1730183011618,-91.4248952868685,
179.142400961866));
#41096=CARTESIAN_POINT('Ctrl Pts',(-60.4832258458109,-91.3794996378083,
178.124928361964));
#41097=CARTESIAN_POINT('Ctrl Pts',(-60.6971853163809,-91.4509713573623,
176.48082732954));
#41098=CARTESIAN_POINT('Ctrl Pts',(-60.911144786951,-91.5224430769164,174.836726297116));
#41099=CARTESIAN_POINT('Ctrl Pts',(-59.9093432098535,-91.7235230465229,
173.529088919052));
#41100=CARTESIAN_POINT('Ctrl Pts',(-58.9075416327559,-91.9246030161294,
172.221451540989));
#41101=CARTESIAN_POINT('Ctrl Pts',(-57.2826423675207,-92.1921093621411,
172.016274058689));
#41102=CARTESIAN_POINT('Ctrl Pts',(-55.6577431022856,-92.4596157081528,
171.81109657639));
#41103=CARTESIAN_POINT('Ctrl Pts',(-54.3674116834706,-92.6914548865237,
172.828569176292));
#41104=CARTESIAN_POINT('Ctrl Pts',(-53.0770802646556,-92.9232940648947,
173.846041776195));
#41105=CARTESIAN_POINT('Ctrl Pts',(-52.8829969199195,-93.0382658746513,
175.490142808619));
#41106=CARTESIAN_POINT('Ctrl Pts',(-52.6889135751835,-93.1532376844079,
177.134243841043));
#41107=CARTESIAN_POINT('Ctrl Pts',(-53.7105912781151,-93.1386012441121,
178.441881219107));
#41108=CARTESIAN_POINT('Ctrl Pts',(-54.7322689810467,-93.1239648038163,
179.74951859717));
#41109=CARTESIAN_POINT('Ctrl Pts',(-56.3770443721158,-93.0429019871153,
179.954696079469));
#41110=CARTESIAN_POINT('Ctrl Pts',(-58.021819763185,-92.9618391704143,180.159873561769));
#41111=CARTESIAN_POINT('Ctrl Pts',(-59.3320273078341,-92.9164435213541,
179.142400961866));
#41112=CARTESIAN_POINT('Ctrl Pts',(-60.6422348524831,-92.8710478722939,
178.124928361964));
#41113=CARTESIAN_POINT('Ctrl Pts',(-60.8561943230532,-92.9425195918479,
176.48082732954));
#41114=CARTESIAN_POINT('Ctrl Pts',(-61.0701537936233,-93.013991311402,174.836726297116));
#41115=CARTESIAN_POINT('Ctrl Pts',(-60.0683522165257,-93.2150712810085,
173.529088919052));
#41116=CARTESIAN_POINT('Ctrl Pts',(-59.0665506394281,-93.416151250615,172.221451540989));
#41117=CARTESIAN_POINT('Ctrl Pts',(-57.4416513741929,-93.6836575966267,
172.016274058689));
#41118=CARTESIAN_POINT('Ctrl Pts',(-55.8167521089578,-93.9511639426384,
171.81109657639));
#41119=CARTESIAN_POINT('Ctrl Pts',(-54.5264206901428,-94.1830031210093,
172.828569176292));
#41120=CARTESIAN_POINT('Ctrl Pts',(-53.2360892713278,-94.4148422993803,
173.846041776195));
#41121=CARTESIAN_POINT('Ctrl Pts',(-53.0420059265917,-94.5298141091369,
175.490142808619));
#41122=CARTESIAN_POINT('Ctrl Pts',(-52.8479225818557,-94.6447859188935,
177.134243841043));
#41123=CARTESIAN_POINT('Ctrl Pts',(-53.8696002847873,-94.6301494785977,
178.441881219107));
#41124=CARTESIAN_POINT('Ctrl Pts',(-54.8912779877189,-94.615513038302,179.74951859717));
#41125=CARTESIAN_POINT('Ctrl Pts',(-56.5360533787881,-94.5344502216009,
179.954696079469));
#41126=CARTESIAN_POINT('Ctrl Pts',(-58.1808287698573,-94.4533874048999,
180.159873561769));
#41127=CARTESIAN_POINT('Ctrl Pts',(-59.4910363145063,-94.4079917558397,
179.142400961866));
#41128=CARTESIAN_POINT('Ctrl Pts',(-60.8012438591553,-94.3625961067795,
178.124928361964));
#41129=CARTESIAN_POINT('Ctrl Pts',(-61.0152033297254,-94.4340678263335,
176.48082732954));
#41130=CARTESIAN_POINT('Ctrl Pts',(-61.2291628002955,-94.5055395458876,
174.836726297116));
#41131=CARTESIAN_POINT('Ctrl Pts',(-60.2273612231979,-94.7066195154941,
173.529088919052));
#41132=CARTESIAN_POINT('Ctrl Pts',(-59.2255596461003,-94.9076994851006,
172.221451540989));
#41133=CARTESIAN_POINT('Ctrl Pts',(-57.6006603808652,-95.1752058311123,
172.016274058689));
#41134=CARTESIAN_POINT('Ctrl Pts',(-55.97576111563,-95.442712177124,171.81109657639));
#41135=CARTESIAN_POINT('Ctrl Pts',(-54.685429696815,-95.6745513554949,172.828569176292));
#41136=CARTESIAN_POINT('Ctrl Pts',(-53.395098278,-95.9063905338659,173.846041776195));
#41137=CARTESIAN_POINT('Ctrl Pts',(-53.201014933264,-96.0213623436225,175.490142808619));
#41138=CARTESIAN_POINT('Ctrl Pts',(-53.0069315885279,-96.1363341533791,
177.134243841043));
#41139=CARTESIAN_POINT('Ctrl Pts',(-54.0286092914595,-96.1216977130833,
178.441881219107));
#41140=CARTESIAN_POINT('Ctrl Pts',(-55.0502869943911,-96.1070612727875,
179.74951859717));
#41141=CARTESIAN_POINT('Ctrl Pts',(-56.6950623854603,-96.0259984560865,
179.954696079469));
#41142=CARTESIAN_POINT('Ctrl Pts',(-58.3398377765295,-95.9449356393855,
180.159873561769));
#41143=CARTESIAN_POINT('Ctrl Pts',(-59.6500453211785,-95.8995399903253,
179.142400961866));
#41144=CARTESIAN_POINT('Ctrl Pts',(-60.9602528658275,-95.8541443412651,
178.124928361964));
#41145=CARTESIAN_POINT('Ctrl Pts',(-61.1742123363976,-95.9256160608192,
176.48082732954));
#41146=CARTESIAN_POINT('Ctrl Pts',(-61.3881718069677,-95.9970877803732,
174.836726297116));
#41147=CARTESIAN_POINT('Ctrl Pts',(-60.3863702298701,-96.1981677499797,
173.529088919052));
#41148=CARTESIAN_POINT('Ctrl Pts',(-59.3845686527726,-96.3992477195862,
172.221451540989));
#41149=CARTESIAN_POINT('Ctrl Pts',(-57.7596693875374,-96.6667540655979,
172.016274058689));
#41150=CARTESIAN_POINT('Ctrl Pts',(-56.1347701223022,-96.9342604116096,
171.81109657639));
#41151=CARTESIAN_POINT('Ctrl Pts',(-54.8444387034872,-97.1660995899806,
172.828569176292));
#41152=CARTESIAN_POINT('Ctrl Pts',(-53.5541072846722,-97.3979387683514,
173.846041776195));
#41153=CARTESIAN_POINT('Ctrl Pts',(-53.3600239399362,-97.5129105781081,
175.490142808619));
#41154=CARTESIAN_POINT('Ctrl Pts',(-53.1659405952001,-97.6278823878647,
177.134243841043));
#41155=CARTESIAN_POINT('Ctrl Pts',(-54.1876182981317,-97.6132459475689,
178.441881219107));
#41156=CARTESIAN_POINT('Ctrl Pts',(-55.2092960010633,-97.5986095072732,
179.74951859717));
#41157=CARTESIAN_POINT('Ctrl Pts',(-56.8540713921325,-97.5175466905721,
179.954696079469));
#41158=CARTESIAN_POINT('Ctrl Pts',(-58.4988467832017,-97.4364838738711,
180.159873561769));
#41159=CARTESIAN_POINT('Ctrl Pts',(-59.8090543278507,-97.3910882248109,
179.142400961866));
#41160=CARTESIAN_POINT('Ctrl Pts',(-61.1192618724998,-97.3456925757507,
178.124928361964));
#41161=CARTESIAN_POINT('Ctrl Pts',(-61.3332213430699,-97.4171642953048,
176.48082732954));
#41162=CARTESIAN_POINT('Ctrl Pts',(-61.5471808136399,-97.4886360148588,
174.836726297116));
#41163=CARTESIAN_POINT('Ctrl Pts',(-60.5453792365424,-97.6897159844653,
173.529088919052));
#41164=CARTESIAN_POINT('Ctrl Pts',(-59.5435776594448,-97.8907959540718,
172.221451540989));
#41165=CARTESIAN_POINT('Ctrl Pts',(-57.9186783942096,-98.1583023000835,
172.016274058689));
#41166=CARTESIAN_POINT('Ctrl Pts',(-56.2937791289745,-98.4258086460952,
171.81109657639));
#41167=CARTESIAN_POINT('Ctrl Pts',(-55.0034477101595,-98.6576478244661,
172.828569176292));
#41168=CARTESIAN_POINT('Ctrl Pts',(-53.7131162913445,-98.8894870028371,
173.846041776195));
#41169=CARTESIAN_POINT('Ctrl Pts',(-53.5190329466084,-99.0044588125937,
175.490142808619));
#41170=CARTESIAN_POINT('Ctrl Pts',(-53.3249496018724,-99.1194306223503,
177.134243841043));
#41171=CARTESIAN_POINT('Ctrl Pts',(-54.346627304804,-99.1047941820545,178.441881219107));
#41172=CARTESIAN_POINT('Ctrl Pts',(-55.3683050077356,-99.0901577417588,
179.74951859717));
#41173=CARTESIAN_POINT('Ctrl Pts',(-57.0130803988047,-99.0090949250577,
179.954696079469));
#41174=CARTESIAN_POINT('Ctrl Pts',(-58.6578557898739,-98.9280321083567,
180.159873561769));
#41175=CARTESIAN_POINT('Ctrl Pts',(-59.968063334523,-98.8826364592965,179.142400961866));
#41176=CARTESIAN_POINT('Ctrl Pts',(-61.278270879172,-98.8372408102363,178.124928361964));
#41177=CARTESIAN_POINT('Ctrl Pts',(-61.4922303497421,-98.9087125297904,
176.48082732954));
#41178=CARTESIAN_POINT('Ctrl Pts',(-61.7061898203122,-98.9801842493444,
174.836726297116));
#41179=CARTESIAN_POINT('Ctrl Pts',(-60.7043882432146,-99.1812642189509,
173.529088919052));
#41180=CARTESIAN_POINT('Ctrl Pts',(-59.702586666117,-99.3823441885574,172.221451540989));
#41181=CARTESIAN_POINT('Ctrl Pts',(-58.0776874008818,-99.6498505345691,
172.016274058689));
#41182=CARTESIAN_POINT('Ctrl Pts',(-56.4527881356467,-99.9173568805808,
171.81109657639));
#41183=CARTESIAN_POINT('Ctrl Pts',(-55.1624567168317,-100.149196058952,
172.828569176292));
#41184=CARTESIAN_POINT('Ctrl Pts',(-53.8721252980167,-100.381035237323,
173.846041776195));
#41185=CARTESIAN_POINT('Ctrl Pts',(-53.6780419532806,-100.496007047079,
175.490142808619));
#41186=CARTESIAN_POINT('Ctrl Pts',(-53.4839586085446,-100.610978856836,
177.134243841043));
#41187=CARTESIAN_POINT('Ctrl Pts',(-54.5056363114762,-100.59634241654,178.441881219107));
#41188=CARTESIAN_POINT('Ctrl Pts',(-55.5273140144078,-100.581705976244,
179.74951859717));
#41189=CARTESIAN_POINT('Ctrl Pts',(-57.172089405477,-100.500643159543,179.954696079469));
#41190=CARTESIAN_POINT('Ctrl Pts',(-58.8168647965462,-100.419580342842,
180.159873561769));
#41191=CARTESIAN_POINT('Ctrl Pts',(-60.1270723411952,-100.374184693782,
179.142400961866));
#41192=CARTESIAN_POINT('Ctrl Pts',(-61.4372798858442,-100.328789044722,
178.124928361964));
#41193=CARTESIAN_POINT('Ctrl Pts',(-61.6512393564143,-100.400260764276,
176.48082732954));
#41194=CARTESIAN_POINT('Ctrl Pts',(-61.8651988269844,-100.47173248383,174.836726297116));
#41195=CARTESIAN_POINT('Ctrl Pts',(-60.8633972498868,-100.672812453437,
173.529088919052));
#41196=CARTESIAN_POINT('Ctrl Pts',(-59.8615956727892,-100.873892423043,
172.221451540989));
#41197=CARTESIAN_POINT('Ctrl Pts',(-58.2366964075541,-101.141398769055,
172.016274058689));
#41198=CARTESIAN_POINT('Ctrl Pts',(-56.6117971423189,-101.408905115066,
171.81109657639));
#41199=CARTESIAN_POINT('Ctrl Pts',(-55.3214657235039,-101.640744293437,
172.828569176292));
#41200=CARTESIAN_POINT('Ctrl Pts',(-54.0311343046889,-101.872583471808,
173.846041776195));
#41201=CARTESIAN_POINT('Ctrl Pts',(-53.8370509599529,-101.987555281565,
175.490142808619));
#41202=CARTESIAN_POINT('Ctrl Pts',(-53.6429676152168,-102.102527091322,
177.134243841043));
#41203=CARTESIAN_POINT('Ctrl Pts',(-54.6646453181484,-102.087890651026,
178.441881219107));
#41204=CARTESIAN_POINT('Ctrl Pts',(-55.68632302108,-102.07325421073,179.74951859717));
#41205=CARTESIAN_POINT('Ctrl Pts',(-57.3310984121492,-101.992191394029,
179.954696079469));
#41206=CARTESIAN_POINT('Ctrl Pts',(-58.9758738032184,-101.911128577328,
180.159873561769));
#41207=CARTESIAN_POINT('Ctrl Pts',(-60.2860813478674,-101.865732928268,
179.142400961866));
#41208=CARTESIAN_POINT('Ctrl Pts',(-61.5962888925164,-101.820337279207,
178.124928361964));
#41209=CARTESIAN_POINT('Ctrl Pts',(-61.8102483630865,-101.891808998762,
176.48082732954));
#41210=CARTESIAN_POINT('Ctrl Pts',(-62.0242078336566,-101.963280718316,
174.836726297116));
#41211=CARTESIAN_POINT('Ctrl Pts',(-61.022406256559,-102.164360687922,173.529088919052));
#41212=CARTESIAN_POINT('Ctrl Pts',(-60.0206046794615,-102.365440657529,
172.221451540989));
#41213=CARTESIAN_POINT('Ctrl Pts',(-58.3957054142263,-102.63294700354,172.016274058689));
#41214=CARTESIAN_POINT('Ctrl Pts',(-56.7708061489911,-102.900453349552,
171.81109657639));
#41215=CARTESIAN_POINT('Ctrl Pts',(-55.4804747301761,-103.132292527923,
172.828569176292));
#41216=CARTESIAN_POINT('Ctrl Pts',(-54.1901433113612,-103.364131706294,
173.846041776195));
#41217=CARTESIAN_POINT('Ctrl Pts',(-53.9960599666251,-103.479103516051,
175.490142808619));
#41218=CARTESIAN_POINT('Ctrl Pts',(-53.801976621889,-103.594075325807,177.134243841043));
#41219=CARTESIAN_POINT('Ctrl Pts',(-54.8236543248206,-103.579438885511,
178.441881219107));
#41220=CARTESIAN_POINT('Ctrl Pts',(-55.8453320277522,-103.564802445216,
179.74951859717));
#41221=CARTESIAN_POINT('Ctrl Pts',(-57.4901074188214,-103.483739628515,
179.954696079469));
#41222=CARTESIAN_POINT('Ctrl Pts',(-59.1348828098906,-103.402676811814,
180.159873561769));
#41223=CARTESIAN_POINT('Ctrl Pts',(-60.4450903545396,-103.357281162753,
179.142400961866));
#41224=CARTESIAN_POINT('Ctrl Pts',(-61.7552978991887,-103.311885513693,
178.124928361964));
#41225=CARTESIAN_POINT('Ctrl Pts',(-61.9692573697588,-103.383357233247,
176.48082732954));
#41226=CARTESIAN_POINT('Ctrl Pts',(-62.1832168403288,-103.454828952801,
174.836726297116));
#41227=CARTESIAN_POINT('Ctrl Pts',(-61.1814152632313,-103.655908922408,
173.529088919052));
#41228=CARTESIAN_POINT('Ctrl Pts',(-60.1796136861337,-103.856988892014,
172.221451540989));
#41229=CARTESIAN_POINT('Ctrl Pts',(-58.5547144208985,-104.124495238026,
172.016274058689));
#41230=CARTESIAN_POINT('Ctrl Pts',(-56.9298151556634,-104.392001584038,
171.81109657639));
#41231=CARTESIAN_POINT('Ctrl Pts',(-55.6394837368484,-104.623840762409,
172.828569176292));
#41232=CARTESIAN_POINT('Ctrl Pts',(-54.3491523180334,-104.855679940779,
173.846041776195));
#41233=CARTESIAN_POINT('Ctrl Pts',(-54.1550689732973,-104.970651750536,
175.490142808619));
#41234=CARTESIAN_POINT('Ctrl Pts',(-53.9609856285613,-105.085623560293,
177.134243841043));
#41235=CARTESIAN_POINT('Ctrl Pts',(-54.9826633314929,-105.070987119997,
178.441881219107));
#41236=CARTESIAN_POINT('Ctrl Pts',(-56.0043410344245,-105.056350679701,
179.74951859717));
#41237=CARTESIAN_POINT('Ctrl Pts',(-57.6491164254937,-104.975287863,179.954696079469));
#41238=CARTESIAN_POINT('Ctrl Pts',(-59.2938918165629,-104.894225046299,
180.159873561769));
#41239=CARTESIAN_POINT('Ctrl Pts',(-60.6040993612119,-104.848829397239,
179.142400961866));
#41240=CARTESIAN_POINT('Ctrl Pts',(-61.9143069058609,-104.803433748179,
178.124928361964));
#41241=CARTESIAN_POINT('Ctrl Pts',(-62.128266376431,-104.874905467733,176.48082732954));
#41242=CARTESIAN_POINT('Ctrl Pts',(-62.3422258470011,-104.946377187287,
174.836726297116));
#41243=CARTESIAN_POINT('Ctrl Pts',(-61.3404242699035,-105.147457156893,
173.529088919052));
#41244=CARTESIAN_POINT('Ctrl Pts',(-60.3386226928059,-105.3485371265,172.221451540989));
#41245=CARTESIAN_POINT('Ctrl Pts',(-58.7137234275708,-105.616043472511,
172.016274058689));
#41246=CARTESIAN_POINT('Ctrl Pts',(-57.0888241623356,-105.883549818523,
171.81109657639));
#41247=CARTESIAN_POINT('Ctrl Pts',(-55.7984927435206,-106.115388996894,
172.828569176292));
#41248=CARTESIAN_POINT('Ctrl Pts',(-54.5081613247056,-106.347228175265,
173.846041776195));
#41249=CARTESIAN_POINT('Ctrl Pts',(-54.3140779799695,-106.462199985022,
175.490142808619));
#41250=CARTESIAN_POINT('Ctrl Pts',(-54.1199946352335,-106.577171794778,
177.134243841043));
#41251=CARTESIAN_POINT('Ctrl Pts',(-55.1416723381651,-106.562535354483,
178.441881219107));
#41252=CARTESIAN_POINT('Ctrl Pts',(-56.1633500410967,-106.547898914187,
179.74951859717));
#41253=CARTESIAN_POINT('Ctrl Pts',(-57.8081254321659,-106.466836097486,
179.954696079469));
#41254=CARTESIAN_POINT('Ctrl Pts',(-59.4529008232351,-106.385773280785,
180.159873561769));
#41255=CARTESIAN_POINT('Ctrl Pts',(-60.7631083678841,-106.340377631725,
179.142400961866));
#41256=CARTESIAN_POINT('Ctrl Pts',(-62.0733159125331,-106.294981982664,
178.124928361964));
#41257=CARTESIAN_POINT('Ctrl Pts',(-62.2872753831032,-106.366453702218,
176.48082732954));
#41258=CARTESIAN_POINT('Ctrl Pts',(-62.5012348536733,-106.437925421772,
174.836726297116));
#41259=CARTESIAN_POINT('Ctrl Pts',(-61.4994332765757,-106.639005391379,
173.529088919052));
#41260=CARTESIAN_POINT('Ctrl Pts',(-60.4976316994782,-106.840085360985,
172.221451540989));
#41261=CARTESIAN_POINT('Ctrl Pts',(-58.872732434243,-107.107591706997,172.016274058689));
#41262=CARTESIAN_POINT('Ctrl Pts',(-57.2478331690078,-107.375098053009,
171.81109657639));
#41263=CARTESIAN_POINT('Ctrl Pts',(-55.9575017501928,-107.60693723138,172.828569176292));
#41264=CARTESIAN_POINT('Ctrl Pts',(-54.6671703313778,-107.838776409751,
173.846041776195));
#41265=CARTESIAN_POINT('Ctrl Pts',(-54.4730869866418,-107.953748219507,
175.490142808619));
#41266=CARTESIAN_POINT('Ctrl Pts',(-54.2790036419057,-108.068720029264,
177.134243841043));
#41267=CARTESIAN_POINT('Ctrl Pts',(-55.3006813448373,-108.054083588968,
178.441881219107));
#41268=CARTESIAN_POINT('Ctrl Pts',(-56.3223590477689,-108.039447148672,
179.74951859717));
#41269=CARTESIAN_POINT('Ctrl Pts',(-57.9671344388381,-107.958384331971,
179.954696079469));
#41270=CARTESIAN_POINT('Ctrl Pts',(-59.6119098299073,-107.87732151527,180.159873561769));
#41271=CARTESIAN_POINT('Ctrl Pts',(-60.9221173745563,-107.83192586621,179.142400961866));
#41272=CARTESIAN_POINT('Ctrl Pts',(-62.2323249192054,-107.78653021715,178.124928361964));
#41273=CARTESIAN_POINT('Ctrl Pts',(-62.4462843897754,-107.858001936704,
176.48082732954));
#41274=CARTESIAN_POINT('Ctrl Pts',(-62.6602438603455,-107.929473656258,
174.836726297116));
#41275=CARTESIAN_POINT('Ctrl Pts',(-61.6584422832479,-108.130553625865,
173.529088919052));
#41276=CARTESIAN_POINT('Ctrl Pts',(-60.6566407061504,-108.331633595471,
172.221451540989));
#41277=CARTESIAN_POINT('Ctrl Pts',(-59.0317414409152,-108.599139941483,
172.016274058689));
#41278=CARTESIAN_POINT('Ctrl Pts',(-57.4068421756801,-108.866646287494,
171.81109657639));
#41279=CARTESIAN_POINT('Ctrl Pts',(-56.1165107568651,-109.098485465865,
172.828569176292));
#41280=CARTESIAN_POINT('Ctrl Pts',(-54.8261793380501,-109.330324644236,
173.846041776195));
#41281=CARTESIAN_POINT('Ctrl Pts',(-54.632095993314,-109.445296453993,175.490142808619));
#41282=CARTESIAN_POINT('Ctrl Pts',(-54.438012648578,-109.56026826375,177.134243841043));
#41283=CARTESIAN_POINT('Ctrl Pts',(-55.4596903515096,-109.545631823454,
178.441881219107));
#41284=CARTESIAN_POINT('Ctrl Pts',(-56.4813680544411,-109.530995383158,
179.74951859717));
#41285=CARTESIAN_POINT('Ctrl Pts',(-58.1261434455103,-109.449932566457,
179.954696079469));
#41286=CARTESIAN_POINT('Ctrl Pts',(-59.7709188365795,-109.368869749756,
180.159873561769));
#41287=CARTESIAN_POINT('Ctrl Pts',(-61.0811263812286,-109.323474100696,
179.142400961866));
#41288=CARTESIAN_POINT('Ctrl Pts',(-62.3913339258776,-109.278078451635,
178.124928361964));
#41289=CARTESIAN_POINT('Ctrl Pts',(-62.6052933964477,-109.34955017119,176.48082732954));
#41290=CARTESIAN_POINT('Ctrl Pts',(-62.8192528670178,-109.421021890744,
174.836726297116));
#41291=CARTESIAN_POINT('Ctrl Pts',(-61.8174512899202,-109.62210186035,173.529088919052));
#41292=CARTESIAN_POINT('Ctrl Pts',(-60.8156497128226,-109.823181829957,
172.221451540989));
#41293=CARTESIAN_POINT('Ctrl Pts',(-59.1907504475874,-110.090688175968,
172.016274058689));
#41294=CARTESIAN_POINT('Ctrl Pts',(-57.5658511823523,-110.35819452198,171.81109657639));
#41295=CARTESIAN_POINT('Ctrl Pts',(-56.2755197635373,-110.590033700351,
172.828569176292));
#41296=CARTESIAN_POINT('Ctrl Pts',(-54.9851883447223,-110.821872878722,
173.846041776195));
#41297=CARTESIAN_POINT('Ctrl Pts',(-54.7911049999862,-110.936844688478,
175.490142808619));
#41298=CARTESIAN_POINT('Ctrl Pts',(-54.5970216552502,-111.051816498235,
177.134243841043));
#41299=CARTESIAN_POINT('Ctrl Pts',(-55.6186993581818,-111.037180057939,
178.441881219107));
#41300=CARTESIAN_POINT('Ctrl Pts',(-56.6403770611134,-111.022543617644,
179.74951859717));
#41301=CARTESIAN_POINT('Ctrl Pts',(-58.2851524521826,-110.941480800943,
179.954696079469));
#41302=CARTESIAN_POINT('Ctrl Pts',(-59.9299278432518,-110.860417984242,
180.159873561769));
#41303=CARTESIAN_POINT('Ctrl Pts',(-61.2401353879008,-110.815022335181,
179.142400961866));
#41304=CARTESIAN_POINT('Ctrl Pts',(-62.5503429325498,-110.769626686121,
178.124928361964));
#41305=CARTESIAN_POINT('Ctrl Pts',(-62.7643024031199,-110.841098405675,
176.48082732954));
#41306=CARTESIAN_POINT('Ctrl Pts',(-62.97826187369,-110.912570125229,174.836726297116));
#41307=CARTESIAN_POINT('Ctrl Pts',(-61.9764602965924,-111.113650094836,
173.529088919052));
#41308=CARTESIAN_POINT('Ctrl Pts',(-60.9746587194948,-111.314730064442,
172.221451540989));
#41309=CARTESIAN_POINT('Ctrl Pts',(-59.3497594542597,-111.582236410454,
172.016274058689));
#41310=CARTESIAN_POINT('Ctrl Pts',(-57.7248601890245,-111.849742756466,
171.81109657639));
#41311=CARTESIAN_POINT('Ctrl Pts',(-56.4345287702095,-112.081581934837,
172.828569176292));
#41312=CARTESIAN_POINT('Ctrl Pts',(-55.1441973513945,-112.313421113207,
173.846041776195));
#41313=CARTESIAN_POINT('Ctrl Pts',(-54.9501140066585,-112.428392922964,
175.490142808619));
#41314=CARTESIAN_POINT('Ctrl Pts',(-54.7560306619224,-112.543364732721,
177.134243841043));
#41315=CARTESIAN_POINT('Ctrl Pts',(-55.777708364854,-112.528728292425,178.441881219107));
#41316=CARTESIAN_POINT('Ctrl Pts',(-56.7993860677856,-112.514091852129,
179.74951859717));
#41317=CARTESIAN_POINT('Ctrl Pts',(-58.4441614588548,-112.433029035428,
179.954696079469));
#41318=CARTESIAN_POINT('Ctrl Pts',(-60.088936849924,-112.351966218727,180.159873561769));
#41319=CARTESIAN_POINT('Ctrl Pts',(-61.399144394573,-112.306570569667,179.142400961866));
#41320=CARTESIAN_POINT('Ctrl Pts',(-62.709351939222,-112.261174920607,178.124928361964));
#41321=CARTESIAN_POINT('Ctrl Pts',(-62.9233114097921,-112.332646640161,
176.48082732954));
#41322=CARTESIAN_POINT('Ctrl Pts',(-63.1372708803622,-112.404118359715,
174.836726297116));
#41323=CARTESIAN_POINT('Ctrl Pts',(-62.1354693032646,-112.605198329321,
173.529088919052));
#41324=CARTESIAN_POINT('Ctrl Pts',(-61.1336677261671,-112.806278298928,
172.221451540989));
#41325=CARTESIAN_POINT('Ctrl Pts',(-59.5087684609319,-113.07378464494,172.016274058689));
#41326=CARTESIAN_POINT('Ctrl Pts',(-57.8838691956967,-113.341290990951,
171.81109657639));
#41327=CARTESIAN_POINT('Ctrl Pts',(-56.5935377768817,-113.573130169322,
172.828569176292));
#41328=CARTESIAN_POINT('Ctrl Pts',(-55.3032063580667,-113.804969347693,
173.846041776195));
#41329=CARTESIAN_POINT('Ctrl Pts',(-55.1091230133307,-113.91994115745,175.490142808619));
#41330=CARTESIAN_POINT('Ctrl Pts',(-54.9150396685946,-114.034912967206,
177.134243841043));
#41331=CARTESIAN_POINT('Ctrl Pts',(-55.9367173715262,-114.020276526911,
178.441881219107));
#41332=CARTESIAN_POINT('Ctrl Pts',(-56.9583950744578,-114.005640086615,
179.74951859717));
#41333=CARTESIAN_POINT('Ctrl Pts',(-58.603170465527,-113.924577269914,179.954696079469));
#41334=CARTESIAN_POINT('Ctrl Pts',(-60.2479458565962,-113.843514453213,
180.159873561769));
#41335=CARTESIAN_POINT('Ctrl Pts',(-61.5581534012452,-113.798118804152,
179.142400961866));
#41336=CARTESIAN_POINT('Ctrl Pts',(-62.8683609458943,-113.752723155092,
178.124928361964));
#41337=CARTESIAN_POINT('Ctrl Pts',(-63.0823204164643,-113.824194874646,
176.48082732954));
#41338=CARTESIAN_POINT('Ctrl Pts',(-63.2962798870344,-113.8956665942,174.836726297116));
#41339=CARTESIAN_POINT('Ctrl Pts',(-62.2944783099369,-114.096746563807,
173.529088919052));
#41340=CARTESIAN_POINT('Ctrl Pts',(-61.2926767328393,-114.297826533413,
172.221451540989));
#41341=CARTESIAN_POINT('Ctrl Pts',(-59.6677774676041,-114.565332879425,
172.016274058689));
#41342=CARTESIAN_POINT('Ctrl Pts',(-58.042878202369,-114.832839225437,171.81109657639));
#41343=CARTESIAN_POINT('Ctrl Pts',(-56.752546783554,-115.064678403808,172.828569176292));
#41344=CARTESIAN_POINT('Ctrl Pts',(-55.462215364739,-115.296517582179,173.846041776195));
#41345=CARTESIAN_POINT('Ctrl Pts',(-55.2681320200029,-115.411489391935,
175.490142808619));
#41346=CARTESIAN_POINT('Ctrl Pts',(-55.0740486752669,-115.526461201692,
177.134243841043));
#41347=CARTESIAN_POINT('Ctrl Pts',(-56.0957263781985,-115.511824761396,
178.441881219107));
#41348=CARTESIAN_POINT('Ctrl Pts',(-57.1174040811301,-115.4971883211,179.74951859717));
#41349=CARTESIAN_POINT('Ctrl Pts',(-58.7621794721992,-115.416125504399,
179.954696079469));
#41350=CARTESIAN_POINT('Ctrl Pts',(-60.4069548632684,-115.335062687698,
180.159873561769));
#41351=CARTESIAN_POINT('Ctrl Pts',(-61.7171624079175,-115.289667038638,
179.142400961866));
#41352=CARTESIAN_POINT('Ctrl Pts',(-63.0273699525665,-115.244271389578,
178.124928361964));
#41353=CARTESIAN_POINT('Ctrl Pts',(-63.2413294231366,-115.315743109132,
176.48082732954));
#41354=CARTESIAN_POINT('Ctrl Pts',(-63.4552888937067,-115.387214828686,
174.836726297116));
#41355=CARTESIAN_POINT('Ctrl Pts',(-62.4534873166091,-115.588294798292,
173.529088919052));
#41356=CARTESIAN_POINT('Ctrl Pts',(-61.4516857395115,-115.789374767899,
172.221451540989));
#41357=CARTESIAN_POINT('Ctrl Pts',(-59.8267864742763,-116.056881113911,
172.016274058689));
#41358=CARTESIAN_POINT('Ctrl Pts',(-58.2018872090412,-116.324387459922,
171.81109657639));
#41359=CARTESIAN_POINT('Ctrl Pts',(-56.9115557902262,-116.556226638293,
172.828569176292));
#41360=CARTESIAN_POINT('Ctrl Pts',(-55.6212243714112,-116.788065816664,
173.846041776195));
#41361=CARTESIAN_POINT('Ctrl Pts',(-55.4271410266751,-116.903037626421,
175.490142808619));
#41362=CARTESIAN_POINT('Ctrl Pts',(-55.2330576819391,-117.018009436178,
177.134243841043));
#41363=CARTESIAN_POINT('Ctrl Pts',(-56.2547353848707,-117.003372995882,
178.441881219107));
#41364=CARTESIAN_POINT('Ctrl Pts',(-57.2764130878023,-116.988736555586,
179.74951859717));
#41365=CARTESIAN_POINT('Ctrl Pts',(-58.9211884788715,-116.907673738885,
179.954696079469));
#41366=CARTESIAN_POINT('Ctrl Pts',(-60.5659638699407,-116.826610922184,
180.159873561769));
#41367=CARTESIAN_POINT('Ctrl Pts',(-61.8761714145897,-116.781215273124,
179.142400961866));
#41368=CARTESIAN_POINT('Ctrl Pts',(-63.1863789592387,-116.735819624063,
178.124928361964));
#41369=CARTESIAN_POINT('Ctrl Pts',(-63.4003384298088,-116.807291343618,
176.48082732954));
#41370=CARTESIAN_POINT('Ctrl Pts',(-63.6142979003789,-116.878763063172,
174.836726297116));
#41371=CARTESIAN_POINT('Ctrl Pts',(-62.6124963232813,-117.079843032778,
173.529088919052));
#41372=CARTESIAN_POINT('Ctrl Pts',(-61.6106947461837,-117.280923002385,
172.221451540989));
#41373=CARTESIAN_POINT('Ctrl Pts',(-59.9857954809486,-117.548429348396,
172.016274058689));
#41374=CARTESIAN_POINT('Ctrl Pts',(-58.3608962157134,-117.815935694408,
171.81109657639));
#41375=CARTESIAN_POINT('Ctrl Pts',(-57.0705647968984,-118.047774872779,
172.828569176292));
#41376=CARTESIAN_POINT('Ctrl Pts',(-55.7802333780834,-118.27961405115,173.846041776195));
#41377=CARTESIAN_POINT('Ctrl Pts',(-55.5861500333474,-118.394585860907,
175.490142808619));
#41378=CARTESIAN_POINT('Ctrl Pts',(-55.3920666886113,-118.509557670663,
177.134243841043));
#41379=CARTESIAN_POINT('Ctrl Pts',(-56.4137443915429,-118.494921230367,
178.441881219107));
#41380=CARTESIAN_POINT('Ctrl Pts',(-57.4354220944745,-118.480284790072,
179.74951859717));
#41381=CARTESIAN_POINT('Ctrl Pts',(-59.0801974855437,-118.399221973371,
179.954696079469));
#41382=CARTESIAN_POINT('Ctrl Pts',(-60.7249728766129,-118.31815915667,180.159873561769));
#41383=CARTESIAN_POINT('Ctrl Pts',(-62.0351804212619,-118.272763507609,
179.142400961866));
#41384=CARTESIAN_POINT('Ctrl Pts',(-63.345387965911,-118.227367858549,178.124928361964));
#41385=CARTESIAN_POINT('Ctrl Pts',(-63.559347436481,-118.298839578103,176.48082732954));
#41386=CARTESIAN_POINT('Ctrl Pts',(-63.7733069070511,-118.370311297657,
174.836726297116));
#41387=CARTESIAN_POINT('Ctrl Pts',(-62.7715053299535,-118.571391267264,
173.529088919052));
#41388=CARTESIAN_POINT('Ctrl Pts',(-61.769703752856,-118.77247123687,172.221451540989));
#41389=CARTESIAN_POINT('Ctrl Pts',(-60.1448044876208,-119.039977582882,
172.016274058689));
#41390=CARTESIAN_POINT('Ctrl Pts',(-58.5199052223856,-119.307483928894,
171.81109657639));
#41391=CARTESIAN_POINT('Ctrl Pts',(-57.2295738035707,-119.539323107265,
172.828569176292));
#41392=CARTESIAN_POINT('Ctrl Pts',(-55.9392423847557,-119.771162285635,
173.846041776195));
#41393=CARTESIAN_POINT('Ctrl Pts',(-55.7451590400196,-119.886134095392,
175.490142808619));
#41394=CARTESIAN_POINT('Ctrl Pts',(-55.5510756952835,-120.001105905149,
177.134243841043));
#41395=CARTESIAN_POINT('Ctrl Pts',(-56.5727533982151,-119.986469464853,
178.441881219107));
#41396=CARTESIAN_POINT('Ctrl Pts',(-57.5944311011467,-119.971833024557,
179.74951859717));
#41397=CARTESIAN_POINT('Ctrl Pts',(-59.2392064922159,-119.890770207856,
179.954696079469));
#41398=CARTESIAN_POINT('Ctrl Pts',(-60.8839818832851,-119.809707391155,
180.159873561769));
#41399=CARTESIAN_POINT('Ctrl Pts',(-62.1941894279341,-119.764311742095,
179.142400961866));
#41400=CARTESIAN_POINT('Ctrl Pts',(-63.5043969725832,-119.718916093035,
178.124928361964));
#41401=CARTESIAN_POINT('Ctrl Pts',(-63.7183564431533,-119.790387812589,
176.48082732954));
#41402=CARTESIAN_POINT('Ctrl Pts',(-63.9323159137233,-119.861859532143,
174.836726297116));
#41403=CARTESIAN_POINT('Ctrl Pts',(-62.9305143366258,-120.062939501749,
173.529088919052));
#41404=CARTESIAN_POINT('Ctrl Pts',(-61.9287127595282,-120.264019471356,
172.221451540989));
#41405=CARTESIAN_POINT('Ctrl Pts',(-60.303813494293,-120.531525817368,172.016274058689));
#41406=CARTESIAN_POINT('Ctrl Pts',(-58.6789142290579,-120.799032163379,
171.81109657639));
#41407=CARTESIAN_POINT('Ctrl Pts',(-57.3885828102429,-121.03087134175,172.828569176292));
#41408=CARTESIAN_POINT('Ctrl Pts',(-56.0982513914279,-121.262710520121,
173.846041776195));
#41409=CARTESIAN_POINT('Ctrl Pts',(-55.9041680466918,-121.377682329878,
175.490142808619));
#41410=CARTESIAN_POINT('Ctrl Pts',(-55.7100847019558,-121.492654139634,
177.134243841043));
#41411=CARTESIAN_POINT('Ctrl Pts',(-56.7317624048874,-121.478017699339,
178.441881219107));
#41412=CARTESIAN_POINT('Ctrl Pts',(-57.753440107819,-121.463381259043,179.74951859717));
#41413=CARTESIAN_POINT('Ctrl Pts',(-59.3982154988882,-121.382318442342,
179.954696079469));
#41414=CARTESIAN_POINT('Ctrl Pts',(-61.0429908899573,-121.301255625641,
180.159873561769));
#41415=CARTESIAN_POINT('Ctrl Pts',(-62.3531984346064,-121.25585997658,179.142400961866));
#41416=CARTESIAN_POINT('Ctrl Pts',(-63.6634059792554,-121.21046432752,178.124928361964));
#41417=CARTESIAN_POINT('Ctrl Pts',(-63.8773654498255,-121.281936047074,
176.48082732954));
#41418=CARTESIAN_POINT('Ctrl Pts',(-64.0913249203956,-121.353407766628,
174.836726297116));
#41419=CARTESIAN_POINT('Ctrl Pts',(-63.089523343298,-121.554487736235,173.529088919052));
#41420=CARTESIAN_POINT('Ctrl Pts',(-62.0877217662004,-121.755567705841,
172.221451540989));
#41421=CARTESIAN_POINT('Ctrl Pts',(-60.4628225009653,-122.023074051853,
172.016274058689));
#41422=CARTESIAN_POINT('Ctrl Pts',(-58.8379232357301,-122.290580397865,
171.81109657639));
#41423=CARTESIAN_POINT('Ctrl Pts',(-57.5475918169151,-122.522419576236,
172.828569176292));
#41424=CARTESIAN_POINT('Ctrl Pts',(-56.2572603981001,-122.754258754607,
173.846041776195));
#41425=CARTESIAN_POINT('Ctrl Pts',(-56.0631770533641,-122.869230564363,
175.490142808619));
#41426=CARTESIAN_POINT('Ctrl Pts',(-55.869093708628,-122.98420237412,177.134243841043));
#41427=CARTESIAN_POINT('Ctrl Pts',(-56.8907714115596,-122.969565933824,
178.441881219107));
#41428=CARTESIAN_POINT('Ctrl Pts',(-57.9124491144912,-122.954929493528,
179.74951859717));
#41429=CARTESIAN_POINT('Ctrl Pts',(-59.5572245055604,-122.873866676827,
179.954696079469));
#41430=CARTESIAN_POINT('Ctrl Pts',(-61.2019998966296,-122.792803860126,
180.159873561769));
#41431=CARTESIAN_POINT('Ctrl Pts',(-62.5122074412786,-122.747408211066,
179.142400961866));
#41432=CARTESIAN_POINT('Ctrl Pts',(-63.8224149859276,-122.702012562006,
178.124928361964));
#41433=CARTESIAN_POINT('Ctrl Pts',(-64.0363744564977,-122.77348428156,176.48082732954));
#41434=CARTESIAN_POINT('Ctrl Pts',(-64.2503339270678,-122.844956001114,
174.836726297116));
#41435=CARTESIAN_POINT('Ctrl Pts',(-63.2485323499702,-123.046035970721,
173.529088919052));
#41436=CARTESIAN_POINT('Ctrl Pts',(-62.2467307728726,-123.247115940327,
172.221451540989));
#41437=CARTESIAN_POINT('Ctrl Pts',(-60.6218315076375,-123.514622286339,
172.016274058689));
#41438=CARTESIAN_POINT('Ctrl Pts',(-58.9969322424023,-123.78212863235,171.81109657639));
#41439=CARTESIAN_POINT('Ctrl Pts',(-57.7066008235873,-124.013967810721,
172.828569176292));
#41440=CARTESIAN_POINT('Ctrl Pts',(-56.4162694047723,-124.245806989092,
173.846041776195));
#41441=CARTESIAN_POINT('Ctrl Pts',(-56.2221860600363,-124.360778798849,
175.490142808619));
#41442=CARTESIAN_POINT('Ctrl Pts',(-56.0281027153002,-124.475750608606,
177.134243841043));
#41443=CARTESIAN_POINT('Ctrl Pts',(-57.0497804182318,-124.46111416831,178.441881219107));
#41444=CARTESIAN_POINT('Ctrl Pts',(-58.0714581211634,-124.446477728014,
179.74951859717));
#41445=CARTESIAN_POINT('Ctrl Pts',(-59.7162335122326,-124.365414911313,
179.954696079469));
#41446=CARTESIAN_POINT('Ctrl Pts',(-61.3610089033018,-124.284352094612,
180.159873561769));
#41447=CARTESIAN_POINT('Ctrl Pts',(-62.6712164479508,-124.238956445552,
179.142400961866));
#41448=CARTESIAN_POINT('Ctrl Pts',(-63.9814239925999,-124.193560796491,
178.124928361964));
#41449=CARTESIAN_POINT('Ctrl Pts',(-64.1953834631699,-124.265032516046,
176.48082732954));
#41450=CARTESIAN_POINT('Ctrl Pts',(-64.40934293374,-124.3365042356,174.836726297116));
#41451=CARTESIAN_POINT('Ctrl Pts',(-63.4075413566424,-124.537584205206,
173.529088919052));
#41452=CARTESIAN_POINT('Ctrl Pts',(-62.4057397795449,-124.738664174813,
172.221451540989));
#41453=CARTESIAN_POINT('Ctrl Pts',(-60.7808405143097,-125.006170520824,
172.016274058689));
#41454=CARTESIAN_POINT('Ctrl Pts',(-59.1559412490746,-125.273676866836,
171.81109657639));
#41455=CARTESIAN_POINT('Ctrl Pts',(-57.8656098302596,-125.505516045207,
172.828569176292));
#41456=CARTESIAN_POINT('Ctrl Pts',(-56.5752784114446,-125.737355223578,
173.846041776195));
#41457=CARTESIAN_POINT('Ctrl Pts',(-56.3811950667085,-125.852327033334,
175.490142808619));
#41458=CARTESIAN_POINT('Ctrl Pts',(-56.1871117219724,-125.967298843091,
177.134243841043));
#41459=CARTESIAN_POINT('Ctrl Pts',(-57.208789424904,-125.952662402795,178.441881219107));
#41460=CARTESIAN_POINT('Ctrl Pts',(-58.2304671278357,-125.9380259625,179.74951859717));
#41461=CARTESIAN_POINT('Ctrl Pts',(-59.8752425189048,-125.856963145799,
179.954696079469));
#41462=CARTESIAN_POINT('Ctrl Pts',(-61.520017909974,-125.775900329098,180.159873561769));
#41463=CARTESIAN_POINT('Ctrl Pts',(-62.8302254546231,-125.730504680037,
179.142400961866));
#41464=CARTESIAN_POINT('Ctrl Pts',(-64.1404329992721,-125.685109030977,
178.124928361964));
#41465=CARTESIAN_POINT('Ctrl Pts',(-64.3543924698422,-125.756580750531,
176.48082732954));
#41466=CARTESIAN_POINT('Ctrl Pts',(-64.5683519404122,-125.828052470085,
174.836726297116));
#41467=CARTESIAN_POINT('Ctrl Pts',(-63.5665503633147,-126.029132439692,
173.529088919052));
#41468=CARTESIAN_POINT('Ctrl Pts',(-62.5647487862171,-126.230212409298,
172.221451540989));
#41469=CARTESIAN_POINT('Ctrl Pts',(-60.9398495209819,-126.49771875531,172.016274058689));
#41470=CARTESIAN_POINT('Ctrl Pts',(-59.3149502557468,-126.765225101322,
171.81109657639));
#41471=CARTESIAN_POINT('Ctrl Pts',(-58.0246188369318,-126.997064279693,
172.828569176292));
#41472=CARTESIAN_POINT('Ctrl Pts',(-56.7342874181168,-127.228903458063,
173.846041776195));
#41473=CARTESIAN_POINT('Ctrl Pts',(-56.5402040733807,-127.34387526782,175.490142808619));
#41474=CARTESIAN_POINT('Ctrl Pts',(-56.3461207286447,-127.458847077577,
177.134243841043));
#41475=CARTESIAN_POINT('Ctrl Pts',(-57.3677984315763,-127.444210637281,
178.441881219107));
#41476=CARTESIAN_POINT('Ctrl Pts',(-58.0247571031797,-127.434799120962,
179.282717534088));
#41477=CARTESIAN_POINT('Ctrl Pts',(-59.0118785952597,-127.394648976958,
179.686725372425));
#41478=CARTESIAN_POINT('Ctrl Pts',(-50.1268408042676,-67.1847631435675,
175.490142808619));
#41479=CARTESIAN_POINT('Ctrl Pts',(-49.9327574595315,-67.2997349533242,
177.134243841043));
#41480=CARTESIAN_POINT('Ctrl Pts',(-50.9544351624631,-67.2850985130284,
178.441881219107));
#41481=CARTESIAN_POINT('Ctrl Pts',(-51.9761128653947,-67.2704620727326,
179.74951859717));
#41482=CARTESIAN_POINT('Ctrl Pts',(-53.6208882564639,-67.1893992560316,
179.954696079469));
#41483=CARTESIAN_POINT('Ctrl Pts',(-55.2656636475331,-67.1083364393306,
180.159873561769));
#41484=CARTESIAN_POINT('Ctrl Pts',(-56.5758711921821,-67.0629407902703,
179.142400961866));
#41485=CARTESIAN_POINT('Ctrl Pts',(-57.8860787368312,-67.0175451412101,
178.124928361964));
#41486=CARTESIAN_POINT('Ctrl Pts',(-58.1000382074012,-67.0890168607642,
176.48082732954));
#41487=CARTESIAN_POINT('Ctrl Pts',(-58.3139976779713,-67.1604885803183,
174.836726297116));
#41488=CARTESIAN_POINT('Ctrl Pts',(-57.3121961008737,-67.3615685499248,
173.529088919052));
#41489=CARTESIAN_POINT('Ctrl Pts',(-56.3103945237762,-67.5626485195312,
172.221451540989));
#41490=CARTESIAN_POINT('Ctrl Pts',(-54.685495258541,-67.830154865543,172.016274058689));
#41491=CARTESIAN_POINT('Ctrl Pts',(-53.0605959933058,-68.0976612115547,
171.81109657639));
#41492=CARTESIAN_POINT('Ctrl Pts',(-51.7702645744908,-68.3295003899256,
172.828569176292));
#41493=CARTESIAN_POINT('Ctrl Pts',(-50.4799331556759,-68.5613395682965,
173.846041776195));
#41494=CARTESIAN_POINT('Ctrl Pts',(-50.2858498109398,-68.6763113780532,
175.490142808619));
#41495=CARTESIAN_POINT('Ctrl Pts',(-50.0917664662038,-68.7912831878098,
177.134243841043));
#41496=CARTESIAN_POINT('Ctrl Pts',(-51.1134441691353,-68.776646747514,178.441881219107));
#41497=CARTESIAN_POINT('Ctrl Pts',(-52.1351218720669,-68.7620103072182,
179.74951859717));
#41498=CARTESIAN_POINT('Ctrl Pts',(-53.7798972631361,-68.6809474905172,
179.954696079469));
#41499=CARTESIAN_POINT('Ctrl Pts',(-55.4246726542053,-68.5998846738162,
180.159873561769));
#41500=CARTESIAN_POINT('Ctrl Pts',(-56.7348801988543,-68.5544890247559,
179.142400961866));
#41501=CARTESIAN_POINT('Ctrl Pts',(-58.0450877435034,-68.5090933756957,
178.124928361964));
#41502=CARTESIAN_POINT('Ctrl Pts',(-58.2590472140735,-68.5805650952498,
176.48082732954));
#41503=CARTESIAN_POINT('Ctrl Pts',(-58.4730066846436,-68.6520368148039,
174.836726297116));
#41504=CARTESIAN_POINT('Ctrl Pts',(-57.471205107546,-68.8531167844104,173.529088919052));
#41505=CARTESIAN_POINT('Ctrl Pts',(-56.4694035304484,-69.0541967540168,
172.221451540989));
#41506=CARTESIAN_POINT('Ctrl Pts',(-54.8445042652132,-69.3217031000286,
172.016274058689));
#41507=CARTESIAN_POINT('Ctrl Pts',(-53.2196049999781,-69.5892094460403,
171.81109657639));
#41508=CARTESIAN_POINT('Ctrl Pts',(-51.9292735811631,-69.8210486244112,
172.828569176292));
#41509=CARTESIAN_POINT('Ctrl Pts',(-50.6389421623481,-70.0528878027821,
173.846041776195));
#41510=CARTESIAN_POINT('Ctrl Pts',(-50.444858817612,-70.1678596125387,175.490142808619));
#41511=CARTESIAN_POINT('Ctrl Pts',(-50.250775472876,-70.2828314222954,177.134243841043));
#41512=CARTESIAN_POINT('Ctrl Pts',(-51.2724531758076,-70.2681949819996,
178.441881219107));
#41513=CARTESIAN_POINT('Ctrl Pts',(-52.2941308787392,-70.2535585417038,
179.74951859717));
#41514=CARTESIAN_POINT('Ctrl Pts',(-53.9389062698084,-70.1724957250028,
179.954696079469));
#41515=CARTESIAN_POINT('Ctrl Pts',(-55.5836816608776,-70.0914329083018,
180.159873561769));
#41516=CARTESIAN_POINT('Ctrl Pts',(-56.8938892055266,-70.0460372592415,
179.142400961866));
#41517=CARTESIAN_POINT('Ctrl Pts',(-58.2040967501756,-70.0006416101813,
178.124928361964));
#41518=CARTESIAN_POINT('Ctrl Pts',(-58.4180562207457,-70.0721133297354,
176.48082732954));
#41519=CARTESIAN_POINT('Ctrl Pts',(-58.6320156913158,-70.1435850492895,
174.836726297116));
#41520=CARTESIAN_POINT('Ctrl Pts',(-57.6302141142182,-70.344665018896,173.529088919052));
#41521=CARTESIAN_POINT('Ctrl Pts',(-56.6284125371206,-70.5457449885024,
172.221451540989));
#41522=CARTESIAN_POINT('Ctrl Pts',(-55.0035132718855,-70.8132513345142,
172.016274058689));
#41523=CARTESIAN_POINT('Ctrl Pts',(-53.3786140066503,-71.0807576805259,
171.81109657639));
#41524=CARTESIAN_POINT('Ctrl Pts',(-52.0882825878353,-71.3125968588968,
172.828569176292));
#41525=CARTESIAN_POINT('Ctrl Pts',(-50.7979511690203,-71.5444360372677,
173.846041776195));
#41526=CARTESIAN_POINT('Ctrl Pts',(-50.6038678242843,-71.6594078470244,
175.490142808619));
#41527=CARTESIAN_POINT('Ctrl Pts',(-50.4097844795482,-71.774379656781,177.134243841043));
#41528=CARTESIAN_POINT('Ctrl Pts',(-51.4314621824798,-71.7597432164852,
178.441881219107));
#41529=CARTESIAN_POINT('Ctrl Pts',(-52.4531398854114,-71.7451067761894,
179.74951859717));
#41530=CARTESIAN_POINT('Ctrl Pts',(-54.0979152764806,-71.6640439594884,
179.954696079469));
#41531=CARTESIAN_POINT('Ctrl Pts',(-55.7426906675498,-71.5829811427874,
180.159873561769));
#41532=CARTESIAN_POINT('Ctrl Pts',(-57.0528982121988,-71.5375854937271,
179.142400961866));
#41533=CARTESIAN_POINT('Ctrl Pts',(-58.3631057568478,-71.4921898446669,
178.124928361964));
#41534=CARTESIAN_POINT('Ctrl Pts',(-58.5770652274179,-71.563661564221,176.48082732954));
#41535=CARTESIAN_POINT('Ctrl Pts',(-58.791024697988,-71.6351332837751,174.836726297116));
#41536=CARTESIAN_POINT('Ctrl Pts',(-57.7892231208904,-71.8362132533815,
173.529088919052));
#41537=CARTESIAN_POINT('Ctrl Pts',(-56.7874215437929,-72.037293222988,172.221451540989));
#41538=CARTESIAN_POINT('Ctrl Pts',(-55.1625222785577,-72.3047995689997,
172.016274058689));
#41539=CARTESIAN_POINT('Ctrl Pts',(-53.5376230133225,-72.5723059150115,
171.81109657639));
#41540=CARTESIAN_POINT('Ctrl Pts',(-52.2472915945075,-72.8041450933824,
172.828569176292));
#41541=CARTESIAN_POINT('Ctrl Pts',(-50.9569601756925,-73.0359842717533,
173.846041776195));
#41542=CARTESIAN_POINT('Ctrl Pts',(-50.7628768309565,-73.1509560815099,
175.490142808619));
#41543=CARTESIAN_POINT('Ctrl Pts',(-50.5687934862204,-73.2659278912666,
177.134243841043));
#41544=CARTESIAN_POINT('Ctrl Pts',(-51.590471189152,-73.2512914509708,178.441881219107));
#41545=CARTESIAN_POINT('Ctrl Pts',(-52.6121488920836,-73.236655010675,179.74951859717));
#41546=CARTESIAN_POINT('Ctrl Pts',(-54.2569242831528,-73.155592193974,179.954696079469));
#41547=CARTESIAN_POINT('Ctrl Pts',(-55.901699674222,-73.074529377273,180.159873561769));
#41548=CARTESIAN_POINT('Ctrl Pts',(-57.211907218871,-73.0291337282128,179.142400961866));
#41549=CARTESIAN_POINT('Ctrl Pts',(-58.5221147635201,-72.9837380791525,
178.124928361964));
#41550=CARTESIAN_POINT('Ctrl Pts',(-58.7360742340901,-73.0552097987066,
176.48082732954));
#41551=CARTESIAN_POINT('Ctrl Pts',(-58.9500337046602,-73.1266815182607,
174.836726297116));
#41552=CARTESIAN_POINT('Ctrl Pts',(-57.9482321275626,-73.3277614878671,
173.529088919052));
#41553=CARTESIAN_POINT('Ctrl Pts',(-56.9464305504651,-73.5288414574736,
172.221451540989));
#41554=CARTESIAN_POINT('Ctrl Pts',(-55.3215312852299,-73.7963478034854,
172.016274058689));
#41555=CARTESIAN_POINT('Ctrl Pts',(-53.6966320199948,-74.0638541494971,
171.81109657639));
#41556=CARTESIAN_POINT('Ctrl Pts',(-52.4063006011798,-74.295693327868,172.828569176292));
#41557=CARTESIAN_POINT('Ctrl Pts',(-51.1159691823648,-74.5275325062389,
173.846041776195));
#41558=CARTESIAN_POINT('Ctrl Pts',(-50.9218858376287,-74.6425043159955,
175.490142808619));
#41559=CARTESIAN_POINT('Ctrl Pts',(-50.7278024928926,-74.7574761257522,
177.134243841043));
#41560=CARTESIAN_POINT('Ctrl Pts',(-51.7494801958242,-74.7428396854564,
178.441881219107));
#41561=CARTESIAN_POINT('Ctrl Pts',(-52.7711578987558,-74.7282032451606,
179.74951859717));
#41562=CARTESIAN_POINT('Ctrl Pts',(-54.415933289825,-74.6471404284596,179.954696079469));
#41563=CARTESIAN_POINT('Ctrl Pts',(-56.0607086808942,-74.5660776117586,
180.159873561769));
#41564=CARTESIAN_POINT('Ctrl Pts',(-57.3709162255433,-74.5206819626983,
179.142400961866));
#41565=CARTESIAN_POINT('Ctrl Pts',(-58.6811237701923,-74.4752863136381,
178.124928361964));
#41566=CARTESIAN_POINT('Ctrl Pts',(-58.8950832407624,-74.5467580331922,
176.48082732954));
#41567=CARTESIAN_POINT('Ctrl Pts',(-59.1090427113324,-74.6182297527463,
174.836726297116));
#41568=CARTESIAN_POINT('Ctrl Pts',(-58.1072411342349,-74.8193097223528,
173.529088919052));
#41569=CARTESIAN_POINT('Ctrl Pts',(-57.1054395571373,-75.0203896919592,
172.221451540989));
#41570=CARTESIAN_POINT('Ctrl Pts',(-55.4805402919021,-75.287896037971,172.016274058689));
#41571=CARTESIAN_POINT('Ctrl Pts',(-53.855641026667,-75.5554023839827,171.81109657639));
#41572=CARTESIAN_POINT('Ctrl Pts',(-52.565309607852,-75.7872415623536,172.828569176292));
#41573=CARTESIAN_POINT('Ctrl Pts',(-51.274978189037,-76.0190807407245,173.846041776195));
#41574=CARTESIAN_POINT('Ctrl Pts',(-51.0808948443009,-76.1340525504811,
175.490142808619));
#41575=CARTESIAN_POINT('Ctrl Pts',(-50.8868114995649,-76.2490243602377,
177.134243841043));
#41576=CARTESIAN_POINT('Ctrl Pts',(-51.9084892024965,-76.234387919942,178.441881219107));
#41577=CARTESIAN_POINT('Ctrl Pts',(-52.9301669054281,-76.2197514796462,
179.74951859717));
#41578=CARTESIAN_POINT('Ctrl Pts',(-54.5749422964973,-76.1386886629452,
179.954696079469));
#41579=CARTESIAN_POINT('Ctrl Pts',(-56.2197176875665,-76.0576258462442,
180.159873561769));
#41580=CARTESIAN_POINT('Ctrl Pts',(-57.5299252322155,-76.012230197184,179.142400961866));
#41581=CARTESIAN_POINT('Ctrl Pts',(-58.8401327768645,-75.9668345481237,
178.124928361964));
#41582=CARTESIAN_POINT('Ctrl Pts',(-59.0540922474346,-76.0383062676778,
176.48082732954));
#41583=CARTESIAN_POINT('Ctrl Pts',(-59.2680517180047,-76.1097779872319,
174.836726297116));
#41584=CARTESIAN_POINT('Ctrl Pts',(-58.2662501409071,-76.3108579568383,
173.529088919052));
#41585=CARTESIAN_POINT('Ctrl Pts',(-57.2644485638095,-76.5119379264448,
172.221451540989));
#41586=CARTESIAN_POINT('Ctrl Pts',(-55.6395492985744,-76.7794442724566,
172.016274058689));
#41587=CARTESIAN_POINT('Ctrl Pts',(-54.0146500333392,-77.0469506184683,
171.81109657639));
#41588=CARTESIAN_POINT('Ctrl Pts',(-52.7243186145242,-77.2787897968392,
172.828569176292));
#41589=CARTESIAN_POINT('Ctrl Pts',(-51.4339871957092,-77.5106289752101,
173.846041776195));
#41590=CARTESIAN_POINT('Ctrl Pts',(-51.2399038509732,-77.6256007849667,
175.490142808619));
#41591=CARTESIAN_POINT('Ctrl Pts',(-51.0458205062371,-77.7405725947234,
177.134243841043));
#41592=CARTESIAN_POINT('Ctrl Pts',(-52.0674982091687,-77.7259361544276,
178.441881219107));
#41593=CARTESIAN_POINT('Ctrl Pts',(-53.0891759121003,-77.7112997141318,
179.74951859717));
#41594=CARTESIAN_POINT('Ctrl Pts',(-54.7339513031695,-77.6302368974308,
179.954696079469));
#41595=CARTESIAN_POINT('Ctrl Pts',(-56.3787266942387,-77.5491740807298,
180.159873561769));
#41596=CARTESIAN_POINT('Ctrl Pts',(-57.6889342388877,-77.5037784316696,
179.142400961866));
#41597=CARTESIAN_POINT('Ctrl Pts',(-58.9991417835367,-77.4583827826093,
178.124928361964));
#41598=CARTESIAN_POINT('Ctrl Pts',(-59.2131012541068,-77.5298545021634,
176.48082732954));
#41599=CARTESIAN_POINT('Ctrl Pts',(-59.4270607246769,-77.6013262217175,
174.836726297116));
#41600=CARTESIAN_POINT('Ctrl Pts',(-58.4252591475793,-77.802406191324,173.529088919052));
#41601=CARTESIAN_POINT('Ctrl Pts',(-57.4234575704818,-78.0034861609304,
172.221451540989));
#41602=CARTESIAN_POINT('Ctrl Pts',(-55.7985583052466,-78.2709925069422,
172.016274058689));
#41603=CARTESIAN_POINT('Ctrl Pts',(-54.1736590400114,-78.5384988529539,
171.81109657639));
#41604=CARTESIAN_POINT('Ctrl Pts',(-52.8833276211964,-78.7703380313248,
172.828569176292));
#41605=CARTESIAN_POINT('Ctrl Pts',(-51.5929962023814,-79.0021772096957,
173.846041776195));
#41606=CARTESIAN_POINT('Ctrl Pts',(-51.3989128576454,-79.1171490194523,
175.490142808619));
#41607=CARTESIAN_POINT('Ctrl Pts',(-51.2048295129093,-79.232120829209,177.134243841043));
#41608=CARTESIAN_POINT('Ctrl Pts',(-52.2265072158409,-79.2174843889132,
178.441881219107));
#41609=CARTESIAN_POINT('Ctrl Pts',(-53.2481849187725,-79.2028479486174,
179.74951859717));
#41610=CARTESIAN_POINT('Ctrl Pts',(-54.8929603098417,-79.1217851319164,
179.954696079469));
#41611=CARTESIAN_POINT('Ctrl Pts',(-56.5377357009109,-79.0407223152154,
180.159873561769));
#41612=CARTESIAN_POINT('Ctrl Pts',(-57.8479432455599,-78.9953266661552,
179.142400961866));
#41613=CARTESIAN_POINT('Ctrl Pts',(-59.158150790209,-78.9499310170949,178.124928361964));
#41614=CARTESIAN_POINT('Ctrl Pts',(-59.372110260779,-79.021402736649,176.48082732954));
#41615=CARTESIAN_POINT('Ctrl Pts',(-59.5860697313491,-79.0928744562031,
174.836726297116));
#41616=CARTESIAN_POINT('Ctrl Pts',(-58.5842681542516,-79.2939544258096,
173.529088919052));
#41617=CARTESIAN_POINT('Ctrl Pts',(-57.582466577154,-79.495034395416,172.221451540989));
#41618=CARTESIAN_POINT('Ctrl Pts',(-55.9575673119188,-79.7625407414277,
172.016274058689));
#41619=CARTESIAN_POINT('Ctrl Pts',(-54.3326680466837,-80.0300470874395,
171.81109657639));
#41620=CARTESIAN_POINT('Ctrl Pts',(-53.0423366278687,-80.2618862658104,
172.828569176292));
#41621=CARTESIAN_POINT('Ctrl Pts',(-51.7520052090537,-80.4937254441813,
173.846041776195));
#41622=CARTESIAN_POINT('Ctrl Pts',(-51.5579218643176,-80.6086972539379,
175.490142808619));
#41623=CARTESIAN_POINT('Ctrl Pts',(-51.3638385195816,-80.7236690636945,
177.134243841043));
#41624=CARTESIAN_POINT('Ctrl Pts',(-52.3855162225132,-80.7090326233988,
178.441881219107));
#41625=CARTESIAN_POINT('Ctrl Pts',(-53.4071939254448,-80.694396183103,179.74951859717));
#41626=CARTESIAN_POINT('Ctrl Pts',(-55.0519693165139,-80.613333366402,179.954696079469));
#41627=CARTESIAN_POINT('Ctrl Pts',(-56.6967447075831,-80.532270549701,180.159873561769));
#41628=CARTESIAN_POINT('Ctrl Pts',(-58.0069522522322,-80.4868749006407,
179.142400961866));
#41629=CARTESIAN_POINT('Ctrl Pts',(-59.3171597968812,-80.4414792515805,
178.124928361964));
#41630=CARTESIAN_POINT('Ctrl Pts',(-59.5311192674513,-80.5129509711346,
176.48082732954));
#41631=CARTESIAN_POINT('Ctrl Pts',(-59.7450787380214,-80.5844226906887,
174.836726297116));
#41632=CARTESIAN_POINT('Ctrl Pts',(-58.7432771609238,-80.7855026602952,
173.529088919052));
#41633=CARTESIAN_POINT('Ctrl Pts',(-57.7414755838262,-80.9865826299016,
172.221451540989));
#41634=CARTESIAN_POINT('Ctrl Pts',(-56.116576318591,-81.2540889759133,172.016274058689));
#41635=CARTESIAN_POINT('Ctrl Pts',(-54.4916770533559,-81.5215953219251,
171.81109657639));
#41636=CARTESIAN_POINT('Ctrl Pts',(-53.2013456345409,-81.753434500296,172.828569176292));
#41637=CARTESIAN_POINT('Ctrl Pts',(-51.9110142157259,-81.9852736786669,
173.846041776195));
#41638=CARTESIAN_POINT('Ctrl Pts',(-51.7169308709898,-82.1002454884235,
175.490142808619));
#41639=CARTESIAN_POINT('Ctrl Pts',(-51.5228475262538,-82.2152172981802,
177.134243841043));
#41640=CARTESIAN_POINT('Ctrl Pts',(-52.5445252291854,-82.2005808578844,
178.441881219107));
#41641=CARTESIAN_POINT('Ctrl Pts',(-53.566202932117,-82.1859444175886,179.74951859717));
#41642=CARTESIAN_POINT('Ctrl Pts',(-55.2109783231862,-82.1048816008876,
179.954696079469));
#41643=CARTESIAN_POINT('Ctrl Pts',(-56.8557537142554,-82.0238187841866,
180.159873561769));
#41644=CARTESIAN_POINT('Ctrl Pts',(-58.1659612589044,-81.9784231351264,
179.142400961866));
#41645=CARTESIAN_POINT('Ctrl Pts',(-59.4761688035534,-81.9330274860661,
178.124928361964));
#41646=CARTESIAN_POINT('Ctrl Pts',(-59.6901282741235,-82.0044992056202,
176.48082732954));
#41647=CARTESIAN_POINT('Ctrl Pts',(-59.9040877446936,-82.0759709251743,
174.836726297116));
#41648=CARTESIAN_POINT('Ctrl Pts',(-58.902286167596,-82.2770508947808,173.529088919052));
#41649=CARTESIAN_POINT('Ctrl Pts',(-57.9004845904984,-82.4781308643872,
172.221451540989));
#41650=CARTESIAN_POINT('Ctrl Pts',(-56.2755853252633,-82.745637210399,172.016274058689));
#41651=CARTESIAN_POINT('Ctrl Pts',(-54.6506860600281,-83.0131435564107,
171.81109657639));
#41652=CARTESIAN_POINT('Ctrl Pts',(-53.3603546412131,-83.2449827347816,
172.828569176292));
#41653=CARTESIAN_POINT('Ctrl Pts',(-52.0700232223981,-83.4768219131525,
173.846041776195));
#41654=CARTESIAN_POINT('Ctrl Pts',(-51.8759398776621,-83.5917937229092,
175.490142808619));
#41655=CARTESIAN_POINT('Ctrl Pts',(-51.681856532926,-83.7067655326658,177.134243841043));
#41656=CARTESIAN_POINT('Ctrl Pts',(-52.7035342358576,-83.69212909237,178.441881219107));
#41657=CARTESIAN_POINT('Ctrl Pts',(-53.7252119387892,-83.6774926520742,
179.74951859717));
#41658=CARTESIAN_POINT('Ctrl Pts',(-55.3699873298584,-83.5964298353732,
179.954696079469));
#41659=CARTESIAN_POINT('Ctrl Pts',(-57.0147627209276,-83.5153670186722,
180.159873561769));
#41660=CARTESIAN_POINT('Ctrl Pts',(-58.3249702655766,-83.469971369612,179.142400961866));
#41661=CARTESIAN_POINT('Ctrl Pts',(-59.6351778102256,-83.4245757205517,
178.124928361964));
#41662=CARTESIAN_POINT('Ctrl Pts',(-59.8491372807957,-83.4960474401058,
176.48082732954));
#41663=CARTESIAN_POINT('Ctrl Pts',(-60.0630967513658,-83.5675191596599,
174.836726297116));
#41664=CARTESIAN_POINT('Ctrl Pts',(-59.0612951742682,-83.7685991292663,
173.529088919052));
#41665=CARTESIAN_POINT('Ctrl Pts',(-58.0594935971707,-83.9696790988728,
172.221451540989));
#41666=CARTESIAN_POINT('Ctrl Pts',(-56.4345943319355,-84.2371854448845,
172.016274058689));
#41667=CARTESIAN_POINT('Ctrl Pts',(-54.8096950667003,-84.5046917908963,
171.81109657639));
#41668=CARTESIAN_POINT('Ctrl Pts',(-53.5193636478853,-84.7365309692672,
172.828569176292));
#41669=CARTESIAN_POINT('Ctrl Pts',(-52.2290322290704,-84.9683701476381,
173.846041776195));
#41670=CARTESIAN_POINT('Ctrl Pts',(-52.0349488843343,-85.0833419573947,
175.490142808619));
#41671=CARTESIAN_POINT('Ctrl Pts',(-51.8408655395982,-85.1983137671514,
177.134243841043));
#41672=CARTESIAN_POINT('Ctrl Pts',(-52.8625432425298,-85.1836773268556,
178.441881219107));
#41673=CARTESIAN_POINT('Ctrl Pts',(-53.8842209454614,-85.1690408865598,
179.74951859717));
#41674=CARTESIAN_POINT('Ctrl Pts',(-55.5289963365306,-85.0879780698588,
179.954696079469));
#41675=CARTESIAN_POINT('Ctrl Pts',(-57.1737717275998,-85.0069152531578,
180.159873561769));
#41676=CARTESIAN_POINT('Ctrl Pts',(-58.4839792722488,-84.9615196040975,
179.142400961866));
#41677=CARTESIAN_POINT('Ctrl Pts',(-59.7941868168979,-84.9161239550373,
178.124928361964));
#41678=CARTESIAN_POINT('Ctrl Pts',(-60.008146287468,-84.9875956745914,176.48082732954));
#41679=CARTESIAN_POINT('Ctrl Pts',(-60.222105758038,-85.0590673941455,174.836726297116));
#41680=CARTESIAN_POINT('Ctrl Pts',(-59.2203041809405,-85.260147363752,173.529088919052));
#41681=CARTESIAN_POINT('Ctrl Pts',(-58.2185026038429,-85.4612273333584,
172.221451540989));
#41682=CARTESIAN_POINT('Ctrl Pts',(-56.5936033386077,-85.7287336793702,
172.016274058689));
#41683=CARTESIAN_POINT('Ctrl Pts',(-54.9687040733726,-85.9962400253819,
171.81109657639));
#41684=CARTESIAN_POINT('Ctrl Pts',(-53.6783726545576,-86.2280792037528,
172.828569176292));
#41685=CARTESIAN_POINT('Ctrl Pts',(-52.3880412357426,-86.4599183821237,
173.846041776195));
#41686=CARTESIAN_POINT('Ctrl Pts',(-52.1939578910065,-86.5748901918803,
175.490142808619));
#41687=CARTESIAN_POINT('Ctrl Pts',(-51.9998745462705,-86.689862001637,177.134243841043));
#41688=CARTESIAN_POINT('Ctrl Pts',(-53.0215522492021,-86.6752255613412,
178.441881219107));
#41689=CARTESIAN_POINT('Ctrl Pts',(-54.0432299521337,-86.6605891210454,
179.74951859717));
#41690=CARTESIAN_POINT('Ctrl Pts',(-55.6880053432029,-86.5795263043444,
179.954696079469));
#41691=CARTESIAN_POINT('Ctrl Pts',(-57.332780734272,-86.4984634876434,180.159873561769));
#41692=CARTESIAN_POINT('Ctrl Pts',(-58.6429882789211,-86.4530678385832,
179.142400961866));
#41693=CARTESIAN_POINT('Ctrl Pts',(-59.9531958235701,-86.4076721895229,
178.124928361964));
#41694=CARTESIAN_POINT('Ctrl Pts',(-60.1671552941402,-86.479143909077,176.48082732954));
#41695=CARTESIAN_POINT('Ctrl Pts',(-60.3811147647103,-86.5506156286311,
174.836726297116));
#41696=CARTESIAN_POINT('Ctrl Pts',(-59.3793131876127,-86.7516955982376,
173.529088919052));
#41697=CARTESIAN_POINT('Ctrl Pts',(-58.3775116105151,-86.952775567844,172.221451540989));
#41698=CARTESIAN_POINT('Ctrl Pts',(-56.7526123452799,-87.2202819138558,
172.016274058689));
#41699=CARTESIAN_POINT('Ctrl Pts',(-55.1277130800448,-87.4877882598675,
171.81109657639));
#41700=CARTESIAN_POINT('Ctrl Pts',(-53.8373816612298,-87.7196274382384,
172.828569176292));
#41701=CARTESIAN_POINT('Ctrl Pts',(-52.5470502424148,-87.9514666166093,
173.846041776195));
#41702=CARTESIAN_POINT('Ctrl Pts',(-52.3529668976787,-88.0664384263659,
175.490142808619));
#41703=CARTESIAN_POINT('Ctrl Pts',(-52.1588835529427,-88.1814102361226,
177.134243841043));
#41704=CARTESIAN_POINT('Ctrl Pts',(-53.1805612558743,-88.1667737958268,
178.441881219107));
#41705=CARTESIAN_POINT('Ctrl Pts',(-54.2022389588059,-88.152137355531,179.74951859717));
#41706=CARTESIAN_POINT('Ctrl Pts',(-55.8470143498751,-88.07107453883,179.954696079469));
#41707=CARTESIAN_POINT('Ctrl Pts',(-57.4917897409443,-87.990011722129,180.159873561769));
#41708=CARTESIAN_POINT('Ctrl Pts',(-58.8019972855933,-87.9446160730687,
179.142400961866));
#41709=CARTESIAN_POINT('Ctrl Pts',(-60.1122048302423,-87.8992204240085,
178.124928361964));
#41710=CARTESIAN_POINT('Ctrl Pts',(-60.3261643008124,-87.9706921435626,
176.48082732954));
#41711=CARTESIAN_POINT('Ctrl Pts',(-60.5401237713825,-88.0421638631167,
174.836726297116));
#41712=CARTESIAN_POINT('Ctrl Pts',(-59.5383221942849,-88.2432438327232,
173.529088919052));
#41713=CARTESIAN_POINT('Ctrl Pts',(-58.5365206171873,-88.4443238023296,
172.221451540989));
#41714=CARTESIAN_POINT('Ctrl Pts',(-56.9116213519522,-88.7118301483414,
172.016274058689));
#41715=CARTESIAN_POINT('Ctrl Pts',(-55.286722086717,-88.9793364943531,171.81109657639));
#41716=CARTESIAN_POINT('Ctrl Pts',(-53.996390667902,-89.211175672724,172.828569176292));
#41717=CARTESIAN_POINT('Ctrl Pts',(-52.706059249087,-89.4430148510949,173.846041776195));
#41718=CARTESIAN_POINT('Ctrl Pts',(-52.511975904351,-89.5579866608516,175.490142808619));
#41719=CARTESIAN_POINT('Ctrl Pts',(-52.3178925596149,-89.6729584706082,
177.134243841043));
#41720=CARTESIAN_POINT('Ctrl Pts',(-53.3395702625465,-89.6583220303124,
178.441881219107));
#41721=CARTESIAN_POINT('Ctrl Pts',(-54.3612479654781,-89.6436855900166,
179.74951859717));
#41722=CARTESIAN_POINT('Ctrl Pts',(-56.0060233565473,-89.5626227733156,
179.954696079469));
#41723=CARTESIAN_POINT('Ctrl Pts',(-57.6507987476165,-89.4815599566146,
180.159873561769));
#41724=CARTESIAN_POINT('Ctrl Pts',(-58.9610062922655,-89.4361643075543,
179.142400961866));
#41725=CARTESIAN_POINT('Ctrl Pts',(-60.2712138369146,-89.3907686584941,
178.124928361964));
#41726=CARTESIAN_POINT('Ctrl Pts',(-60.4851733074846,-89.4622403780482,
176.48082732954));
#41727=CARTESIAN_POINT('Ctrl Pts',(-60.6991327780547,-89.5337120976023,
174.836726297116));
#41728=CARTESIAN_POINT('Ctrl Pts',(-59.6973312009571,-89.7347920672087,
173.529088919052));
#41729=CARTESIAN_POINT('Ctrl Pts',(-58.6955296238596,-89.9358720368152,
172.221451540989));
#41730=CARTESIAN_POINT('Ctrl Pts',(-57.0706303586244,-90.203378382827,172.016274058689));
#41731=CARTESIAN_POINT('Ctrl Pts',(-55.4457310933893,-90.4708847288387,
171.81109657639));
#41732=CARTESIAN_POINT('Ctrl Pts',(-54.1553996745743,-90.7027239072096,
172.828569176292));
#41733=CARTESIAN_POINT('Ctrl Pts',(-52.8650682557593,-90.9345630855805,
173.846041776195));
#41734=CARTESIAN_POINT('Ctrl Pts',(-52.6709849110232,-91.0495348953371,
175.490142808619));
#41735=CARTESIAN_POINT('Ctrl Pts',(-52.4769015662871,-91.1645067050937,
177.134243841043));
#41736=CARTESIAN_POINT('Ctrl Pts',(-53.4985792692187,-91.149870264798,178.441881219107));
#41737=CARTESIAN_POINT('Ctrl Pts',(-54.5202569721503,-91.1352338245022,
179.74951859717));
#41738=CARTESIAN_POINT('Ctrl Pts',(-56.1650323632195,-91.0541710078012,
179.954696079469));
#41739=CARTESIAN_POINT('Ctrl Pts',(-57.8098077542887,-90.9731081911002,
180.159873561769));
#41740=CARTESIAN_POINT('Ctrl Pts',(-59.1200152989378,-90.92771254204,179.142400961866));
#41741=CARTESIAN_POINT('Ctrl Pts',(-60.4302228435868,-90.8823168929797,
178.124928361964));
#41742=CARTESIAN_POINT('Ctrl Pts',(-60.6441823141569,-90.9537886125338,
176.48082732954));
#41743=CARTESIAN_POINT('Ctrl Pts',(-60.858141784727,-91.0252603320879,174.836726297116));
#41744=CARTESIAN_POINT('Ctrl Pts',(-59.8563402076294,-91.2263403016943,
173.529088919052));
#41745=CARTESIAN_POINT('Ctrl Pts',(-58.8545386305318,-91.4274202713008,
172.221451540989));
#41746=CARTESIAN_POINT('Ctrl Pts',(-57.2296393652966,-91.6949266173126,
172.016274058689));
#41747=CARTESIAN_POINT('Ctrl Pts',(-55.6047401000615,-91.9624329633243,
171.81109657639));
#41748=CARTESIAN_POINT('Ctrl Pts',(-54.3144086812465,-92.1942721416952,
172.828569176292));
#41749=CARTESIAN_POINT('Ctrl Pts',(-53.0240772624315,-92.4261113200661,
173.846041776195));
#41750=CARTESIAN_POINT('Ctrl Pts',(-52.8299939176954,-92.5410831298227,
175.490142808619));
#41751=CARTESIAN_POINT('Ctrl Pts',(-52.6359105729594,-92.6560549395794,
177.134243841043));
#41752=CARTESIAN_POINT('Ctrl Pts',(-53.657588275891,-92.6414184992836,178.441881219107));
#41753=CARTESIAN_POINT('Ctrl Pts',(-54.6792659788226,-92.6267820589878,
179.74951859717));
#41754=CARTESIAN_POINT('Ctrl Pts',(-56.3240413698918,-92.5457192422868,
179.954696079469));
#41755=CARTESIAN_POINT('Ctrl Pts',(-57.968816760961,-92.4646564255858,180.159873561769));
#41756=CARTESIAN_POINT('Ctrl Pts',(-59.27902430561,-92.4192607765256,179.142400961866));
#41757=CARTESIAN_POINT('Ctrl Pts',(-60.589231850259,-92.3738651274653,178.124928361964));
#41758=CARTESIAN_POINT('Ctrl Pts',(-60.8031913208291,-92.4453368470194,
176.48082732954));
#41759=CARTESIAN_POINT('Ctrl Pts',(-61.0171507913992,-92.5168085665735,
174.836726297116));
#41760=CARTESIAN_POINT('Ctrl Pts',(-60.0153492143016,-92.71788853618,173.529088919052));
#41761=CARTESIAN_POINT('Ctrl Pts',(-59.013547637204,-92.9189685057864,172.221451540989));
#41762=CARTESIAN_POINT('Ctrl Pts',(-57.3886483719689,-93.1864748517982,
172.016274058689));
#41763=CARTESIAN_POINT('Ctrl Pts',(-55.7637491067337,-93.4539811978099,
171.81109657639));
#41764=CARTESIAN_POINT('Ctrl Pts',(-54.4734176879187,-93.6858203761808,
172.828569176292));
#41765=CARTESIAN_POINT('Ctrl Pts',(-53.1830862691037,-93.9176595545517,
173.846041776195));
#41766=CARTESIAN_POINT('Ctrl Pts',(-52.9890029243677,-94.0326313643084,
175.490142808619));
#41767=CARTESIAN_POINT('Ctrl Pts',(-52.7949195796316,-94.147603174065,177.134243841043));
#41768=CARTESIAN_POINT('Ctrl Pts',(-53.8165972825632,-94.1329667337692,
178.441881219107));
#41769=CARTESIAN_POINT('Ctrl Pts',(-54.8382749854948,-94.1183302934734,
179.74951859717));
#41770=CARTESIAN_POINT('Ctrl Pts',(-56.483050376564,-94.0372674767724,179.954696079469));
#41771=CARTESIAN_POINT('Ctrl Pts',(-58.1278257676332,-93.9562046600714,
180.159873561769));
#41772=CARTESIAN_POINT('Ctrl Pts',(-59.4380333122822,-93.9108090110112,
179.142400961866));
#41773=CARTESIAN_POINT('Ctrl Pts',(-60.7482408569312,-93.8654133619509,
178.124928361964));
#41774=CARTESIAN_POINT('Ctrl Pts',(-60.9622003275013,-93.936885081505,176.48082732954));
#41775=CARTESIAN_POINT('Ctrl Pts',(-61.1761597980714,-94.0083568010591,
174.836726297116));
#41776=CARTESIAN_POINT('Ctrl Pts',(-60.1743582209738,-94.2094367706656,
173.529088919052));
#41777=CARTESIAN_POINT('Ctrl Pts',(-59.1725566438763,-94.410516740272,172.221451540989));
#41778=CARTESIAN_POINT('Ctrl Pts',(-57.5476573786411,-94.6780230862838,
172.016274058689));
#41779=CARTESIAN_POINT('Ctrl Pts',(-55.9227581134059,-94.9455294322955,
171.81109657639));
#41780=CARTESIAN_POINT('Ctrl Pts',(-54.6324266945909,-95.1773686106664,
172.828569176292));
#41781=CARTESIAN_POINT('Ctrl Pts',(-53.342095275776,-95.4092077890373,173.846041776195));
#41782=CARTESIAN_POINT('Ctrl Pts',(-53.1480119310399,-95.5241795987939,
175.490142808619));
#41783=CARTESIAN_POINT('Ctrl Pts',(-52.9539285863038,-95.6391514085506,
177.134243841043));
#41784=CARTESIAN_POINT('Ctrl Pts',(-53.9756062892354,-95.6245149682548,
178.441881219107));
#41785=CARTESIAN_POINT('Ctrl Pts',(-54.997283992167,-95.609878527959,179.74951859717));
#41786=CARTESIAN_POINT('Ctrl Pts',(-56.6420593832362,-95.528815711258,179.954696079469));
#41787=CARTESIAN_POINT('Ctrl Pts',(-58.2868347743054,-95.447752894557,180.159873561769));
#41788=CARTESIAN_POINT('Ctrl Pts',(-59.5970423189544,-95.4023572454968,
179.142400961866));
#41789=CARTESIAN_POINT('Ctrl Pts',(-60.9072498636035,-95.3569615964365,
178.124928361964));
#41790=CARTESIAN_POINT('Ctrl Pts',(-61.1212093341735,-95.4284333159906,
176.48082732954));
#41791=CARTESIAN_POINT('Ctrl Pts',(-61.3351688047436,-95.4999050355447,
174.836726297116));
#41792=CARTESIAN_POINT('Ctrl Pts',(-60.3333672276461,-95.7009850051512,
173.529088919052));
#41793=CARTESIAN_POINT('Ctrl Pts',(-59.3315656505485,-95.9020649747577,
172.221451540989));
#41794=CARTESIAN_POINT('Ctrl Pts',(-57.7066663853133,-96.1695713207694,
172.016274058689));
#41795=CARTESIAN_POINT('Ctrl Pts',(-56.0817671200782,-96.4370776667811,
171.81109657639));
#41796=CARTESIAN_POINT('Ctrl Pts',(-54.7914357012632,-96.668916845152,172.828569176292));
#41797=CARTESIAN_POINT('Ctrl Pts',(-53.5011042824482,-96.9007560235229,
173.846041776195));
#41798=CARTESIAN_POINT('Ctrl Pts',(-53.3070209377121,-97.0157278332795,
175.490142808619));
#41799=CARTESIAN_POINT('Ctrl Pts',(-53.1129375929761,-97.1306996430362,
177.134243841043));
#41800=CARTESIAN_POINT('Ctrl Pts',(-54.1346152959077,-97.1160632027404,
178.441881219107));
#41801=CARTESIAN_POINT('Ctrl Pts',(-55.1562929988393,-97.1014267624446,
179.74951859717));
#41802=CARTESIAN_POINT('Ctrl Pts',(-56.8010683899085,-97.0203639457436,
179.954696079469));
#41803=CARTESIAN_POINT('Ctrl Pts',(-58.4458437809776,-96.9393011290426,
180.159873561769));
#41804=CARTESIAN_POINT('Ctrl Pts',(-59.7560513256267,-96.8939054799824,
179.142400961866));
#41805=CARTESIAN_POINT('Ctrl Pts',(-61.0662588702757,-96.8485098309221,
178.124928361964));
#41806=CARTESIAN_POINT('Ctrl Pts',(-61.2802183408458,-96.9199815504762,
176.48082732954));
#41807=CARTESIAN_POINT('Ctrl Pts',(-61.4941778114159,-96.9914532700303,
174.836726297116));
#41808=CARTESIAN_POINT('Ctrl Pts',(-60.4923762343183,-97.1925332396368,
173.529088919052));
#41809=CARTESIAN_POINT('Ctrl Pts',(-59.4905746572207,-97.3936132092432,
172.221451540989));
#41810=CARTESIAN_POINT('Ctrl Pts',(-57.8656753919855,-97.661119555255,172.016274058689));
#41811=CARTESIAN_POINT('Ctrl Pts',(-56.2407761267504,-97.9286259012667,
171.81109657639));
#41812=CARTESIAN_POINT('Ctrl Pts',(-54.9504447079354,-98.1604650796376,
172.828569176292));
#41813=CARTESIAN_POINT('Ctrl Pts',(-53.6601132891204,-98.3923042580085,
173.846041776195));
#41814=CARTESIAN_POINT('Ctrl Pts',(-53.4660299443843,-98.5072760677652,
175.490142808619));
#41815=CARTESIAN_POINT('Ctrl Pts',(-53.2719465996483,-98.6222478775218,
177.134243841043));
#41816=CARTESIAN_POINT('Ctrl Pts',(-54.2936243025799,-98.607611437226,178.441881219107));
#41817=CARTESIAN_POINT('Ctrl Pts',(-55.3153020055115,-98.5929749969302,
179.74951859717));
#41818=CARTESIAN_POINT('Ctrl Pts',(-56.9600773965807,-98.5119121802292,
179.954696079469));
#41819=CARTESIAN_POINT('Ctrl Pts',(-58.6048527876499,-98.4308493635282,
180.159873561769));
#41820=CARTESIAN_POINT('Ctrl Pts',(-59.9150603322989,-98.385453714468,179.142400961866));
#41821=CARTESIAN_POINT('Ctrl Pts',(-61.2252678769479,-98.3400580654077,
178.124928361964));
#41822=CARTESIAN_POINT('Ctrl Pts',(-61.439227347518,-98.4115297849618,176.48082732954));
#41823=CARTESIAN_POINT('Ctrl Pts',(-61.6531868180881,-98.4830015045159,
174.836726297116));
#41824=CARTESIAN_POINT('Ctrl Pts',(-60.6513852409905,-98.6840814741224,
173.529088919052));
#41825=CARTESIAN_POINT('Ctrl Pts',(-59.6495836638929,-98.8851614437288,
172.221451540989));
#41826=CARTESIAN_POINT('Ctrl Pts',(-58.0246843986578,-99.1526677897406,
172.016274058689));
#41827=CARTESIAN_POINT('Ctrl Pts',(-56.3997851334226,-99.4201741357523,
171.81109657639));
#41828=CARTESIAN_POINT('Ctrl Pts',(-55.1094537146076,-99.6520133141232,
172.828569176292));
#41829=CARTESIAN_POINT('Ctrl Pts',(-53.8191222957926,-99.8838524924941,
173.846041776195));
#41830=CARTESIAN_POINT('Ctrl Pts',(-53.6250389510566,-99.9988243022507,
175.490142808619));
#41831=CARTESIAN_POINT('Ctrl Pts',(-53.4309556063205,-100.113796112007,
177.134243841043));
#41832=CARTESIAN_POINT('Ctrl Pts',(-54.4526333092521,-100.099159671712,
178.441881219107));
#41833=CARTESIAN_POINT('Ctrl Pts',(-55.4743110121837,-100.084523231416,
179.74951859717));
#41834=CARTESIAN_POINT('Ctrl Pts',(-57.1190864032529,-100.003460414715,
179.954696079469));
#41835=CARTESIAN_POINT('Ctrl Pts',(-58.7638617943221,-99.9223975980138,
180.159873561769));
#41836=CARTESIAN_POINT('Ctrl Pts',(-60.0740693389711,-99.8770019489536,
179.142400961866));
#41837=CARTESIAN_POINT('Ctrl Pts',(-61.3842768836201,-99.8316062998934,
178.124928361964));
#41838=CARTESIAN_POINT('Ctrl Pts',(-61.5982363541902,-99.9030780194474,
176.48082732954));
#41839=CARTESIAN_POINT('Ctrl Pts',(-61.8121958247603,-99.9745497390015,
174.836726297116));
#41840=CARTESIAN_POINT('Ctrl Pts',(-60.8103942476627,-100.175629708608,
173.529088919052));
#41841=CARTESIAN_POINT('Ctrl Pts',(-59.8085926705652,-100.376709678214,
172.221451540989));
#41842=CARTESIAN_POINT('Ctrl Pts',(-58.18369340533,-100.644216024226,172.016274058689));
#41843=CARTESIAN_POINT('Ctrl Pts',(-56.5587941400948,-100.911722370238,
171.81109657639));
#41844=CARTESIAN_POINT('Ctrl Pts',(-55.2684627212798,-101.143561548609,
172.828569176292));
#41845=CARTESIAN_POINT('Ctrl Pts',(-53.9781313024648,-101.37540072698,173.846041776195));
#41846=CARTESIAN_POINT('Ctrl Pts',(-53.7840479577288,-101.490372536736,
175.490142808619));
#41847=CARTESIAN_POINT('Ctrl Pts',(-53.5899646129927,-101.605344346493,
177.134243841043));
#41848=CARTESIAN_POINT('Ctrl Pts',(-54.6116423159243,-101.590707906197,
178.441881219107));
#41849=CARTESIAN_POINT('Ctrl Pts',(-55.6333200188559,-101.576071465901,
179.74951859717));
#41850=CARTESIAN_POINT('Ctrl Pts',(-57.2780954099251,-101.4950086492,179.954696079469));
#41851=CARTESIAN_POINT('Ctrl Pts',(-58.9228708009943,-101.413945832499,
180.159873561769));
#41852=CARTESIAN_POINT('Ctrl Pts',(-60.2330783456433,-101.368550183439,
179.142400961866));
#41853=CARTESIAN_POINT('Ctrl Pts',(-61.5432858902924,-101.323154534379,
178.124928361964));
#41854=CARTESIAN_POINT('Ctrl Pts',(-61.7572453608625,-101.394626253933,
176.48082732954));
#41855=CARTESIAN_POINT('Ctrl Pts',(-61.9712048314326,-101.466097973487,
174.836726297116));
#41856=CARTESIAN_POINT('Ctrl Pts',(-60.969403254335,-101.667177943094,173.529088919052));
#41857=CARTESIAN_POINT('Ctrl Pts',(-59.9676016772374,-101.8682579127,172.221451540989));
#41858=CARTESIAN_POINT('Ctrl Pts',(-58.3427024120022,-102.135764258712,
172.016274058689));
#41859=CARTESIAN_POINT('Ctrl Pts',(-56.7178031467671,-102.403270604724,
171.81109657639));
#41860=CARTESIAN_POINT('Ctrl Pts',(-55.4274717279521,-102.635109783094,
172.828569176292));
#41861=CARTESIAN_POINT('Ctrl Pts',(-54.1371403091371,-102.866948961465,
173.846041776195));
#41862=CARTESIAN_POINT('Ctrl Pts',(-53.943056964401,-102.981920771222,175.490142808619));
#41863=CARTESIAN_POINT('Ctrl Pts',(-53.748973619665,-103.096892580979,177.134243841043));
#41864=CARTESIAN_POINT('Ctrl Pts',(-54.7706513225966,-103.082256140683,
178.441881219107));
#41865=CARTESIAN_POINT('Ctrl Pts',(-55.7923290255282,-103.067619700387,
179.74951859717));
#41866=CARTESIAN_POINT('Ctrl Pts',(-57.4371044165974,-102.986556883686,
179.954696079469));
#41867=CARTESIAN_POINT('Ctrl Pts',(-59.0818798076666,-102.905494066985,
180.159873561769));
#41868=CARTESIAN_POINT('Ctrl Pts',(-60.3920873523156,-102.860098417925,
179.142400961866));
#41869=CARTESIAN_POINT('Ctrl Pts',(-61.7022948969646,-102.814702768865,
178.124928361964));
#41870=CARTESIAN_POINT('Ctrl Pts',(-61.9162543675347,-102.886174488419,
176.48082732954));
#41871=CARTESIAN_POINT('Ctrl Pts',(-62.1302138381048,-102.957646207973,
174.836726297116));
#41872=CARTESIAN_POINT('Ctrl Pts',(-61.1284122610072,-103.158726177579,
173.529088919052));
#41873=CARTESIAN_POINT('Ctrl Pts',(-60.1266106839096,-103.359806147186,
172.221451540989));
#41874=CARTESIAN_POINT('Ctrl Pts',(-58.5017114186745,-103.627312493197,
172.016274058689));
#41875=CARTESIAN_POINT('Ctrl Pts',(-56.8768121534393,-103.894818839209,
171.81109657639));
#41876=CARTESIAN_POINT('Ctrl Pts',(-55.5864807346243,-104.12665801758,172.828569176292));
#41877=CARTESIAN_POINT('Ctrl Pts',(-54.2961493158093,-104.358497195951,
173.846041776195));
#41878=CARTESIAN_POINT('Ctrl Pts',(-54.1020659710732,-104.473469005708,
175.490142808619));
#41879=CARTESIAN_POINT('Ctrl Pts',(-53.9079826263372,-104.588440815464,
177.134243841043));
#41880=CARTESIAN_POINT('Ctrl Pts',(-54.9296603292688,-104.573804375168,
178.441881219107));
#41881=CARTESIAN_POINT('Ctrl Pts',(-55.9513380322004,-104.559167934873,
179.74951859717));
#41882=CARTESIAN_POINT('Ctrl Pts',(-57.5961134232696,-104.478105118172,
179.954696079469));
#41883=CARTESIAN_POINT('Ctrl Pts',(-59.2408888143388,-104.397042301471,
180.159873561769));
#41884=CARTESIAN_POINT('Ctrl Pts',(-60.5510963589878,-104.35164665241,179.142400961866));
#41885=CARTESIAN_POINT('Ctrl Pts',(-61.8613039036368,-104.30625100335,178.124928361964));
#41886=CARTESIAN_POINT('Ctrl Pts',(-62.0752633742069,-104.377722722904,
176.48082732954));
#41887=CARTESIAN_POINT('Ctrl Pts',(-62.289222844777,-104.449194442458,174.836726297116));
#41888=CARTESIAN_POINT('Ctrl Pts',(-61.2874212676794,-104.650274412065,
173.529088919052));
#41889=CARTESIAN_POINT('Ctrl Pts',(-60.2856196905818,-104.851354381671,
172.221451540989));
#41890=CARTESIAN_POINT('Ctrl Pts',(-58.6607204253467,-105.118860727683,
172.016274058689));
#41891=CARTESIAN_POINT('Ctrl Pts',(-57.0358211601115,-105.386367073695,
171.81109657639));
#41892=CARTESIAN_POINT('Ctrl Pts',(-55.7454897412965,-105.618206252066,
172.828569176292));
#41893=CARTESIAN_POINT('Ctrl Pts',(-54.4551583224815,-105.850045430437,
173.846041776195));
#41894=CARTESIAN_POINT('Ctrl Pts',(-54.2610749777455,-105.965017240193,
175.490142808619));
#41895=CARTESIAN_POINT('Ctrl Pts',(-54.0669916330094,-106.07998904995,177.134243841043));
#41896=CARTESIAN_POINT('Ctrl Pts',(-55.088669335941,-106.065352609654,178.441881219107));
#41897=CARTESIAN_POINT('Ctrl Pts',(-56.1103470388726,-106.050716169358,
179.74951859717));
#41898=CARTESIAN_POINT('Ctrl Pts',(-57.7551224299418,-105.969653352657,
179.954696079469));
#41899=CARTESIAN_POINT('Ctrl Pts',(-59.399897821011,-105.888590535956,180.159873561769));
#41900=CARTESIAN_POINT('Ctrl Pts',(-60.71010536566,-105.843194886896,179.142400961866));
#41901=CARTESIAN_POINT('Ctrl Pts',(-62.0203129103091,-105.797799237836,
178.124928361964));
#41902=CARTESIAN_POINT('Ctrl Pts',(-62.2342723808791,-105.86927095739,176.48082732954));
#41903=CARTESIAN_POINT('Ctrl Pts',(-62.4482318514492,-105.940742676944,
174.836726297116));
#41904=CARTESIAN_POINT('Ctrl Pts',(-61.4464302743516,-106.14182264655,173.529088919052));
#41905=CARTESIAN_POINT('Ctrl Pts',(-60.4446286972541,-106.342902616157,
172.221451540989));
#41906=CARTESIAN_POINT('Ctrl Pts',(-58.8197294320189,-106.610408962169,
172.016274058689));
#41907=CARTESIAN_POINT('Ctrl Pts',(-57.1948301667837,-106.87791530818,171.81109657639));
#41908=CARTESIAN_POINT('Ctrl Pts',(-55.9044987479688,-107.109754486551,
172.828569176292));
#41909=CARTESIAN_POINT('Ctrl Pts',(-54.6141673291538,-107.341593664922,
173.846041776195));
#41910=CARTESIAN_POINT('Ctrl Pts',(-54.4200839844177,-107.456565474679,
175.490142808619));
#41911=CARTESIAN_POINT('Ctrl Pts',(-54.2260006396817,-107.571537284435,
177.134243841043));
#41912=CARTESIAN_POINT('Ctrl Pts',(-55.2476783426132,-107.55690084414,178.441881219107));
#41913=CARTESIAN_POINT('Ctrl Pts',(-56.2693560455449,-107.542264403844,
179.74951859717));
#41914=CARTESIAN_POINT('Ctrl Pts',(-57.914131436614,-107.461201587143,179.954696079469));
#41915=CARTESIAN_POINT('Ctrl Pts',(-59.5589068276832,-107.380138770442,
180.159873561769));
#41916=CARTESIAN_POINT('Ctrl Pts',(-60.8691143723323,-107.334743121382,
179.142400961866));
#41917=CARTESIAN_POINT('Ctrl Pts',(-62.1793219169813,-107.289347472321,
178.124928361964));
#41918=CARTESIAN_POINT('Ctrl Pts',(-62.3932813875514,-107.360819191875,
176.48082732954));
#41919=CARTESIAN_POINT('Ctrl Pts',(-62.6072408581214,-107.43229091143,174.836726297116));
#41920=CARTESIAN_POINT('Ctrl Pts',(-61.6054392810239,-107.633370881036,
173.529088919052));
#41921=CARTESIAN_POINT('Ctrl Pts',(-60.6036377039263,-107.834450850642,
172.221451540989));
#41922=CARTESIAN_POINT('Ctrl Pts',(-58.9787384386911,-108.101957196654,
172.016274058689));
#41923=CARTESIAN_POINT('Ctrl Pts',(-57.353839173456,-108.369463542666,171.81109657639));
#41924=CARTESIAN_POINT('Ctrl Pts',(-56.063507754641,-108.601302721037,172.828569176292));
#41925=CARTESIAN_POINT('Ctrl Pts',(-54.773176335826,-108.833141899408,173.846041776195));
#41926=CARTESIAN_POINT('Ctrl Pts',(-54.5790929910899,-108.948113709164,
175.490142808619));
#41927=CARTESIAN_POINT('Ctrl Pts',(-54.3850096463539,-109.063085518921,
177.134243841043));
#41928=CARTESIAN_POINT('Ctrl Pts',(-55.4066873492855,-109.048449078625,
178.441881219107));
#41929=CARTESIAN_POINT('Ctrl Pts',(-56.4283650522171,-109.033812638329,
179.74951859717));
#41930=CARTESIAN_POINT('Ctrl Pts',(-58.0731404432863,-108.952749821628,
179.954696079469));
#41931=CARTESIAN_POINT('Ctrl Pts',(-59.7179158343555,-108.871687004927,
180.159873561769));
#41932=CARTESIAN_POINT('Ctrl Pts',(-61.0281233790045,-108.826291355867,
179.142400961866));
#41933=CARTESIAN_POINT('Ctrl Pts',(-62.3383309236535,-108.780895706807,
178.124928361964));
#41934=CARTESIAN_POINT('Ctrl Pts',(-62.5522903942236,-108.852367426361,
176.48082732954));
#41935=CARTESIAN_POINT('Ctrl Pts',(-62.7662498647937,-108.923839145915,
174.836726297116));
#41936=CARTESIAN_POINT('Ctrl Pts',(-61.7644482876961,-109.124919115522,
173.529088919052));
#41937=CARTESIAN_POINT('Ctrl Pts',(-60.7626467105985,-109.325999085128,
172.221451540989));
#41938=CARTESIAN_POINT('Ctrl Pts',(-59.1377474453634,-109.59350543114,172.016274058689));
#41939=CARTESIAN_POINT('Ctrl Pts',(-57.5128481801282,-109.861011777152,
171.81109657639));
#41940=CARTESIAN_POINT('Ctrl Pts',(-56.2225167613132,-110.092850955522,
172.828569176292));
#41941=CARTESIAN_POINT('Ctrl Pts',(-54.9321853424982,-110.324690133893,
173.846041776195));
#41942=CARTESIAN_POINT('Ctrl Pts',(-54.7381019977622,-110.43966194365,175.490142808619));
#41943=CARTESIAN_POINT('Ctrl Pts',(-54.5440186530261,-110.554633753407,
177.134243841043));
#41944=CARTESIAN_POINT('Ctrl Pts',(-55.5656963559577,-110.539997313111,
178.441881219107));
#41945=CARTESIAN_POINT('Ctrl Pts',(-56.5873740588893,-110.525360872815,
179.74951859717));
#41946=CARTESIAN_POINT('Ctrl Pts',(-58.2321494499585,-110.444298056114,
179.954696079469));
#41947=CARTESIAN_POINT('Ctrl Pts',(-59.8769248410277,-110.363235239413,
180.159873561769));
#41948=CARTESIAN_POINT('Ctrl Pts',(-61.1871323856767,-110.317839590353,
179.142400961866));
#41949=CARTESIAN_POINT('Ctrl Pts',(-62.4973399303257,-110.272443941293,
178.124928361964));
#41950=CARTESIAN_POINT('Ctrl Pts',(-62.7112994008958,-110.343915660847,
176.48082732954));
#41951=CARTESIAN_POINT('Ctrl Pts',(-62.9252588714659,-110.415387380401,
174.836726297116));
#41952=CARTESIAN_POINT('Ctrl Pts',(-61.9234572943683,-110.616467350007,
173.529088919052));
#41953=CARTESIAN_POINT('Ctrl Pts',(-60.9216557172708,-110.817547319614,
172.221451540989));
#41954=CARTESIAN_POINT('Ctrl Pts',(-59.2967564520356,-111.085053665625,
172.016274058689));
#41955=CARTESIAN_POINT('Ctrl Pts',(-57.6718571868004,-111.352560011637,
171.81109657639));
#41956=CARTESIAN_POINT('Ctrl Pts',(-56.3815257679854,-111.584399190008,
172.828569176292));
#41957=CARTESIAN_POINT('Ctrl Pts',(-55.0911943491704,-111.816238368379,
173.846041776195));
#41958=CARTESIAN_POINT('Ctrl Pts',(-54.8971110044344,-111.931210178136,
175.490142808619));
#41959=CARTESIAN_POINT('Ctrl Pts',(-54.7030276596983,-112.046181987892,
177.134243841043));
#41960=CARTESIAN_POINT('Ctrl Pts',(-55.7247053626299,-112.031545547596,
178.441881219107));
#41961=CARTESIAN_POINT('Ctrl Pts',(-56.7463830655615,-112.016909107301,
179.74951859717));
#41962=CARTESIAN_POINT('Ctrl Pts',(-58.3911584566307,-111.9358462906,179.954696079469));
#41963=CARTESIAN_POINT('Ctrl Pts',(-60.0359338476999,-111.854783473899,
180.159873561769));
#41964=CARTESIAN_POINT('Ctrl Pts',(-61.3461413923489,-111.809387824838,
179.142400961866));
#41965=CARTESIAN_POINT('Ctrl Pts',(-62.656348936998,-111.763992175778,178.124928361964));
#41966=CARTESIAN_POINT('Ctrl Pts',(-62.870308407568,-111.835463895332,176.48082732954));
#41967=CARTESIAN_POINT('Ctrl Pts',(-63.0842678781381,-111.906935614886,
174.836726297116));
#41968=CARTESIAN_POINT('Ctrl Pts',(-62.0824663010406,-112.108015584493,
173.529088919052));
#41969=CARTESIAN_POINT('Ctrl Pts',(-61.080664723943,-112.309095554099,172.221451540989));
#41970=CARTESIAN_POINT('Ctrl Pts',(-59.4557654587078,-112.576601900111,
172.016274058689));
#41971=CARTESIAN_POINT('Ctrl Pts',(-57.8308661934727,-112.844108246123,
171.81109657639));
#41972=CARTESIAN_POINT('Ctrl Pts',(-56.5405347746577,-113.075947424494,
172.828569176292));
#41973=CARTESIAN_POINT('Ctrl Pts',(-55.2502033558427,-113.307786602865,
173.846041776195));
#41974=CARTESIAN_POINT('Ctrl Pts',(-55.0561200111066,-113.422758412621,
175.490142808619));
#41975=CARTESIAN_POINT('Ctrl Pts',(-54.8620366663706,-113.537730222378,
177.134243841043));
#41976=CARTESIAN_POINT('Ctrl Pts',(-55.8837143693022,-113.523093782082,
178.441881219107));
#41977=CARTESIAN_POINT('Ctrl Pts',(-56.9053920722338,-113.508457341786,
179.74951859717));
#41978=CARTESIAN_POINT('Ctrl Pts',(-58.550167463303,-113.427394525085,179.954696079469));
#41979=CARTESIAN_POINT('Ctrl Pts',(-60.1949428543721,-113.346331708384,
180.159873561769));
#41980=CARTESIAN_POINT('Ctrl Pts',(-61.5051503990212,-113.300936059324,
179.142400961866));
#41981=CARTESIAN_POINT('Ctrl Pts',(-62.8153579436702,-113.255540410264,
178.124928361964));
#41982=CARTESIAN_POINT('Ctrl Pts',(-63.0293174142403,-113.327012129818,
176.48082732954));
#41983=CARTESIAN_POINT('Ctrl Pts',(-63.2432768848104,-113.398483849372,
174.836726297116));
#41984=CARTESIAN_POINT('Ctrl Pts',(-62.2414753077128,-113.599563818978,
173.529088919052));
#41985=CARTESIAN_POINT('Ctrl Pts',(-61.2396737306152,-113.800643788585,
172.221451540989));
#41986=CARTESIAN_POINT('Ctrl Pts',(-59.6147744653801,-114.068150134597,
172.016274058689));
#41987=CARTESIAN_POINT('Ctrl Pts',(-57.9898752001449,-114.335656480608,
171.81109657639));
#41988=CARTESIAN_POINT('Ctrl Pts',(-56.6995437813299,-114.567495658979,
172.828569176292));
#41989=CARTESIAN_POINT('Ctrl Pts',(-55.4092123625149,-114.79933483735,173.846041776195));
#41990=CARTESIAN_POINT('Ctrl Pts',(-55.2151290177788,-114.914306647107,
175.490142808619));
#41991=CARTESIAN_POINT('Ctrl Pts',(-55.0210456730428,-115.029278456863,
177.134243841043));
#41992=CARTESIAN_POINT('Ctrl Pts',(-56.0427233759744,-115.014642016568,
178.441881219107));
#41993=CARTESIAN_POINT('Ctrl Pts',(-57.064401078906,-115.000005576272,179.74951859717));
#41994=CARTESIAN_POINT('Ctrl Pts',(-58.7091764699752,-114.918942759571,
179.954696079469));
#41995=CARTESIAN_POINT('Ctrl Pts',(-60.3539518610444,-114.83787994287,180.159873561769));
#41996=CARTESIAN_POINT('Ctrl Pts',(-61.6641594056934,-114.79248429381,179.142400961866));
#41997=CARTESIAN_POINT('Ctrl Pts',(-62.9743669503424,-114.747088644749,
178.124928361964));
#41998=CARTESIAN_POINT('Ctrl Pts',(-63.1883264209125,-114.818560364303,
176.48082732954));
#41999=CARTESIAN_POINT('Ctrl Pts',(-63.4022858914826,-114.890032083858,
174.836726297116));
#42000=CARTESIAN_POINT('Ctrl Pts',(-62.400484314385,-115.091112053464,173.529088919052));
#42001=CARTESIAN_POINT('Ctrl Pts',(-61.3986827372874,-115.29219202307,172.221451540989));
#42002=CARTESIAN_POINT('Ctrl Pts',(-59.7737834720523,-115.559698369082,
172.016274058689));
#42003=CARTESIAN_POINT('Ctrl Pts',(-58.1488842068171,-115.827204715094,
171.81109657639));
#42004=CARTESIAN_POINT('Ctrl Pts',(-56.8585527880021,-116.059043893465,
172.828569176292));
#42005=CARTESIAN_POINT('Ctrl Pts',(-55.5682213691871,-116.290883071836,
173.846041776195));
#42006=CARTESIAN_POINT('Ctrl Pts',(-55.3741380244511,-116.405854881592,
175.490142808619));
#42007=CARTESIAN_POINT('Ctrl Pts',(-55.180054679715,-116.520826691349,177.134243841043));
#42008=CARTESIAN_POINT('Ctrl Pts',(-56.2017323826466,-116.506190251053,
178.441881219107));
#42009=CARTESIAN_POINT('Ctrl Pts',(-57.2234100855782,-116.491553810757,
179.74951859717));
#42010=CARTESIAN_POINT('Ctrl Pts',(-58.8681854766474,-116.410490994056,
179.954696079469));
#42011=CARTESIAN_POINT('Ctrl Pts',(-60.5129608677166,-116.329428177355,
180.159873561769));
#42012=CARTESIAN_POINT('Ctrl Pts',(-61.8231684123656,-116.284032528295,
179.142400961866));
#42013=CARTESIAN_POINT('Ctrl Pts',(-63.1333759570146,-116.238636879235,
178.124928361964));
#42014=CARTESIAN_POINT('Ctrl Pts',(-63.3473354275847,-116.310108598789,
176.48082732954));
#42015=CARTESIAN_POINT('Ctrl Pts',(-63.5612948981548,-116.381580318343,
174.836726297116));
#42016=CARTESIAN_POINT('Ctrl Pts',(-62.5594933210572,-116.58266028795,173.529088919052));
#42017=CARTESIAN_POINT('Ctrl Pts',(-61.5576917439597,-116.783740257556,
172.221451540989));
#42018=CARTESIAN_POINT('Ctrl Pts',(-59.9327924787245,-117.051246603568,
172.016274058689));
#42019=CARTESIAN_POINT('Ctrl Pts',(-58.3078932134894,-117.318752949579,
171.81109657639));
#42020=CARTESIAN_POINT('Ctrl Pts',(-57.0175617946743,-117.55059212795,172.828569176292));
#42021=CARTESIAN_POINT('Ctrl Pts',(-55.7272303758593,-117.782431306321,
173.846041776195));
#42022=CARTESIAN_POINT('Ctrl Pts',(-55.5331470311233,-117.897403116078,
175.490142808619));
#42023=CARTESIAN_POINT('Ctrl Pts',(-55.3390636863872,-118.012374925835,
177.134243841043));
#42024=CARTESIAN_POINT('Ctrl Pts',(-56.3607413893188,-117.997738485539,
178.441881219107));
#42025=CARTESIAN_POINT('Ctrl Pts',(-57.3824190922504,-117.983102045243,
179.74951859717));
#42026=CARTESIAN_POINT('Ctrl Pts',(-59.0271944833196,-117.902039228542,
179.954696079469));
#42027=CARTESIAN_POINT('Ctrl Pts',(-60.6719698743888,-117.820976411841,
180.159873561769));
#42028=CARTESIAN_POINT('Ctrl Pts',(-61.9821774190378,-117.775580762781,
179.142400961866));
#42029=CARTESIAN_POINT('Ctrl Pts',(-63.2923849636869,-117.730185113721,
178.124928361964));
#42030=CARTESIAN_POINT('Ctrl Pts',(-63.506344434257,-117.801656833275,176.48082732954));
#42031=CARTESIAN_POINT('Ctrl Pts',(-63.720303904827,-117.873128552829,174.836726297116));
#42032=CARTESIAN_POINT('Ctrl Pts',(-62.7185023277295,-118.074208522435,
173.529088919052));
#42033=CARTESIAN_POINT('Ctrl Pts',(-61.7167007506319,-118.275288492042,
172.221451540989));
#42034=CARTESIAN_POINT('Ctrl Pts',(-60.0918014853967,-118.542794838053,
172.016274058689));
#42035=CARTESIAN_POINT('Ctrl Pts',(-58.4669022201616,-118.810301184065,
171.81109657639));
#42036=CARTESIAN_POINT('Ctrl Pts',(-57.1765708013466,-119.042140362436,
172.828569176292));
#42037=CARTESIAN_POINT('Ctrl Pts',(-55.8862393825316,-119.273979540807,
173.846041776195));
#42038=CARTESIAN_POINT('Ctrl Pts',(-55.6921560377955,-119.388951350564,
175.490142808619));
#42039=CARTESIAN_POINT('Ctrl Pts',(-55.4980726930595,-119.50392316032,177.134243841043));
#42040=CARTESIAN_POINT('Ctrl Pts',(-56.5197503959911,-119.489286720024,
178.441881219107));
#42041=CARTESIAN_POINT('Ctrl Pts',(-57.5414280989227,-119.474650279729,
179.74951859717));
#42042=CARTESIAN_POINT('Ctrl Pts',(-59.1862034899919,-119.393587463028,
179.954696079469));
#42043=CARTESIAN_POINT('Ctrl Pts',(-60.8309788810611,-119.312524646327,
180.159873561769));
#42044=CARTESIAN_POINT('Ctrl Pts',(-62.1411864257101,-119.267128997266,
179.142400961866));
#42045=CARTESIAN_POINT('Ctrl Pts',(-63.4513939703591,-119.221733348206,
178.124928361964));
#42046=CARTESIAN_POINT('Ctrl Pts',(-63.6653534409292,-119.29320506776,176.48082732954));
#42047=CARTESIAN_POINT('Ctrl Pts',(-63.8793129114993,-119.364676787314,
174.836726297116));
#42048=CARTESIAN_POINT('Ctrl Pts',(-62.8775113344017,-119.565756756921,
173.529088919052));
#42049=CARTESIAN_POINT('Ctrl Pts',(-61.8757097573041,-119.766836726527,
172.221451540989));
#42050=CARTESIAN_POINT('Ctrl Pts',(-60.250810492069,-120.034343072539,172.016274058689));
#42051=CARTESIAN_POINT('Ctrl Pts',(-58.6259112268338,-120.301849418551,
171.81109657639));
#42052=CARTESIAN_POINT('Ctrl Pts',(-57.3355798080188,-120.533688596922,
172.828569176292));
#42053=CARTESIAN_POINT('Ctrl Pts',(-56.0452483892038,-120.765527775293,
173.846041776195));
#42054=CARTESIAN_POINT('Ctrl Pts',(-55.8511650444677,-120.880499585049,
175.490142808619));
#42055=CARTESIAN_POINT('Ctrl Pts',(-55.6570816997317,-120.995471394806,
177.134243841043));
#42056=CARTESIAN_POINT('Ctrl Pts',(-56.6787594026633,-120.98083495451,178.441881219107));
#42057=CARTESIAN_POINT('Ctrl Pts',(-57.7004371055949,-120.966198514214,
179.74951859717));
#42058=CARTESIAN_POINT('Ctrl Pts',(-59.3452124966641,-120.885135697513,
179.954696079469));
#42059=CARTESIAN_POINT('Ctrl Pts',(-60.9899878877333,-120.804072880812,
180.159873561769));
#42060=CARTESIAN_POINT('Ctrl Pts',(-62.3001954323823,-120.758677231752,
179.142400961866));
#42061=CARTESIAN_POINT('Ctrl Pts',(-63.6104029770313,-120.713281582692,
178.124928361964));
#42062=CARTESIAN_POINT('Ctrl Pts',(-63.8243624476014,-120.784753302246,
176.48082732954));
#42063=CARTESIAN_POINT('Ctrl Pts',(-64.0383219181715,-120.8562250218,174.836726297116));
#42064=CARTESIAN_POINT('Ctrl Pts',(-63.0365203410739,-121.057304991406,
173.529088919052));
#42065=CARTESIAN_POINT('Ctrl Pts',(-62.0347187639764,-121.258384961013,
172.221451540989));
#42066=CARTESIAN_POINT('Ctrl Pts',(-60.4098194987412,-121.525891307025,
172.016274058689));
#42067=CARTESIAN_POINT('Ctrl Pts',(-58.784920233506,-121.793397653036,171.81109657639));
#42068=CARTESIAN_POINT('Ctrl Pts',(-57.494588814691,-122.025236831407,172.828569176292));
#42069=CARTESIAN_POINT('Ctrl Pts',(-56.204257395876,-122.257076009778,173.846041776195));
#42070=CARTESIAN_POINT('Ctrl Pts',(-56.01017405114,-122.372047819535,175.490142808619));
#42071=CARTESIAN_POINT('Ctrl Pts',(-55.8160907064039,-122.487019629291,
177.134243841043));
#42072=CARTESIAN_POINT('Ctrl Pts',(-56.8377684093355,-122.472383188996,
178.441881219107));
#42073=CARTESIAN_POINT('Ctrl Pts',(-57.8594461122671,-122.4577467487,179.74951859717));
#42074=CARTESIAN_POINT('Ctrl Pts',(-59.5042215033363,-122.376683931999,
179.954696079469));
#42075=CARTESIAN_POINT('Ctrl Pts',(-61.1489968944055,-122.295621115298,
180.159873561769));
#42076=CARTESIAN_POINT('Ctrl Pts',(-62.4592044390545,-122.250225466238,
179.142400961866));
#42077=CARTESIAN_POINT('Ctrl Pts',(-63.7694119837035,-122.204829817177,
178.124928361964));
#42078=CARTESIAN_POINT('Ctrl Pts',(-63.9833714542736,-122.276301536731,
176.48082732954));
#42079=CARTESIAN_POINT('Ctrl Pts',(-64.1973309248437,-122.347773256285,
174.836726297116));
#42080=CARTESIAN_POINT('Ctrl Pts',(-63.1955293477461,-122.548853225892,
173.529088919052));
#42081=CARTESIAN_POINT('Ctrl Pts',(-62.1937277706486,-122.749933195498,
172.221451540989));
#42082=CARTESIAN_POINT('Ctrl Pts',(-60.5688285054134,-123.01743954151,172.016274058689));
#42083=CARTESIAN_POINT('Ctrl Pts',(-58.9439292401782,-123.284945887522,
171.81109657639));
#42084=CARTESIAN_POINT('Ctrl Pts',(-57.6535978213633,-123.516785065893,
172.828569176292));
#42085=CARTESIAN_POINT('Ctrl Pts',(-56.3632664025483,-123.748624244264,
173.846041776195));
#42086=CARTESIAN_POINT('Ctrl Pts',(-56.1691830578122,-123.86359605402,175.490142808619));
#42087=CARTESIAN_POINT('Ctrl Pts',(-55.9750997130761,-123.978567863777,
177.134243841043));
#42088=CARTESIAN_POINT('Ctrl Pts',(-56.9967774160077,-123.963931423481,
178.441881219107));
#42089=CARTESIAN_POINT('Ctrl Pts',(-58.0184551189394,-123.949294983185,
179.74951859717));
#42090=CARTESIAN_POINT('Ctrl Pts',(-59.6632305100085,-123.868232166484,
179.954696079469));
#42091=CARTESIAN_POINT('Ctrl Pts',(-61.3080059010777,-123.787169349783,
180.159873561769));
#42092=CARTESIAN_POINT('Ctrl Pts',(-62.6182134457268,-123.741773700723,
179.142400961866));
#42093=CARTESIAN_POINT('Ctrl Pts',(-63.9284209903758,-123.696378051663,
178.124928361964));
#42094=CARTESIAN_POINT('Ctrl Pts',(-64.1423804609459,-123.767849771217,
176.48082732954));
#42095=CARTESIAN_POINT('Ctrl Pts',(-64.3563399315159,-123.839321490771,
174.836726297116));
#42096=CARTESIAN_POINT('Ctrl Pts',(-63.3545383544184,-124.040401460378,
173.529088919052));
#42097=CARTESIAN_POINT('Ctrl Pts',(-62.3527367773208,-124.241481429984,
172.221451540989));
#42098=CARTESIAN_POINT('Ctrl Pts',(-60.7278375120856,-124.508987775996,
172.016274058689));
#42099=CARTESIAN_POINT('Ctrl Pts',(-59.1029382468505,-124.776494122007,
171.81109657639));
#42100=CARTESIAN_POINT('Ctrl Pts',(-57.8126068280355,-125.008333300378,
172.828569176292));
#42101=CARTESIAN_POINT('Ctrl Pts',(-56.5222754092205,-125.240172478749,
173.846041776195));
#42102=CARTESIAN_POINT('Ctrl Pts',(-56.3281920644844,-125.355144288506,
175.490142808619));
#42103=CARTESIAN_POINT('Ctrl Pts',(-56.1341087197484,-125.470116098263,
177.134243841043));
#42104=CARTESIAN_POINT('Ctrl Pts',(-57.15578642268,-125.455479657967,178.441881219107));
#42105=CARTESIAN_POINT('Ctrl Pts',(-58.1774641256116,-125.440843217671,
179.74951859717));
#42106=CARTESIAN_POINT('Ctrl Pts',(-59.8222395166808,-125.35978040097,179.954696079469));
#42107=CARTESIAN_POINT('Ctrl Pts',(-61.46701490775,-125.278717584269,180.159873561769));
#42108=CARTESIAN_POINT('Ctrl Pts',(-62.777222452399,-125.233321935209,179.142400961866));
#42109=CARTESIAN_POINT('Ctrl Pts',(-64.087429997048,-125.187926286149,178.124928361964));
#42110=CARTESIAN_POINT('Ctrl Pts',(-64.3013894676181,-125.259398005703,
176.48082732954));
#42111=CARTESIAN_POINT('Ctrl Pts',(-64.5153489381882,-125.330869725257,
174.836726297116));
#42112=CARTESIAN_POINT('Ctrl Pts',(-63.5135473610906,-125.531949694863,
173.529088919052));
#42113=CARTESIAN_POINT('Ctrl Pts',(-62.511745783993,-125.73302966447,172.221451540989));
#42114=CARTESIAN_POINT('Ctrl Pts',(-60.8868465187579,-126.000536010481,
172.016274058689));
#42115=CARTESIAN_POINT('Ctrl Pts',(-59.2619472535227,-126.268042356493,
171.81109657639));
#42116=CARTESIAN_POINT('Ctrl Pts',(-57.9716158347077,-126.499881534864,
172.828569176292));
#42117=CARTESIAN_POINT('Ctrl Pts',(-56.6812844158927,-126.731720713235,
173.846041776195));
#42118=CARTESIAN_POINT('Ctrl Pts',(-56.4872010711566,-126.846692522992,
175.490142808619));
#42119=CARTESIAN_POINT('Ctrl Pts',(-56.2931177264206,-126.961664332748,
177.134243841043));
#42120=CARTESIAN_POINT('Ctrl Pts',(-57.3147954293522,-126.947027892452,
178.441881219107));
#42121=CARTESIAN_POINT('Ctrl Pts',(-58.3364731322838,-126.932391452157,
179.74951859717));
#42122=CARTESIAN_POINT('Ctrl Pts',(-59.981248523353,-126.851328635456,179.954696079469));
#42123=CARTESIAN_POINT('Ctrl Pts',(-61.6260239144222,-126.770265818755,
180.159873561769));
#42124=CARTESIAN_POINT('Ctrl Pts',(-62.9362314590712,-126.724870169694,
179.142400961866));
#42125=CARTESIAN_POINT('Ctrl Pts',(-64.2464390037202,-126.679474520634,
178.124928361964));
#42126=CARTESIAN_POINT('Ctrl Pts',(-64.4603984742903,-126.750946240188,
176.48082732954));
#42127=CARTESIAN_POINT('Ctrl Pts',(-64.6743579448604,-126.822417959742,
174.836726297116));
#42128=CARTESIAN_POINT('Ctrl Pts',(-63.6725563677628,-127.023497929349,
173.529088919052));
#42129=CARTESIAN_POINT('Ctrl Pts',(-62.6707547906653,-127.224577898955,
172.221451540989));
#42130=CARTESIAN_POINT('Ctrl Pts',(-61.0458555254301,-127.492084244967,
172.016274058689));
#42131=CARTESIAN_POINT('Ctrl Pts',(-59.4209562601949,-127.759590590979,
171.81109657639));
#42132=CARTESIAN_POINT('Ctrl Pts',(-58.1306248413799,-127.99142976935,172.828569176292));
#42133=CARTESIAN_POINT('Ctrl Pts',(-56.8402934225649,-128.223268947721,
173.846041776195));
#42134=CARTESIAN_POINT('Ctrl Pts',(-56.6462100778289,-128.338240757477,
175.490142808619));
#42135=CARTESIAN_POINT('Ctrl Pts',(-56.4521267330928,-128.453212567234,
177.134243841043));
#42136=CARTESIAN_POINT('Ctrl Pts',(-57.4738044360244,-128.438576126938,
178.441881219107));
#42137=CARTESIAN_POINT('Ctrl Pts',(-58.495482138956,-128.423939686642,179.74951859717));
#42138=CARTESIAN_POINT('Ctrl Pts',(-60.1402575300252,-128.342876869941,
179.954696079469));
#42139=CARTESIAN_POINT('Ctrl Pts',(-61.7850329210944,-128.26181405324,180.159873561769));
#42140=CARTESIAN_POINT('Ctrl Pts',(-63.0952404657434,-128.21641840418,179.142400961866));
#42141=CARTESIAN_POINT('Ctrl Pts',(-64.4054480103925,-128.17102275512,178.124928361964));
#42142=CARTESIAN_POINT('Ctrl Pts',(-64.6194074809625,-128.242494474674,
176.48082732954));
#42143=CARTESIAN_POINT('Ctrl Pts',(-64.8333669515326,-128.313966194228,
174.836726297116));
#42144=CARTESIAN_POINT('Ctrl Pts',(-63.831565374435,-128.515046163834,173.529088919052));
#42145=CARTESIAN_POINT('Ctrl Pts',(-62.8297637973375,-128.716126133441,
172.221451540989));
#42146=CARTESIAN_POINT('Ctrl Pts',(-61.2048645321023,-128.983632479453,
172.016274058689));
#42147=CARTESIAN_POINT('Ctrl Pts',(-59.5799652668672,-129.251138825464,
171.81109657639));
#42148=CARTESIAN_POINT('Ctrl Pts',(-58.2896338480522,-129.482978003835,
172.828569176292));
#42149=CARTESIAN_POINT('Ctrl Pts',(-56.9993024292372,-129.714817182206,
173.846041776195));
#42150=CARTESIAN_POINT('Ctrl Pts',(-56.8052190845011,-129.829788991963,
175.490142808619));
#42151=CARTESIAN_POINT('Ctrl Pts',(-56.611135739765,-129.944760801719,177.134243841043));
#42152=CARTESIAN_POINT('Ctrl Pts',(-57.6328134426967,-129.930124361424,
178.441881219107));
#42153=CARTESIAN_POINT('Ctrl Pts',(-58.6544911456282,-129.915487921128,
179.74951859717));
#42154=CARTESIAN_POINT('Ctrl Pts',(-60.2992665366974,-129.834425104427,
179.954696079469));
#42155=CARTESIAN_POINT('Ctrl Pts',(-61.9440419277666,-129.753362287726,
180.159873561769));
#42156=CARTESIAN_POINT('Ctrl Pts',(-63.2542494724157,-129.707966638666,
179.142400961866));
#42157=CARTESIAN_POINT('Ctrl Pts',(-64.5644570170647,-129.662570989605,
178.124928361964));
#42158=CARTESIAN_POINT('Ctrl Pts',(-64.7784164876348,-129.734042709159,
176.48082732954));
#42159=CARTESIAN_POINT('Ctrl Pts',(-64.9923759582049,-129.805514428714,
174.836726297116));
#42160=CARTESIAN_POINT('Ctrl Pts',(-63.9905743811073,-130.00659439832,173.529088919052));
#42161=CARTESIAN_POINT('Ctrl Pts',(-62.9887728040097,-130.207674367926,
172.221451540989));
#42162=CARTESIAN_POINT('Ctrl Pts',(-61.3638735387746,-130.475180713938,
172.016274058689));
#42163=CARTESIAN_POINT('Ctrl Pts',(-59.7389742735394,-130.74268705995,171.81109657639));
#42164=CARTESIAN_POINT('Ctrl Pts',(-58.4486428547244,-130.974526238321,
172.828569176292));
#42165=CARTESIAN_POINT('Ctrl Pts',(-57.1583114359094,-131.206365416692,
173.846041776195));
#42166=CARTESIAN_POINT('Ctrl Pts',(-56.9642280911733,-131.321337226448,
175.490142808619));
#42167=CARTESIAN_POINT('Ctrl Pts',(-56.7701447464373,-131.436309036205,
177.134243841043));
#42168=CARTESIAN_POINT('Ctrl Pts',(-57.7918224493689,-131.421672595909,
178.441881219107));
#42169=CARTESIAN_POINT('Ctrl Pts',(-58.8135001523005,-131.407036155613,
179.74951859717));
#42170=CARTESIAN_POINT('Ctrl Pts',(-60.4582755433697,-131.325973338912,
179.954696079469));
#42171=CARTESIAN_POINT('Ctrl Pts',(-61.5222352836034,-131.273536043299,
180.087419721831));
#42172=CARTESIAN_POINT('Ctrl Pts',(-62.5109753341386,-131.233577943711,
179.670610857428));
#42173=CARTESIAN_POINT('Ctrl Pts',(-50.1237974946936,-67.3522581446913,
175.487549340184));
#42174=CARTESIAN_POINT('Ctrl Pts',(-49.9286459530297,-67.4673438313769,
177.140258408853));
#42175=CARTESIAN_POINT('Ctrl Pts',(-50.9556208313297,-67.452142676797,178.454742197037));
#42176=CARTESIAN_POINT('Ctrl Pts',(-51.9825957096297,-67.4369415222171,
179.76922598522));
#42177=CARTESIAN_POINT('Ctrl Pts',(-53.6359306348749,-67.3549662019876,
179.975477717318));
#42178=CARTESIAN_POINT('Ctrl Pts',(-55.2892655601202,-67.272990881758,180.181729449417));
#42179=CARTESIAN_POINT('Ctrl Pts',(-56.6062809387202,-67.2268694721162,
179.158929658031));
#42180=CARTESIAN_POINT('Ctrl Pts',(-57.9232963173202,-67.1807480624744,
178.136129866644));
#42181=CARTESIAN_POINT('Ctrl Pts',(-58.1383239848182,-67.2521059050995,
176.483420797975));
#42182=CARTESIAN_POINT('Ctrl Pts',(-58.3533516523161,-67.3234637477245,
174.830711729305));
#42183=CARTESIAN_POINT('Ctrl Pts',(-57.3462528998501,-67.5251084316151,
173.516227941122));
#42184=CARTESIAN_POINT('Ctrl Pts',(-56.3391541473842,-67.7267531155057,
172.201744152939));
#42185=CARTESIAN_POINT('Ctrl Pts',(-54.705695347973,-67.995171965046,171.99549242084));
#42186=CARTESIAN_POINT('Ctrl Pts',(-53.0722365485618,-68.2635908145862,
171.789240688742));
#42187=CARTESIAN_POINT('Ctrl Pts',(-51.7750972957957,-68.4961557535387,
172.812040480128));
#42188=CARTESIAN_POINT('Ctrl Pts',(-50.4779580430297,-68.7287206924912,
173.834840271514));
#42189=CARTESIAN_POINT('Ctrl Pts',(-50.2828065013658,-68.8438063791769,
175.487549340184));
#42190=CARTESIAN_POINT('Ctrl Pts',(-50.0876549597019,-68.9588920658625,
177.140258408853));
#42191=CARTESIAN_POINT('Ctrl Pts',(-51.1146298380019,-68.9436909112826,
178.454742197037));
#42192=CARTESIAN_POINT('Ctrl Pts',(-52.1416047163019,-68.9284897567027,
179.76922598522));
#42193=CARTESIAN_POINT('Ctrl Pts',(-53.7949396415471,-68.8465144364732,
179.975477717318));
#42194=CARTESIAN_POINT('Ctrl Pts',(-55.4482745667924,-68.7645391162437,
180.181729449417));
#42195=CARTESIAN_POINT('Ctrl Pts',(-56.7652899453924,-68.7184177066018,
179.158929658031));
#42196=CARTESIAN_POINT('Ctrl Pts',(-58.0823053239925,-68.67229629696,178.136129866644));
#42197=CARTESIAN_POINT('Ctrl Pts',(-58.2973329914904,-68.7436541395851,
176.483420797975));
#42198=CARTESIAN_POINT('Ctrl Pts',(-58.5123606589883,-68.8150119822101,
174.830711729305));
#42199=CARTESIAN_POINT('Ctrl Pts',(-57.5052619065224,-69.0166566661007,
173.516227941122));
#42200=CARTESIAN_POINT('Ctrl Pts',(-56.4981631540564,-69.2183013499913,
172.201744152939));
#42201=CARTESIAN_POINT('Ctrl Pts',(-54.8647043546452,-69.4867201995316,
171.99549242084));
#42202=CARTESIAN_POINT('Ctrl Pts',(-53.231245555234,-69.7551390490718,171.789240688742));
#42203=CARTESIAN_POINT('Ctrl Pts',(-51.934106302468,-69.9877039880243,172.812040480128));
#42204=CARTESIAN_POINT('Ctrl Pts',(-50.636967049702,-70.2202689269768,173.834840271514));
#42205=CARTESIAN_POINT('Ctrl Pts',(-50.4418155080381,-70.3353546136625,
175.487549340184));
#42206=CARTESIAN_POINT('Ctrl Pts',(-50.2466639663742,-70.4504403003481,
177.140258408853));
#42207=CARTESIAN_POINT('Ctrl Pts',(-51.2736388446741,-70.4352391457682,
178.454742197037));
#42208=CARTESIAN_POINT('Ctrl Pts',(-52.3006137229741,-70.4200379911883,
179.76922598522));
#42209=CARTESIAN_POINT('Ctrl Pts',(-53.9539486482194,-70.3380626709587,
179.975477717318));
#42210=CARTESIAN_POINT('Ctrl Pts',(-55.6072835734646,-70.2560873507292,
180.181729449417));
#42211=CARTESIAN_POINT('Ctrl Pts',(-56.9242989520647,-70.2099659410874,
179.158929658031));
#42212=CARTESIAN_POINT('Ctrl Pts',(-58.2413143306647,-70.1638445314456,
178.136129866644));
#42213=CARTESIAN_POINT('Ctrl Pts',(-58.4563419981626,-70.2352023740707,
176.483420797975));
#42214=CARTESIAN_POINT('Ctrl Pts',(-58.6713696656605,-70.3065602166957,
174.830711729305));
#42215=CARTESIAN_POINT('Ctrl Pts',(-57.6642709131946,-70.5082049005863,
173.516227941122));
#42216=CARTESIAN_POINT('Ctrl Pts',(-56.6571721607287,-70.7098495844769,
172.201744152939));
#42217=CARTESIAN_POINT('Ctrl Pts',(-55.0237133613174,-70.9782684340172,
171.99549242084));
#42218=CARTESIAN_POINT('Ctrl Pts',(-53.3902545619062,-71.2466872835574,
171.789240688742));
#42219=CARTESIAN_POINT('Ctrl Pts',(-52.0931153091402,-71.4792522225099,
172.812040480128));
#42220=CARTESIAN_POINT('Ctrl Pts',(-50.7959760563742,-71.7118171614624,
173.834840271514));
#42221=CARTESIAN_POINT('Ctrl Pts',(-50.6008245147103,-71.8269028481481,
175.487549340184));
#42222=CARTESIAN_POINT('Ctrl Pts',(-50.4056729730464,-71.9419885348337,
177.140258408853));
#42223=CARTESIAN_POINT('Ctrl Pts',(-51.4326478513464,-71.9267873802538,
178.454742197037));
#42224=CARTESIAN_POINT('Ctrl Pts',(-52.4596227296463,-71.9115862256739,
179.76922598522));
#42225=CARTESIAN_POINT('Ctrl Pts',(-54.1129576548916,-71.8296109054444,
179.975477717318));
#42226=CARTESIAN_POINT('Ctrl Pts',(-55.7662925801368,-71.7476355852148,
180.181729449417));
#42227=CARTESIAN_POINT('Ctrl Pts',(-57.0833079587369,-71.701514175573,179.158929658031));
#42228=CARTESIAN_POINT('Ctrl Pts',(-58.4003233373369,-71.6553927659312,
178.136129866644));
#42229=CARTESIAN_POINT('Ctrl Pts',(-58.6153510048348,-71.7267506085562,
176.483420797975));
#42230=CARTESIAN_POINT('Ctrl Pts',(-58.8303786723328,-71.7981084511813,
174.830711729305));
#42231=CARTESIAN_POINT('Ctrl Pts',(-57.8232799198668,-71.9997531350719,
173.516227941122));
#42232=CARTESIAN_POINT('Ctrl Pts',(-56.8161811674009,-72.2013978189625,
172.201744152939));
#42233=CARTESIAN_POINT('Ctrl Pts',(-55.1827223679897,-72.4698166685028,
171.99549242084));
#42234=CARTESIAN_POINT('Ctrl Pts',(-53.5492635685784,-72.738235518043,171.789240688742));
#42235=CARTESIAN_POINT('Ctrl Pts',(-52.2521243158124,-72.9708004569955,
172.812040480128));
#42236=CARTESIAN_POINT('Ctrl Pts',(-50.9549850630464,-73.203365395948,173.834840271514));
#42237=CARTESIAN_POINT('Ctrl Pts',(-50.7598335213825,-73.3184510826337,
175.487549340184));
#42238=CARTESIAN_POINT('Ctrl Pts',(-50.5646819797186,-73.4335367693193,
177.140258408853));
#42239=CARTESIAN_POINT('Ctrl Pts',(-51.5916568580186,-73.4183356147394,
178.454742197037));
#42240=CARTESIAN_POINT('Ctrl Pts',(-52.6186317363186,-73.4031344601595,
179.76922598522));
#42241=CARTESIAN_POINT('Ctrl Pts',(-54.2719666615638,-73.32115913993,179.975477717318));
#42242=CARTESIAN_POINT('Ctrl Pts',(-55.9253015868091,-73.2391838197004,
180.181729449417));
#42243=CARTESIAN_POINT('Ctrl Pts',(-57.2423169654091,-73.1930624100586,
179.158929658031));
#42244=CARTESIAN_POINT('Ctrl Pts',(-58.5593323440091,-73.1469410004168,
178.136129866644));
#42245=CARTESIAN_POINT('Ctrl Pts',(-58.7743600115071,-73.2182988430419,
176.483420797975));
#42246=CARTESIAN_POINT('Ctrl Pts',(-58.989387679005,-73.2896566856669,174.830711729305));
#42247=CARTESIAN_POINT('Ctrl Pts',(-57.9822889265391,-73.4913013695575,
173.516227941122));
#42248=CARTESIAN_POINT('Ctrl Pts',(-56.9751901740731,-73.6929460534481,
172.201744152939));
#42249=CARTESIAN_POINT('Ctrl Pts',(-55.3417313746619,-73.9613649029884,
171.99549242084));
#42250=CARTESIAN_POINT('Ctrl Pts',(-53.7082725752507,-74.2297837525286,
171.789240688742));
#42251=CARTESIAN_POINT('Ctrl Pts',(-52.4111333224846,-74.4623486914811,
172.812040480128));
#42252=CARTESIAN_POINT('Ctrl Pts',(-51.1139940697186,-74.6949136304336,
173.834840271514));
#42253=CARTESIAN_POINT('Ctrl Pts',(-50.9188425280547,-74.8099993171193,
175.487549340184));
#42254=CARTESIAN_POINT('Ctrl Pts',(-50.7236909863908,-74.9250850038049,
177.140258408853));
#42255=CARTESIAN_POINT('Ctrl Pts',(-51.7506658646908,-74.909883849225,178.454742197037));
#42256=CARTESIAN_POINT('Ctrl Pts',(-52.7776407429908,-74.8946826946451,
179.76922598522));
#42257=CARTESIAN_POINT('Ctrl Pts',(-54.430975668236,-74.8127073744155,179.975477717318));
#42258=CARTESIAN_POINT('Ctrl Pts',(-56.0843105934813,-74.730732054186,180.181729449417));
#42259=CARTESIAN_POINT('Ctrl Pts',(-57.4013259720813,-74.6846106445442,
179.158929658031));
#42260=CARTESIAN_POINT('Ctrl Pts',(-58.7183413506814,-74.6384892349024,
178.136129866644));
#42261=CARTESIAN_POINT('Ctrl Pts',(-58.9333690181793,-74.7098470775275,
176.483420797975));
#42262=CARTESIAN_POINT('Ctrl Pts',(-59.1483966856772,-74.7812049201525,
174.830711729305));
#42263=CARTESIAN_POINT('Ctrl Pts',(-58.1412979332113,-74.9828496040431,
173.516227941122));
#42264=CARTESIAN_POINT('Ctrl Pts',(-57.1341991807453,-75.1844942879338,
172.201744152939));
#42265=CARTESIAN_POINT('Ctrl Pts',(-55.5007403813341,-75.452913137474,171.99549242084));
#42266=CARTESIAN_POINT('Ctrl Pts',(-53.8672815819229,-75.7213319870142,
171.789240688742));
#42267=CARTESIAN_POINT('Ctrl Pts',(-52.5701423291569,-75.9538969259667,
172.812040480128));
#42268=CARTESIAN_POINT('Ctrl Pts',(-51.2730030763909,-76.1864618649192,
173.834840271514));
#42269=CARTESIAN_POINT('Ctrl Pts',(-51.077851534727,-76.3015475516049,175.487549340184));
#42270=CARTESIAN_POINT('Ctrl Pts',(-50.8826999930631,-76.4166332382905,
177.140258408853));
#42271=CARTESIAN_POINT('Ctrl Pts',(-51.9096748713631,-76.4014320837106,
178.454742197037));
#42272=CARTESIAN_POINT('Ctrl Pts',(-52.936649749663,-76.3862309291307,179.76922598522));
#42273=CARTESIAN_POINT('Ctrl Pts',(-54.5899846749083,-76.3042556089012,
179.975477717318));
#42274=CARTESIAN_POINT('Ctrl Pts',(-56.2433196001535,-76.2222802886716,
180.181729449417));
#42275=CARTESIAN_POINT('Ctrl Pts',(-57.5603349787536,-76.1761588790298,
179.158929658031));
#42276=CARTESIAN_POINT('Ctrl Pts',(-58.8773503573536,-76.130037469388,178.136129866644));
#42277=CARTESIAN_POINT('Ctrl Pts',(-59.0923780248515,-76.2013953120131,
176.483420797975));
#42278=CARTESIAN_POINT('Ctrl Pts',(-59.3074056923495,-76.2727531546381,
174.830711729305));
#42279=CARTESIAN_POINT('Ctrl Pts',(-58.3003069398835,-76.4743978385287,
173.516227941122));
#42280=CARTESIAN_POINT('Ctrl Pts',(-57.2932081874176,-76.6760425224193,
172.201744152939));
#42281=CARTESIAN_POINT('Ctrl Pts',(-55.6597493880063,-76.9444613719596,
171.99549242084));
#42282=CARTESIAN_POINT('Ctrl Pts',(-54.0262905885951,-77.2128802214998,
171.789240688742));
#42283=CARTESIAN_POINT('Ctrl Pts',(-52.7291513358291,-77.4454451604523,
172.812040480128));
#42284=CARTESIAN_POINT('Ctrl Pts',(-51.4320120830631,-77.6780100994048,
173.834840271514));
#42285=CARTESIAN_POINT('Ctrl Pts',(-51.2368605413992,-77.7930957860905,
175.487549340184));
#42286=CARTESIAN_POINT('Ctrl Pts',(-51.0417089997353,-77.9081814727761,
177.140258408853));
#42287=CARTESIAN_POINT('Ctrl Pts',(-52.0686838780353,-77.8929803181962,
178.454742197037));
#42288=CARTESIAN_POINT('Ctrl Pts',(-53.0956587563352,-77.8777791636163,
179.76922598522));
#42289=CARTESIAN_POINT('Ctrl Pts',(-54.7489936815805,-77.7958038433868,
179.975477717318));
#42290=CARTESIAN_POINT('Ctrl Pts',(-56.4023286068258,-77.7138285231572,
180.181729449417));
#42291=CARTESIAN_POINT('Ctrl Pts',(-57.7193439854258,-77.6677071135154,
179.158929658031));
#42292=CARTESIAN_POINT('Ctrl Pts',(-59.0363593640258,-77.6215857038736,
178.136129866644));
#42293=CARTESIAN_POINT('Ctrl Pts',(-59.2513870315238,-77.6929435464986,
176.483420797975));
#42294=CARTESIAN_POINT('Ctrl Pts',(-59.4664146990217,-77.7643013891237,
174.830711729305));
#42295=CARTESIAN_POINT('Ctrl Pts',(-58.4593159465557,-77.9659460730143,
173.516227941122));
#42296=CARTESIAN_POINT('Ctrl Pts',(-57.4522171940898,-78.167590756905,172.201744152939));
#42297=CARTESIAN_POINT('Ctrl Pts',(-55.8187583946786,-78.4360096064452,
171.99549242084));
#42298=CARTESIAN_POINT('Ctrl Pts',(-54.1852995952674,-78.7044284559854,
171.789240688742));
#42299=CARTESIAN_POINT('Ctrl Pts',(-52.8881603425013,-78.9369933949379,
172.812040480128));
#42300=CARTESIAN_POINT('Ctrl Pts',(-51.5910210897353,-79.1695583338904,
173.834840271514));
#42301=CARTESIAN_POINT('Ctrl Pts',(-51.3958695480714,-79.2846440205761,
175.487549340184));
#42302=CARTESIAN_POINT('Ctrl Pts',(-51.2007180064075,-79.3997297072617,
177.140258408853));
#42303=CARTESIAN_POINT('Ctrl Pts',(-52.2276928847075,-79.3845285526818,
178.454742197037));
#42304=CARTESIAN_POINT('Ctrl Pts',(-53.2546677630075,-79.3693273981019,
179.76922598522));
#42305=CARTESIAN_POINT('Ctrl Pts',(-54.9080026882527,-79.2873520778724,
179.975477717318));
#42306=CARTESIAN_POINT('Ctrl Pts',(-56.561337613498,-79.2053767576428,180.181729449417));
#42307=CARTESIAN_POINT('Ctrl Pts',(-57.878352992098,-79.159255348001,179.158929658031));
#42308=CARTESIAN_POINT('Ctrl Pts',(-59.1953683706981,-79.1131339383592,
178.136129866644));
#42309=CARTESIAN_POINT('Ctrl Pts',(-59.410396038196,-79.1844917809843,176.483420797975));
#42310=CARTESIAN_POINT('Ctrl Pts',(-59.6254237056939,-79.2558496236093,
174.830711729305));
#42311=CARTESIAN_POINT('Ctrl Pts',(-58.618324953228,-79.4574943074999,173.516227941122));
#42312=CARTESIAN_POINT('Ctrl Pts',(-57.611226200762,-79.6591389913905,172.201744152939));
#42313=CARTESIAN_POINT('Ctrl Pts',(-55.9777674013508,-79.9275578409308,
171.99549242084));
#42314=CARTESIAN_POINT('Ctrl Pts',(-54.3443086019396,-80.195976690471,171.789240688742));
#42315=CARTESIAN_POINT('Ctrl Pts',(-53.0471693491736,-80.4285416294235,
172.812040480128));
#42316=CARTESIAN_POINT('Ctrl Pts',(-51.7500300964075,-80.6611065683761,
173.834840271514));
#42317=CARTESIAN_POINT('Ctrl Pts',(-51.5548785547437,-80.7761922550617,
175.487549340184));
#42318=CARTESIAN_POINT('Ctrl Pts',(-51.3597270130797,-80.8912779417473,
177.140258408853));
#42319=CARTESIAN_POINT('Ctrl Pts',(-52.3867018913797,-80.8760767871674,
178.454742197037));
#42320=CARTESIAN_POINT('Ctrl Pts',(-53.4136767696797,-80.8608756325875,
179.76922598522));
#42321=CARTESIAN_POINT('Ctrl Pts',(-55.067011694925,-80.778900312358,179.975477717318));
#42322=CARTESIAN_POINT('Ctrl Pts',(-56.7203466201702,-80.6969249921285,
180.181729449417));
#42323=CARTESIAN_POINT('Ctrl Pts',(-58.0373619987702,-80.6508035824866,
179.158929658031));
#42324=CARTESIAN_POINT('Ctrl Pts',(-59.3543773773703,-80.6046821728448,
178.136129866644));
#42325=CARTESIAN_POINT('Ctrl Pts',(-59.5694050448682,-80.6760400154699,
176.483420797975));
#42326=CARTESIAN_POINT('Ctrl Pts',(-59.7844327123661,-80.7473978580949,
174.830711729305));
#42327=CARTESIAN_POINT('Ctrl Pts',(-58.7773339599002,-80.9490425419855,
173.516227941122));
#42328=CARTESIAN_POINT('Ctrl Pts',(-57.7702352074343,-81.1506872258762,
172.201744152939));
#42329=CARTESIAN_POINT('Ctrl Pts',(-56.136776408023,-81.4191060754164,171.99549242084));
#42330=CARTESIAN_POINT('Ctrl Pts',(-54.5033176086118,-81.6875249249566,
171.789240688742));
#42331=CARTESIAN_POINT('Ctrl Pts',(-53.2061783558458,-81.9200898639091,
172.812040480128));
#42332=CARTESIAN_POINT('Ctrl Pts',(-51.9090391030798,-82.1526548028617,
173.834840271514));
#42333=CARTESIAN_POINT('Ctrl Pts',(-51.7138875614159,-82.2677404895473,
175.487549340184));
#42334=CARTESIAN_POINT('Ctrl Pts',(-51.518736019752,-82.382826176233,177.140258408853));
#42335=CARTESIAN_POINT('Ctrl Pts',(-52.545710898052,-82.367625021653,178.454742197037));
#42336=CARTESIAN_POINT('Ctrl Pts',(-53.5726857763519,-82.3524238670731,
179.76922598522));
#42337=CARTESIAN_POINT('Ctrl Pts',(-55.2260207015972,-82.2704485468436,
179.975477717318));
#42338=CARTESIAN_POINT('Ctrl Pts',(-56.8793556268424,-82.188473226614,180.181729449417));
#42339=CARTESIAN_POINT('Ctrl Pts',(-58.1963710054425,-82.1423518169722,
179.158929658031));
#42340=CARTESIAN_POINT('Ctrl Pts',(-59.5133863840425,-82.0962304073304,
178.136129866644));
#42341=CARTESIAN_POINT('Ctrl Pts',(-59.7284140515404,-82.1675882499554,
176.483420797975));
#42342=CARTESIAN_POINT('Ctrl Pts',(-59.9434417190384,-82.2389460925805,
174.830711729305));
#42343=CARTESIAN_POINT('Ctrl Pts',(-58.9363429665724,-82.4405907764711,
173.516227941122));
#42344=CARTESIAN_POINT('Ctrl Pts',(-57.9292442141065,-82.6422354603618,
172.201744152939));
#42345=CARTESIAN_POINT('Ctrl Pts',(-56.2957854146952,-82.910654309902,171.99549242084));
#42346=CARTESIAN_POINT('Ctrl Pts',(-54.662326615284,-83.1790731594422,171.789240688742));
#42347=CARTESIAN_POINT('Ctrl Pts',(-53.365187362518,-83.4116380983947,172.812040480128));
#42348=CARTESIAN_POINT('Ctrl Pts',(-52.068048109752,-83.6442030373472,173.834840271514));
#42349=CARTESIAN_POINT('Ctrl Pts',(-51.8728965680881,-83.7592887240329,
175.487549340184));
#42350=CARTESIAN_POINT('Ctrl Pts',(-51.6777450264242,-83.8743744107186,
177.140258408853));
#42351=CARTESIAN_POINT('Ctrl Pts',(-52.7047199047242,-83.8591732561386,
178.454742197037));
#42352=CARTESIAN_POINT('Ctrl Pts',(-53.7316947830242,-83.8439721015587,
179.76922598522));
#42353=CARTESIAN_POINT('Ctrl Pts',(-55.3850297082694,-83.7619967813292,
179.975477717318));
#42354=CARTESIAN_POINT('Ctrl Pts',(-57.0383646335147,-83.6800214610996,
180.181729449417));
#42355=CARTESIAN_POINT('Ctrl Pts',(-58.3553800121147,-83.6339000514578,
179.158929658031));
#42356=CARTESIAN_POINT('Ctrl Pts',(-59.6723953907147,-83.587778641816,178.136129866644));
#42357=CARTESIAN_POINT('Ctrl Pts',(-59.8874230582127,-83.6591364844411,
176.483420797975));
#42358=CARTESIAN_POINT('Ctrl Pts',(-60.1024507257106,-83.7304943270661,
174.830711729305));
#42359=CARTESIAN_POINT('Ctrl Pts',(-59.0953519732446,-83.9321390109568,
173.516227941122));
#42360=CARTESIAN_POINT('Ctrl Pts',(-58.0882532207787,-84.1337836948473,
172.201744152939));
#42361=CARTESIAN_POINT('Ctrl Pts',(-56.4547944213675,-84.4022025443876,
171.99549242084));
#42362=CARTESIAN_POINT('Ctrl Pts',(-54.8213356219563,-84.6706213939278,
171.789240688742));
#42363=CARTESIAN_POINT('Ctrl Pts',(-53.5241963691902,-84.9031863328803,
172.812040480128));
#42364=CARTESIAN_POINT('Ctrl Pts',(-52.2270571164242,-85.1357512718329,
173.834840271514));
#42365=CARTESIAN_POINT('Ctrl Pts',(-52.0319055747603,-85.2508369585185,
175.487549340184));
#42366=CARTESIAN_POINT('Ctrl Pts',(-51.8367540330964,-85.3659226452041,
177.140258408853));
#42367=CARTESIAN_POINT('Ctrl Pts',(-52.8637289113964,-85.3507214906242,
178.454742197037));
#42368=CARTESIAN_POINT('Ctrl Pts',(-53.8907037896964,-85.3355203360443,
179.76922598522));
#42369=CARTESIAN_POINT('Ctrl Pts',(-55.5440387149416,-85.2535450158148,
179.975477717318));
#42370=CARTESIAN_POINT('Ctrl Pts',(-57.1973736401869,-85.1715696955852,
180.181729449417));
#42371=CARTESIAN_POINT('Ctrl Pts',(-58.5143890187869,-85.1254482859434,
179.158929658031));
#42372=CARTESIAN_POINT('Ctrl Pts',(-59.831404397387,-85.0793268763016,178.136129866644));
#42373=CARTESIAN_POINT('Ctrl Pts',(-60.0464320648849,-85.1506847189267,
176.483420797975));
#42374=CARTESIAN_POINT('Ctrl Pts',(-60.2614597323828,-85.2220425615517,
174.830711729305));
#42375=CARTESIAN_POINT('Ctrl Pts',(-59.2543609799169,-85.4236872454423,
173.516227941122));
#42376=CARTESIAN_POINT('Ctrl Pts',(-58.2472622274509,-85.6253319293329,
172.201744152939));
#42377=CARTESIAN_POINT('Ctrl Pts',(-56.6138034280397,-85.8937507788732,
171.99549242084));
#42378=CARTESIAN_POINT('Ctrl Pts',(-54.9803446286285,-86.1621696284134,
171.789240688742));
#42379=CARTESIAN_POINT('Ctrl Pts',(-53.6832053758625,-86.3947345673659,
172.812040480128));
#42380=CARTESIAN_POINT('Ctrl Pts',(-52.3860661230965,-86.6272995063184,
173.834840271514));
#42381=CARTESIAN_POINT('Ctrl Pts',(-52.1909145814326,-86.7423851930041,
175.487549340184));
#42382=CARTESIAN_POINT('Ctrl Pts',(-51.9957630397687,-86.8574708796897,
177.140258408853));
#42383=CARTESIAN_POINT('Ctrl Pts',(-53.0227379180686,-86.8422697251098,
178.454742197037));
#42384=CARTESIAN_POINT('Ctrl Pts',(-54.0497127963686,-86.8270685705299,
179.76922598522));
#42385=CARTESIAN_POINT('Ctrl Pts',(-55.7030477216139,-86.7450932503004,
179.975477717318));
#42386=CARTESIAN_POINT('Ctrl Pts',(-57.3563826468591,-86.6631179300708,
180.181729449417));
#42387=CARTESIAN_POINT('Ctrl Pts',(-58.6733980254591,-86.616996520429,179.158929658031));
#42388=CARTESIAN_POINT('Ctrl Pts',(-59.9904134040592,-86.5708751107872,
178.136129866644));
#42389=CARTESIAN_POINT('Ctrl Pts',(-60.2054410715571,-86.6422329534122,
176.483420797975));
#42390=CARTESIAN_POINT('Ctrl Pts',(-60.4204687390551,-86.7135907960373,
174.830711729305));
#42391=CARTESIAN_POINT('Ctrl Pts',(-59.4133699865891,-86.9152354799279,
173.516227941122));
#42392=CARTESIAN_POINT('Ctrl Pts',(-58.4062712341232,-87.1168801638185,
172.201744152939));
#42393=CARTESIAN_POINT('Ctrl Pts',(-56.7728124347119,-87.3852990133588,
171.99549242084));
#42394=CARTESIAN_POINT('Ctrl Pts',(-55.1393536353007,-87.653717862899,171.789240688742));
#42395=CARTESIAN_POINT('Ctrl Pts',(-53.8422143825347,-87.8862828018515,
172.812040480128));
#42396=CARTESIAN_POINT('Ctrl Pts',(-52.5450751297687,-88.118847740804,173.834840271514));
#42397=CARTESIAN_POINT('Ctrl Pts',(-52.3499235881048,-88.2339334274897,
175.487549340184));
#42398=CARTESIAN_POINT('Ctrl Pts',(-52.1547720464409,-88.3490191141753,
177.140258408853));
#42399=CARTESIAN_POINT('Ctrl Pts',(-53.1817469247409,-88.3338179595954,
178.454742197037));
#42400=CARTESIAN_POINT('Ctrl Pts',(-54.2087218030408,-88.3186168050155,
179.76922598522));
#42401=CARTESIAN_POINT('Ctrl Pts',(-55.8620567282861,-88.236641484786,179.975477717318));
#42402=CARTESIAN_POINT('Ctrl Pts',(-57.5153916535314,-88.1546661645564,
180.181729449417));
#42403=CARTESIAN_POINT('Ctrl Pts',(-58.8324070321314,-88.1085447549146,
179.158929658031));
#42404=CARTESIAN_POINT('Ctrl Pts',(-60.1494224107314,-88.0624233452728,
178.136129866644));
#42405=CARTESIAN_POINT('Ctrl Pts',(-60.3644500782293,-88.1337811878979,
176.483420797975));
#42406=CARTESIAN_POINT('Ctrl Pts',(-60.5794777457273,-88.2051390305229,
174.830711729305));
#42407=CARTESIAN_POINT('Ctrl Pts',(-59.5723789932613,-88.4067837144135,
173.516227941122));
#42408=CARTESIAN_POINT('Ctrl Pts',(-58.5652802407954,-88.6084283983041,
172.201744152939));
#42409=CARTESIAN_POINT('Ctrl Pts',(-56.9318214413842,-88.8768472478444,
171.99549242084));
#42410=CARTESIAN_POINT('Ctrl Pts',(-55.2983626419729,-89.1452660973846,
171.789240688742));
#42411=CARTESIAN_POINT('Ctrl Pts',(-54.0012233892069,-89.3778310363371,
172.812040480128));
#42412=CARTESIAN_POINT('Ctrl Pts',(-52.7040841364409,-89.6103959752896,
173.834840271514));
#42413=CARTESIAN_POINT('Ctrl Pts',(-52.508932594777,-89.7254816619753,175.487549340184));
#42414=CARTESIAN_POINT('Ctrl Pts',(-52.3137810531131,-89.840567348661,177.140258408853));
#42415=CARTESIAN_POINT('Ctrl Pts',(-53.3407559314131,-89.825366194081,178.454742197037));
#42416=CARTESIAN_POINT('Ctrl Pts',(-54.3677308097131,-89.8101650395011,
179.76922598522));
#42417=CARTESIAN_POINT('Ctrl Pts',(-56.0210657349583,-89.7281897192716,
179.975477717318));
#42418=CARTESIAN_POINT('Ctrl Pts',(-57.6744006602036,-89.6462143990421,
180.181729449417));
#42419=CARTESIAN_POINT('Ctrl Pts',(-58.9914160388036,-89.6000929894002,
179.158929658031));
#42420=CARTESIAN_POINT('Ctrl Pts',(-60.3084314174037,-89.5539715797584,
178.136129866644));
#42421=CARTESIAN_POINT('Ctrl Pts',(-60.5234590849016,-89.6253294223835,
176.483420797975));
#42422=CARTESIAN_POINT('Ctrl Pts',(-60.7384867523995,-89.6966872650085,
174.830711729305));
#42423=CARTESIAN_POINT('Ctrl Pts',(-59.7313879999336,-89.8983319488991,
173.516227941122));
#42424=CARTESIAN_POINT('Ctrl Pts',(-58.7242892474676,-90.0999766327898,
172.201744152939));
#42425=CARTESIAN_POINT('Ctrl Pts',(-57.0908304480564,-90.36839548233,171.99549242084));
#42426=CARTESIAN_POINT('Ctrl Pts',(-55.4573716486452,-90.6368143318702,
171.789240688742));
#42427=CARTESIAN_POINT('Ctrl Pts',(-54.1602323958791,-90.8693792708227,
172.812040480128));
#42428=CARTESIAN_POINT('Ctrl Pts',(-52.8630931431131,-91.1019442097752,
173.834840271514));
#42429=CARTESIAN_POINT('Ctrl Pts',(-52.6679416014493,-91.2170298964609,
175.487549340184));
#42430=CARTESIAN_POINT('Ctrl Pts',(-52.4727900597853,-91.3321155831465,
177.140258408853));
#42431=CARTESIAN_POINT('Ctrl Pts',(-53.4997649380853,-91.3169144285666,
178.454742197037));
#42432=CARTESIAN_POINT('Ctrl Pts',(-54.5267398163853,-91.3017132739867,
179.76922598522));
#42433=CARTESIAN_POINT('Ctrl Pts',(-56.1800747416305,-91.2197379537572,
179.975477717318));
#42434=CARTESIAN_POINT('Ctrl Pts',(-57.8334096668758,-91.1377626335277,
180.181729449417));
#42435=CARTESIAN_POINT('Ctrl Pts',(-59.1504250454758,-91.0916412238858,
179.158929658031));
#42436=CARTESIAN_POINT('Ctrl Pts',(-60.4674404240759,-91.045519814244,178.136129866644));
#42437=CARTESIAN_POINT('Ctrl Pts',(-60.6824680915738,-91.116877656869,176.483420797975));
#42438=CARTESIAN_POINT('Ctrl Pts',(-60.8974957590717,-91.1882354994941,
174.830711729305));
#42439=CARTESIAN_POINT('Ctrl Pts',(-59.8903970066058,-91.3898801833847,
173.516227941122));
#42440=CARTESIAN_POINT('Ctrl Pts',(-58.8832982541398,-91.5915248672754,
172.201744152939));
#42441=CARTESIAN_POINT('Ctrl Pts',(-57.2498394547286,-91.8599437168156,
171.99549242084));
#42442=CARTESIAN_POINT('Ctrl Pts',(-55.6163806553174,-92.1283625663558,
171.789240688742));
#42443=CARTESIAN_POINT('Ctrl Pts',(-54.3192414025514,-92.3609275053083,
172.812040480128));
#42444=CARTESIAN_POINT('Ctrl Pts',(-53.0221021497854,-92.5934924442608,
173.834840271514));
#42445=CARTESIAN_POINT('Ctrl Pts',(-52.8269506081215,-92.7085781309465,
175.487549340184));
#42446=CARTESIAN_POINT('Ctrl Pts',(-52.6317990664576,-92.8236638176322,
177.140258408853));
#42447=CARTESIAN_POINT('Ctrl Pts',(-53.6587739447575,-92.8084626630522,
178.454742197037));
#42448=CARTESIAN_POINT('Ctrl Pts',(-54.6857488230575,-92.7932615084723,
179.76922598522));
#42449=CARTESIAN_POINT('Ctrl Pts',(-56.3390837483028,-92.7112861882428,
179.975477717318));
#42450=CARTESIAN_POINT('Ctrl Pts',(-57.992418673548,-92.6293108680132,180.181729449417));
#42451=CARTESIAN_POINT('Ctrl Pts',(-59.3094340521481,-92.5831894583715,
179.158929658031));
#42452=CARTESIAN_POINT('Ctrl Pts',(-60.6264494307481,-92.5370680487296,
178.136129866644));
#42453=CARTESIAN_POINT('Ctrl Pts',(-60.841477098246,-92.6084258913547,176.483420797975));
#42454=CARTESIAN_POINT('Ctrl Pts',(-61.056504765744,-92.6797837339797,174.830711729305));
#42455=CARTESIAN_POINT('Ctrl Pts',(-60.049406013278,-92.8814284178703,173.516227941122));
#42456=CARTESIAN_POINT('Ctrl Pts',(-59.0423072608121,-93.083073101761,172.201744152939));
#42457=CARTESIAN_POINT('Ctrl Pts',(-57.4088484614008,-93.3514919513012,
171.99549242084));
#42458=CARTESIAN_POINT('Ctrl Pts',(-55.7753896619896,-93.6199108008414,
171.789240688742));
#42459=CARTESIAN_POINT('Ctrl Pts',(-54.4782504092236,-93.8524757397939,
172.812040480128));
#42460=CARTESIAN_POINT('Ctrl Pts',(-53.1811111564576,-94.0850406787465,
173.834840271514));
#42461=CARTESIAN_POINT('Ctrl Pts',(-52.9859596147937,-94.2001263654321,
175.487549340184));
#42462=CARTESIAN_POINT('Ctrl Pts',(-52.7908080731298,-94.3152120521177,
177.140258408853));
#42463=CARTESIAN_POINT('Ctrl Pts',(-53.8177829514298,-94.3000108975378,
178.454742197037));
#42464=CARTESIAN_POINT('Ctrl Pts',(-54.8447578297298,-94.2848097429579,
179.76922598522));
#42465=CARTESIAN_POINT('Ctrl Pts',(-56.498092754975,-94.2028344227284,179.975477717318));
#42466=CARTESIAN_POINT('Ctrl Pts',(-58.1514276802203,-94.1208591024989,
180.181729449417));
#42467=CARTESIAN_POINT('Ctrl Pts',(-59.4684430588203,-94.074737692857,179.158929658031));
#42468=CARTESIAN_POINT('Ctrl Pts',(-60.7854584374203,-94.0286162832152,
178.136129866644));
#42469=CARTESIAN_POINT('Ctrl Pts',(-61.0004861049183,-94.0999741258402,
176.483420797975));
#42470=CARTESIAN_POINT('Ctrl Pts',(-61.2155137724162,-94.1713319684653,
174.830711729305));
#42471=CARTESIAN_POINT('Ctrl Pts',(-60.2084150199502,-94.372976652356,173.516227941122));
#42472=CARTESIAN_POINT('Ctrl Pts',(-59.2013162674843,-94.5746213362466,
172.201744152939));
#42473=CARTESIAN_POINT('Ctrl Pts',(-57.5678574680731,-94.8430401857868,
171.99549242084));
#42474=CARTESIAN_POINT('Ctrl Pts',(-55.9343986686618,-95.111459035327,171.789240688742));
#42475=CARTESIAN_POINT('Ctrl Pts',(-54.6372594158958,-95.3440239742795,
172.812040480128));
#42476=CARTESIAN_POINT('Ctrl Pts',(-53.3401201631298,-95.5765889132321,
173.834840271514));
#42477=CARTESIAN_POINT('Ctrl Pts',(-53.1449686214659,-95.6916745999177,
175.487549340184));
#42478=CARTESIAN_POINT('Ctrl Pts',(-52.949817079802,-95.8067602866033,177.140258408853));
#42479=CARTESIAN_POINT('Ctrl Pts',(-53.976791958102,-95.7915591320234,178.454742197037));
#42480=CARTESIAN_POINT('Ctrl Pts',(-55.003766836402,-95.7763579774435,179.76922598522));
#42481=CARTESIAN_POINT('Ctrl Pts',(-56.6571017616472,-95.694382657214,179.975477717318));
#42482=CARTESIAN_POINT('Ctrl Pts',(-58.3104366868925,-95.6124073369845,
180.181729449417));
#42483=CARTESIAN_POINT('Ctrl Pts',(-59.6274520654925,-95.5662859273426,
179.158929658031));
#42484=CARTESIAN_POINT('Ctrl Pts',(-60.9444674440926,-95.5201645177008,
178.136129866644));
#42485=CARTESIAN_POINT('Ctrl Pts',(-61.1594951115905,-95.5915223603259,
176.483420797975));
#42486=CARTESIAN_POINT('Ctrl Pts',(-61.3745227790884,-95.6628802029509,
174.830711729305));
#42487=CARTESIAN_POINT('Ctrl Pts',(-60.3674240266225,-95.8645248868416,
173.516227941122));
#42488=CARTESIAN_POINT('Ctrl Pts',(-59.3603252741565,-96.0661695707322,
172.201744152939));
#42489=CARTESIAN_POINT('Ctrl Pts',(-57.7268664747453,-96.3345884202724,
171.99549242084));
#42490=CARTESIAN_POINT('Ctrl Pts',(-56.0934076753341,-96.6030072698126,
171.789240688742));
#42491=CARTESIAN_POINT('Ctrl Pts',(-54.7962684225681,-96.8355722087651,
172.812040480128));
#42492=CARTESIAN_POINT('Ctrl Pts',(-53.4991291698021,-97.0681371477177,
173.834840271514));
#42493=CARTESIAN_POINT('Ctrl Pts',(-53.3039776281381,-97.1832228344033,
175.487549340184));
#42494=CARTESIAN_POINT('Ctrl Pts',(-53.1088260864743,-97.298308521089,177.140258408853));
#42495=CARTESIAN_POINT('Ctrl Pts',(-54.1358009647742,-97.283107366509,178.454742197037));
#42496=CARTESIAN_POINT('Ctrl Pts',(-55.1627758430742,-97.2679062119291,
179.76922598522));
#42497=CARTESIAN_POINT('Ctrl Pts',(-56.8161107683195,-97.1859308916996,
179.975477717318));
#42498=CARTESIAN_POINT('Ctrl Pts',(-58.4694456935647,-97.1039555714701,
180.181729449417));
#42499=CARTESIAN_POINT('Ctrl Pts',(-59.7864610721647,-97.0578341618282,
179.158929658031));
#42500=CARTESIAN_POINT('Ctrl Pts',(-61.1034764507648,-97.0117127521864,
178.136129866644));
#42501=CARTESIAN_POINT('Ctrl Pts',(-61.3185041182627,-97.0830705948115,
176.483420797975));
#42502=CARTESIAN_POINT('Ctrl Pts',(-61.5335317857606,-97.1544284374365,
174.830711729305));
#42503=CARTESIAN_POINT('Ctrl Pts',(-60.5264330332947,-97.3560731213272,
173.516227941122));
#42504=CARTESIAN_POINT('Ctrl Pts',(-59.5193342808287,-97.5577178052177,
172.201744152939));
#42505=CARTESIAN_POINT('Ctrl Pts',(-57.8858754814175,-97.826136654758,171.99549242084));
#42506=CARTESIAN_POINT('Ctrl Pts',(-56.2524166820063,-98.0945555042982,
171.789240688742));
#42507=CARTESIAN_POINT('Ctrl Pts',(-54.9552774292403,-98.3271204432507,
172.812040480128));
#42508=CARTESIAN_POINT('Ctrl Pts',(-53.6581381764743,-98.5596853822032,
173.834840271514));
#42509=CARTESIAN_POINT('Ctrl Pts',(-53.4629866348104,-98.6747710688889,
175.487549340184));
#42510=CARTESIAN_POINT('Ctrl Pts',(-53.2678350931465,-98.7898567555745,
177.140258408853));
#42511=CARTESIAN_POINT('Ctrl Pts',(-54.2948099714464,-98.7746556009946,
178.454742197037));
#42512=CARTESIAN_POINT('Ctrl Pts',(-55.3217848497464,-98.7594544464147,
179.76922598522));
#42513=CARTESIAN_POINT('Ctrl Pts',(-56.9751197749917,-98.6774791261852,
179.975477717318));
#42514=CARTESIAN_POINT('Ctrl Pts',(-58.6284547002369,-98.5955038059557,
180.181729449417));
#42515=CARTESIAN_POINT('Ctrl Pts',(-59.945470078837,-98.5493823963139,179.158929658031));
#42516=CARTESIAN_POINT('Ctrl Pts',(-61.262485457437,-98.503260986672,178.136129866644));
#42517=CARTESIAN_POINT('Ctrl Pts',(-61.4775131249349,-98.5746188292971,
176.483420797975));
#42518=CARTESIAN_POINT('Ctrl Pts',(-61.6925407924329,-98.6459766719221,
174.830711729305));
#42519=CARTESIAN_POINT('Ctrl Pts',(-60.6854420399669,-98.8476213558127,
173.516227941122));
#42520=CARTESIAN_POINT('Ctrl Pts',(-59.678343287501,-99.0492660397034,172.201744152939));
#42521=CARTESIAN_POINT('Ctrl Pts',(-58.0448844880897,-99.3176848892436,
171.99549242084));
#42522=CARTESIAN_POINT('Ctrl Pts',(-56.4114256886785,-99.5861037387838,
171.789240688742));
#42523=CARTESIAN_POINT('Ctrl Pts',(-55.1142864359125,-99.8186686777363,
172.812040480128));
#42524=CARTESIAN_POINT('Ctrl Pts',(-53.8171471831465,-100.051233616689,
173.834840271514));
#42525=CARTESIAN_POINT('Ctrl Pts',(-53.6219956414826,-100.166319303375,
175.487549340184));
#42526=CARTESIAN_POINT('Ctrl Pts',(-53.4268440998187,-100.28140499006,177.140258408853));
#42527=CARTESIAN_POINT('Ctrl Pts',(-54.4538189781187,-100.26620383548,178.454742197037));
#42528=CARTESIAN_POINT('Ctrl Pts',(-55.4807938564187,-100.2510026809,179.76922598522));
#42529=CARTESIAN_POINT('Ctrl Pts',(-57.1341287816639,-100.169027360671,
179.975477717318));
#42530=CARTESIAN_POINT('Ctrl Pts',(-58.7874637069092,-100.087052040441,
180.181729449417));
#42531=CARTESIAN_POINT('Ctrl Pts',(-60.1044790855092,-100.040930630799,
179.158929658031));
#42532=CARTESIAN_POINT('Ctrl Pts',(-61.4214944641092,-99.9948092211576,
178.136129866644));
#42533=CARTESIAN_POINT('Ctrl Pts',(-61.6365221316072,-100.066167063783,
176.483420797975));
#42534=CARTESIAN_POINT('Ctrl Pts',(-61.8515497991051,-100.137524906408,
174.830711729305));
#42535=CARTESIAN_POINT('Ctrl Pts',(-60.8444510466391,-100.339169590298,
173.516227941122));
#42536=CARTESIAN_POINT('Ctrl Pts',(-59.8373522941732,-100.540814274189,
172.201744152939));
#42537=CARTESIAN_POINT('Ctrl Pts',(-58.203893494762,-100.809233123729,171.99549242084));
#42538=CARTESIAN_POINT('Ctrl Pts',(-56.5704346953508,-101.077651973269,
171.789240688742));
#42539=CARTESIAN_POINT('Ctrl Pts',(-55.2732954425847,-101.310216912222,
172.812040480128));
#42540=CARTESIAN_POINT('Ctrl Pts',(-53.9761561898187,-101.542781851174,
173.834840271514));
#42541=CARTESIAN_POINT('Ctrl Pts',(-53.7810046481548,-101.65786753786,175.487549340184));
#42542=CARTESIAN_POINT('Ctrl Pts',(-53.5858531064909,-101.772953224546,
177.140258408853));
#42543=CARTESIAN_POINT('Ctrl Pts',(-54.6128279847909,-101.757752069966,
178.454742197037));
#42544=CARTESIAN_POINT('Ctrl Pts',(-55.6398028630909,-101.742550915386,
179.76922598522));
#42545=CARTESIAN_POINT('Ctrl Pts',(-57.2931377883361,-101.660575595156,
179.975477717318));
#42546=CARTESIAN_POINT('Ctrl Pts',(-58.9464727135814,-101.578600274927,
180.181729449417));
#42547=CARTESIAN_POINT('Ctrl Pts',(-60.2634880921814,-101.532478865285,
179.158929658031));
#42548=CARTESIAN_POINT('Ctrl Pts',(-61.5805034707815,-101.486357455643,
178.136129866644));
#42549=CARTESIAN_POINT('Ctrl Pts',(-61.7955311382794,-101.557715298268,
176.483420797975));
#42550=CARTESIAN_POINT('Ctrl Pts',(-62.0105588057773,-101.629073140893,
174.830711729305));
#42551=CARTESIAN_POINT('Ctrl Pts',(-61.0034600533114,-101.830717824784,
173.516227941122));
#42552=CARTESIAN_POINT('Ctrl Pts',(-59.9963613008454,-102.032362508675,
172.201744152939));
#42553=CARTESIAN_POINT('Ctrl Pts',(-58.3629025014342,-102.300781358215,
171.99549242084));
#42554=CARTESIAN_POINT('Ctrl Pts',(-56.729443702023,-102.569200207755,171.789240688742));
#42555=CARTESIAN_POINT('Ctrl Pts',(-55.432304449257,-102.801765146708,172.812040480128));
#42556=CARTESIAN_POINT('Ctrl Pts',(-54.135165196491,-103.03433008566,173.834840271514));
#42557=CARTESIAN_POINT('Ctrl Pts',(-53.9400136548271,-103.149415772346,
175.487549340184));
#42558=CARTESIAN_POINT('Ctrl Pts',(-53.7448621131632,-103.264501459031,
177.140258408853));
#42559=CARTESIAN_POINT('Ctrl Pts',(-54.7718369914631,-103.249300304451,
178.454742197037));
#42560=CARTESIAN_POINT('Ctrl Pts',(-55.7988118697631,-103.234099149872,
179.76922598522));
#42561=CARTESIAN_POINT('Ctrl Pts',(-57.4521467950084,-103.152123829642,
179.975477717318));
#42562=CARTESIAN_POINT('Ctrl Pts',(-59.1054817202536,-103.070148509412,
180.181729449417));
#42563=CARTESIAN_POINT('Ctrl Pts',(-60.4224970988536,-103.024027099771,
179.158929658031));
#42564=CARTESIAN_POINT('Ctrl Pts',(-61.7395124774537,-102.977905690129,
178.136129866644));
#42565=CARTESIAN_POINT('Ctrl Pts',(-61.9545401449516,-103.049263532754,
176.483420797975));
#42566=CARTESIAN_POINT('Ctrl Pts',(-62.1695678124496,-103.120621375379,
174.830711729305));
#42567=CARTESIAN_POINT('Ctrl Pts',(-61.1624690599836,-103.32226605927,173.516227941122));
#42568=CARTESIAN_POINT('Ctrl Pts',(-60.1553703075177,-103.52391074316,172.201744152939));
#42569=CARTESIAN_POINT('Ctrl Pts',(-58.5219115081064,-103.7923295927,171.99549242084));
#42570=CARTESIAN_POINT('Ctrl Pts',(-56.8884527086952,-104.060748442241,
171.789240688742));
#42571=CARTESIAN_POINT('Ctrl Pts',(-55.5913134559292,-104.293313381193,
172.812040480128));
#42572=CARTESIAN_POINT('Ctrl Pts',(-54.2941742031632,-104.525878320146,
173.834840271514));
#42573=CARTESIAN_POINT('Ctrl Pts',(-54.0990226614993,-104.640964006831,
175.487549340184));
#42574=CARTESIAN_POINT('Ctrl Pts',(-53.9038711198354,-104.756049693517,
177.140258408853));
#42575=CARTESIAN_POINT('Ctrl Pts',(-54.9308459981354,-104.740848538937,
178.454742197037));
#42576=CARTESIAN_POINT('Ctrl Pts',(-55.9578208764353,-104.725647384357,
179.76922598522));
#42577=CARTESIAN_POINT('Ctrl Pts',(-57.6111558016806,-104.643672064128,
179.975477717318));
#42578=CARTESIAN_POINT('Ctrl Pts',(-59.2644907269258,-104.561696743898,
180.181729449417));
#42579=CARTESIAN_POINT('Ctrl Pts',(-60.5815061055259,-104.515575334256,
179.158929658031));
#42580=CARTESIAN_POINT('Ctrl Pts',(-61.8985214841259,-104.469453924614,
178.136129866644));
#42581=CARTESIAN_POINT('Ctrl Pts',(-62.1135491516238,-104.540811767239,
176.483420797975));
#42582=CARTESIAN_POINT('Ctrl Pts',(-62.3285768191218,-104.612169609865,
174.830711729305));
#42583=CARTESIAN_POINT('Ctrl Pts',(-61.3214780666558,-104.813814293755,
173.516227941122));
#42584=CARTESIAN_POINT('Ctrl Pts',(-60.3143793141899,-105.015458977646,
172.201744152939));
#42585=CARTESIAN_POINT('Ctrl Pts',(-58.6809205147787,-105.283877827186,
171.99549242084));
#42586=CARTESIAN_POINT('Ctrl Pts',(-57.0474617153674,-105.552296676726,
171.789240688742));
#42587=CARTESIAN_POINT('Ctrl Pts',(-55.7503224626014,-105.784861615679,
172.812040480128));
#42588=CARTESIAN_POINT('Ctrl Pts',(-54.4531832098354,-106.017426554631,
173.834840271514));
#42589=CARTESIAN_POINT('Ctrl Pts',(-54.2580316681715,-106.132512241317,
175.487549340184));
#42590=CARTESIAN_POINT('Ctrl Pts',(-54.0628801265076,-106.247597928003,
177.140258408853));
#42591=CARTESIAN_POINT('Ctrl Pts',(-55.0898550048076,-106.232396773423,
178.454742197037));
#42592=CARTESIAN_POINT('Ctrl Pts',(-56.1168298831076,-106.217195618843,
179.76922598522));
#42593=CARTESIAN_POINT('Ctrl Pts',(-57.7701648083528,-106.135220298613,
179.975477717318));
#42594=CARTESIAN_POINT('Ctrl Pts',(-59.4234997335981,-106.053244978384,
180.181729449417));
#42595=CARTESIAN_POINT('Ctrl Pts',(-60.7405151121981,-106.007123568742,
179.158929658031));
#42596=CARTESIAN_POINT('Ctrl Pts',(-62.0575304907981,-105.9610021591,178.136129866644));
#42597=CARTESIAN_POINT('Ctrl Pts',(-62.2725581582961,-106.032360001725,
176.483420797975));
#42598=CARTESIAN_POINT('Ctrl Pts',(-62.487585825794,-106.10371784435,174.830711729305));
#42599=CARTESIAN_POINT('Ctrl Pts',(-61.480487073328,-106.305362528241,173.516227941122));
#42600=CARTESIAN_POINT('Ctrl Pts',(-60.4733883208621,-106.507007212131,
172.201744152939));
#42601=CARTESIAN_POINT('Ctrl Pts',(-58.8399295214509,-106.775426061672,
171.99549242084));
#42602=CARTESIAN_POINT('Ctrl Pts',(-57.2064707220397,-107.043844911212,
171.789240688742));
#42603=CARTESIAN_POINT('Ctrl Pts',(-55.9093314692737,-107.276409850164,
172.812040480128));
#42604=CARTESIAN_POINT('Ctrl Pts',(-54.6121922165077,-107.508974789117,
173.834840271514));
#42605=CARTESIAN_POINT('Ctrl Pts',(-54.4170406748437,-107.624060475802,
175.487549340184));
#42606=CARTESIAN_POINT('Ctrl Pts',(-54.2218891331799,-107.739146162488,
177.140258408853));
#42607=CARTESIAN_POINT('Ctrl Pts',(-55.2488640114798,-107.723945007908,
178.454742197037));
#42608=CARTESIAN_POINT('Ctrl Pts',(-56.2758388897798,-107.708743853328,
179.76922598522));
#42609=CARTESIAN_POINT('Ctrl Pts',(-57.929173815025,-107.626768533099,179.975477717318));
#42610=CARTESIAN_POINT('Ctrl Pts',(-59.5825087402703,-107.544793212869,
180.181729449417));
#42611=CARTESIAN_POINT('Ctrl Pts',(-60.8995241188703,-107.498671803227,
179.158929658031));
#42612=CARTESIAN_POINT('Ctrl Pts',(-62.2165394974704,-107.452550393586,
178.136129866644));
#42613=CARTESIAN_POINT('Ctrl Pts',(-62.4315671649683,-107.523908236211,
176.483420797975));
#42614=CARTESIAN_POINT('Ctrl Pts',(-62.6465948324662,-107.595266078836,
174.830711729305));
#42615=CARTESIAN_POINT('Ctrl Pts',(-61.6394960800003,-107.796910762726,
173.516227941122));
#42616=CARTESIAN_POINT('Ctrl Pts',(-60.6323973275343,-107.998555446617,
172.201744152939));
#42617=CARTESIAN_POINT('Ctrl Pts',(-58.9989385281231,-108.266974296157,
171.99549242084));
#42618=CARTESIAN_POINT('Ctrl Pts',(-57.3654797287119,-108.535393145697,
171.789240688742));
#42619=CARTESIAN_POINT('Ctrl Pts',(-56.0683404759459,-108.76795808465,172.812040480128));
#42620=CARTESIAN_POINT('Ctrl Pts',(-54.7712012231799,-109.000523023602,
173.834840271514));
#42621=CARTESIAN_POINT('Ctrl Pts',(-54.576049681516,-109.115608710288,175.487549340184));
#42622=CARTESIAN_POINT('Ctrl Pts',(-54.3808981398521,-109.230694396974,
177.140258408853));
#42623=CARTESIAN_POINT('Ctrl Pts',(-55.407873018152,-109.215493242394,178.454742197037));
#42624=CARTESIAN_POINT('Ctrl Pts',(-56.434847896452,-109.200292087814,179.76922598522));
#42625=CARTESIAN_POINT('Ctrl Pts',(-58.0881828216973,-109.118316767584,
179.975477717318));
#42626=CARTESIAN_POINT('Ctrl Pts',(-59.7415177469425,-109.036341447355,
180.181729449417));
#42627=CARTESIAN_POINT('Ctrl Pts',(-61.0585331255426,-108.990220037713,
179.158929658031));
#42628=CARTESIAN_POINT('Ctrl Pts',(-62.3755485041426,-108.944098628071,
178.136129866644));
#42629=CARTESIAN_POINT('Ctrl Pts',(-62.5905761716405,-109.015456470696,
176.483420797975));
#42630=CARTESIAN_POINT('Ctrl Pts',(-62.8056038391385,-109.086814313321,
174.830711729305));
#42631=CARTESIAN_POINT('Ctrl Pts',(-61.7985050866725,-109.288458997212,
173.516227941122));
#42632=CARTESIAN_POINT('Ctrl Pts',(-60.7914063342066,-109.490103681103,
172.201744152939));
#42633=CARTESIAN_POINT('Ctrl Pts',(-59.1579475347953,-109.758522530643,
171.99549242084));
#42634=CARTESIAN_POINT('Ctrl Pts',(-57.5244887353841,-110.026941380183,
171.789240688742));
#42635=CARTESIAN_POINT('Ctrl Pts',(-56.2273494826181,-110.259506319136,
172.812040480128));
#42636=CARTESIAN_POINT('Ctrl Pts',(-54.9302102298521,-110.492071258088,
173.834840271514));
#42637=CARTESIAN_POINT('Ctrl Pts',(-54.7350586881882,-110.607156944774,
175.487549340184));
#42638=CARTESIAN_POINT('Ctrl Pts',(-54.5399071465243,-110.722242631459,
177.140258408853));
#42639=CARTESIAN_POINT('Ctrl Pts',(-55.5668820248243,-110.707041476879,
178.454742197037));
#42640=CARTESIAN_POINT('Ctrl Pts',(-56.5938569031242,-110.691840322299,
179.76922598522));
#42641=CARTESIAN_POINT('Ctrl Pts',(-58.2471918283695,-110.60986500207,179.975477717318));
#42642=CARTESIAN_POINT('Ctrl Pts',(-59.9005267536148,-110.52788968184,180.181729449417));
#42643=CARTESIAN_POINT('Ctrl Pts',(-61.2175421322148,-110.481768272199,
179.158929658031));
#42644=CARTESIAN_POINT('Ctrl Pts',(-62.5345575108148,-110.435646862557,
178.136129866644));
#42645=CARTESIAN_POINT('Ctrl Pts',(-62.7495851783128,-110.507004705182,
176.483420797975));
#42646=CARTESIAN_POINT('Ctrl Pts',(-62.9646128458107,-110.578362547807,
174.830711729305));
#42647=CARTESIAN_POINT('Ctrl Pts',(-61.9575140933447,-110.780007231698,
173.516227941122));
#42648=CARTESIAN_POINT('Ctrl Pts',(-60.9504153408788,-110.981651915588,
172.201744152939));
#42649=CARTESIAN_POINT('Ctrl Pts',(-59.3169565414675,-111.250070765128,
171.99549242084));
#42650=CARTESIAN_POINT('Ctrl Pts',(-57.6834977420563,-111.518489614669,
171.789240688742));
#42651=CARTESIAN_POINT('Ctrl Pts',(-56.3863584892903,-111.751054553621,
172.812040480128));
#42652=CARTESIAN_POINT('Ctrl Pts',(-55.0892192365243,-111.983619492574,
173.834840271514));
#42653=CARTESIAN_POINT('Ctrl Pts',(-54.8940676948604,-112.098705179259,
175.487549340184));
#42654=CARTESIAN_POINT('Ctrl Pts',(-54.6989161531965,-112.213790865945,
177.140258408853));
#42655=CARTESIAN_POINT('Ctrl Pts',(-55.7258910314965,-112.198589711365,
178.454742197037));
#42656=CARTESIAN_POINT('Ctrl Pts',(-56.7528659097965,-112.183388556785,
179.76922598522));
#42657=CARTESIAN_POINT('Ctrl Pts',(-58.4062008350417,-112.101413236556,
179.975477717318));
#42658=CARTESIAN_POINT('Ctrl Pts',(-60.059535760287,-112.019437916326,180.181729449417));
#42659=CARTESIAN_POINT('Ctrl Pts',(-61.376551138887,-111.973316506684,179.158929658031));
#42660=CARTESIAN_POINT('Ctrl Pts',(-62.6935665174871,-111.927195097042,
178.136129866644));
#42661=CARTESIAN_POINT('Ctrl Pts',(-62.908594184985,-111.998552939667,176.483420797975));
#42662=CARTESIAN_POINT('Ctrl Pts',(-63.1236218524829,-112.069910782293,
174.830711729305));
#42663=CARTESIAN_POINT('Ctrl Pts',(-62.116523100017,-112.271555466183,173.516227941122));
#42664=CARTESIAN_POINT('Ctrl Pts',(-61.109424347551,-112.473200150074,172.201744152939));
#42665=CARTESIAN_POINT('Ctrl Pts',(-59.4759655481398,-112.741618999614,
171.99549242084));
#42666=CARTESIAN_POINT('Ctrl Pts',(-57.8425067487286,-113.010037849154,
171.789240688742));
#42667=CARTESIAN_POINT('Ctrl Pts',(-56.5453674959626,-113.242602788107,
172.812040480128));
#42668=CARTESIAN_POINT('Ctrl Pts',(-55.2482282431966,-113.475167727059,
173.834840271514));
#42669=CARTESIAN_POINT('Ctrl Pts',(-55.0530767015326,-113.590253413745,
175.487549340184));
#42670=CARTESIAN_POINT('Ctrl Pts',(-54.8579251598688,-113.705339100431,
177.140258408853));
#42671=CARTESIAN_POINT('Ctrl Pts',(-55.8849000381687,-113.690137945851,
178.454742197037));
#42672=CARTESIAN_POINT('Ctrl Pts',(-56.9118749164687,-113.674936791271,
179.76922598522));
#42673=CARTESIAN_POINT('Ctrl Pts',(-58.565209841714,-113.592961471041,179.975477717318));
#42674=CARTESIAN_POINT('Ctrl Pts',(-60.2185447669592,-113.510986150812,
180.181729449417));
#42675=CARTESIAN_POINT('Ctrl Pts',(-61.5355601455592,-113.46486474117,179.158929658031));
#42676=CARTESIAN_POINT('Ctrl Pts',(-62.8525755241593,-113.418743331528,
178.136129866644));
#42677=CARTESIAN_POINT('Ctrl Pts',(-63.0676031916572,-113.490101174153,
176.483420797975));
#42678=CARTESIAN_POINT('Ctrl Pts',(-63.2826308591551,-113.561459016778,
174.830711729305));
#42679=CARTESIAN_POINT('Ctrl Pts',(-62.2755321066892,-113.763103700669,
173.516227941122));
#42680=CARTESIAN_POINT('Ctrl Pts',(-61.2684333542232,-113.964748384559,
172.201744152939));
#42681=CARTESIAN_POINT('Ctrl Pts',(-59.634974554812,-114.2331672341,171.99549242084));
#42682=CARTESIAN_POINT('Ctrl Pts',(-58.0015157554008,-114.50158608364,171.789240688742));
#42683=CARTESIAN_POINT('Ctrl Pts',(-56.7043765026348,-114.734151022592,
172.812040480128));
#42684=CARTESIAN_POINT('Ctrl Pts',(-55.4072372498688,-114.966715961545,
173.834840271514));
#42685=CARTESIAN_POINT('Ctrl Pts',(-55.2120857082049,-115.08180164823,175.487549340184));
#42686=CARTESIAN_POINT('Ctrl Pts',(-55.016934166541,-115.196887334916,177.140258408853));
#42687=CARTESIAN_POINT('Ctrl Pts',(-56.043909044841,-115.181686180336,178.454742197037));
#42688=CARTESIAN_POINT('Ctrl Pts',(-57.0708839231409,-115.166485025756,
179.76922598522));
#42689=CARTESIAN_POINT('Ctrl Pts',(-58.7242188483862,-115.084509705527,
179.975477717318));
#42690=CARTESIAN_POINT('Ctrl Pts',(-60.3775537736314,-115.002534385297,
180.181729449417));
#42691=CARTESIAN_POINT('Ctrl Pts',(-61.6945691522315,-114.956412975655,
179.158929658031));
#42692=CARTESIAN_POINT('Ctrl Pts',(-63.0115845308315,-114.910291566014,
178.136129866644));
#42693=CARTESIAN_POINT('Ctrl Pts',(-63.2266121983294,-114.981649408639,
176.483420797975));
#42694=CARTESIAN_POINT('Ctrl Pts',(-63.4416398658274,-115.053007251264,
174.830711729305));
#42695=CARTESIAN_POINT('Ctrl Pts',(-62.4345411133614,-115.254651935154,
173.516227941122));
#42696=CARTESIAN_POINT('Ctrl Pts',(-61.4274423608955,-115.456296619045,
172.201744152939));
#42697=CARTESIAN_POINT('Ctrl Pts',(-59.7939835614843,-115.724715468585,
171.99549242084));
#42698=CARTESIAN_POINT('Ctrl Pts',(-58.160524762073,-115.993134318125,171.789240688742));
#42699=CARTESIAN_POINT('Ctrl Pts',(-56.863385509307,-116.225699257078,172.812040480128));
#42700=CARTESIAN_POINT('Ctrl Pts',(-55.566246256541,-116.45826419603,173.834840271514));
#42701=CARTESIAN_POINT('Ctrl Pts',(-55.3710947148771,-116.573349882716,
175.487549340184));
#42702=CARTESIAN_POINT('Ctrl Pts',(-55.1759431732132,-116.688435569402,
177.140258408853));
#42703=CARTESIAN_POINT('Ctrl Pts',(-56.2029180515132,-116.673234414822,
178.454742197037));
#42704=CARTESIAN_POINT('Ctrl Pts',(-57.2298929298132,-116.658033260242,
179.76922598522));
#42705=CARTESIAN_POINT('Ctrl Pts',(-58.8832278550584,-116.576057940012,
179.975477717318));
#42706=CARTESIAN_POINT('Ctrl Pts',(-60.5365627803037,-116.494082619783,
180.181729449417));
#42707=CARTESIAN_POINT('Ctrl Pts',(-61.8535781589037,-116.447961210141,
179.158929658031));
#42708=CARTESIAN_POINT('Ctrl Pts',(-63.1705935375037,-116.401839800499,
178.136129866644));
#42709=CARTESIAN_POINT('Ctrl Pts',(-63.3856212050017,-116.473197643124,
176.483420797975));
#42710=CARTESIAN_POINT('Ctrl Pts',(-63.6006488724996,-116.544555485749,
174.830711729305));
#42711=CARTESIAN_POINT('Ctrl Pts',(-62.5935501200336,-116.74620016964,173.516227941122));
#42712=CARTESIAN_POINT('Ctrl Pts',(-61.5864513675677,-116.947844853531,
172.201744152939));
#42713=CARTESIAN_POINT('Ctrl Pts',(-59.9529925681565,-117.216263703071,
171.99549242084));
#42714=CARTESIAN_POINT('Ctrl Pts',(-58.3195337687452,-117.484682552611,
171.789240688742));
#42715=CARTESIAN_POINT('Ctrl Pts',(-57.0223945159792,-117.717247491564,
172.812040480128));
#42716=CARTESIAN_POINT('Ctrl Pts',(-55.7252552632132,-117.949812430516,
173.834840271514));
#42717=CARTESIAN_POINT('Ctrl Pts',(-55.5301037215493,-118.064898117202,
175.487549340184));
#42718=CARTESIAN_POINT('Ctrl Pts',(-55.3349521798854,-118.179983803887,
177.140258408853));
#42719=CARTESIAN_POINT('Ctrl Pts',(-56.3619270581854,-118.164782649307,
178.454742197037));
#42720=CARTESIAN_POINT('Ctrl Pts',(-57.3889019364854,-118.149581494728,
179.76922598522));
#42721=CARTESIAN_POINT('Ctrl Pts',(-59.0422368617306,-118.067606174498,
179.975477717318));
#42722=CARTESIAN_POINT('Ctrl Pts',(-60.6955717869759,-117.985630854268,
180.181729449417));
#42723=CARTESIAN_POINT('Ctrl Pts',(-62.0125871655759,-117.939509444627,
179.158929658031));
#42724=CARTESIAN_POINT('Ctrl Pts',(-63.329602544176,-117.893388034985,178.136129866644));
#42725=CARTESIAN_POINT('Ctrl Pts',(-63.5446302116739,-117.96474587761,176.483420797975));
#42726=CARTESIAN_POINT('Ctrl Pts',(-63.7596578791718,-118.036103720235,
174.830711729305));
#42727=CARTESIAN_POINT('Ctrl Pts',(-62.7525591267059,-118.237748404126,
173.516227941122));
#42728=CARTESIAN_POINT('Ctrl Pts',(-61.7454603742399,-118.439393088016,
172.201744152939));
#42729=CARTESIAN_POINT('Ctrl Pts',(-60.1120015748287,-118.707811937556,
171.99549242084));
#42730=CARTESIAN_POINT('Ctrl Pts',(-58.4785427754175,-118.976230787097,
171.789240688742));
#42731=CARTESIAN_POINT('Ctrl Pts',(-57.1814035226515,-119.208795726049,
172.812040480128));
#42732=CARTESIAN_POINT('Ctrl Pts',(-55.8842642698855,-119.441360665002,
173.834840271514));
#42733=CARTESIAN_POINT('Ctrl Pts',(-55.6891127282216,-119.556446351687,
175.487549340184));
#42734=CARTESIAN_POINT('Ctrl Pts',(-55.4939611865577,-119.671532038373,
177.140258408853));
#42735=CARTESIAN_POINT('Ctrl Pts',(-56.5209360648576,-119.656330883793,
178.454742197037));
#42736=CARTESIAN_POINT('Ctrl Pts',(-57.5479109431576,-119.641129729213,
179.76922598522));
#42737=CARTESIAN_POINT('Ctrl Pts',(-59.2012458684029,-119.559154408984,
179.975477717318));
#42738=CARTESIAN_POINT('Ctrl Pts',(-60.8545807936481,-119.477179088754,
180.181729449417));
#42739=CARTESIAN_POINT('Ctrl Pts',(-62.1715961722481,-119.431057679112,
179.158929658031));
#42740=CARTESIAN_POINT('Ctrl Pts',(-63.4886115508482,-119.38493626947,178.136129866644));
#42741=CARTESIAN_POINT('Ctrl Pts',(-63.7036392183461,-119.456294112095,
176.483420797975));
#42742=CARTESIAN_POINT('Ctrl Pts',(-63.918666885844,-119.527651954721,174.830711729305));
#42743=CARTESIAN_POINT('Ctrl Pts',(-62.9115681333781,-119.729296638611,
173.516227941122));
#42744=CARTESIAN_POINT('Ctrl Pts',(-61.9044693809121,-119.930941322502,
172.201744152939));
#42745=CARTESIAN_POINT('Ctrl Pts',(-60.2710105815009,-120.199360172042,
171.99549242084));
#42746=CARTESIAN_POINT('Ctrl Pts',(-58.6375517820897,-120.467779021582,
171.789240688742));
#42747=CARTESIAN_POINT('Ctrl Pts',(-57.3404125293237,-120.700343960535,
172.812040480128));
#42748=CARTESIAN_POINT('Ctrl Pts',(-56.0432732765577,-120.932908899487,
173.834840271514));
#42749=CARTESIAN_POINT('Ctrl Pts',(-55.8481217348938,-121.047994586173,
175.487549340184));
#42750=CARTESIAN_POINT('Ctrl Pts',(-55.6529701932299,-121.163080272859,
177.140258408853));
#42751=CARTESIAN_POINT('Ctrl Pts',(-56.6799450715299,-121.147879118279,
178.454742197037));
#42752=CARTESIAN_POINT('Ctrl Pts',(-57.7069199498298,-121.132677963699,
179.76922598522));
#42753=CARTESIAN_POINT('Ctrl Pts',(-59.3602548750751,-121.050702643469,
179.975477717318));
#42754=CARTESIAN_POINT('Ctrl Pts',(-61.0135898003203,-120.96872732324,180.181729449417));
#42755=CARTESIAN_POINT('Ctrl Pts',(-62.3306051789204,-120.922605913598,
179.158929658031));
#42756=CARTESIAN_POINT('Ctrl Pts',(-63.6476205575204,-120.876484503956,
178.136129866644));
#42757=CARTESIAN_POINT('Ctrl Pts',(-63.8626482250183,-120.947842346581,
176.483420797975));
#42758=CARTESIAN_POINT('Ctrl Pts',(-64.0776758925163,-121.019200189206,
174.830711729305));
#42759=CARTESIAN_POINT('Ctrl Pts',(-63.0705771400503,-121.220844873097,
173.516227941122));
#42760=CARTESIAN_POINT('Ctrl Pts',(-62.0634783875844,-121.422489556987,
172.201744152939));
#42761=CARTESIAN_POINT('Ctrl Pts',(-60.4300195881731,-121.690908406528,
171.99549242084));
#42762=CARTESIAN_POINT('Ctrl Pts',(-58.7965607887619,-121.959327256068,
171.789240688742));
#42763=CARTESIAN_POINT('Ctrl Pts',(-57.4994215359959,-122.19189219502,172.812040480128));
#42764=CARTESIAN_POINT('Ctrl Pts',(-56.2022822832299,-122.424457133973,
173.834840271514));
#42765=CARTESIAN_POINT('Ctrl Pts',(-56.007130741566,-122.539542820658,175.487549340184));
#42766=CARTESIAN_POINT('Ctrl Pts',(-55.8119791999021,-122.654628507344,
177.140258408853));
#42767=CARTESIAN_POINT('Ctrl Pts',(-56.8389540782021,-122.639427352764,
178.454742197037));
#42768=CARTESIAN_POINT('Ctrl Pts',(-57.8659289565021,-122.624226198184,
179.76922598522));
#42769=CARTESIAN_POINT('Ctrl Pts',(-59.5192638817473,-122.542250877955,
179.975477717318));
#42770=CARTESIAN_POINT('Ctrl Pts',(-61.1725988069926,-122.460275557725,
180.181729449417));
#42771=CARTESIAN_POINT('Ctrl Pts',(-62.4896141855926,-122.414154148083,
179.158929658031));
#42772=CARTESIAN_POINT('Ctrl Pts',(-63.8066295641926,-122.368032738442,
178.136129866644));
#42773=CARTESIAN_POINT('Ctrl Pts',(-64.0216572316905,-122.439390581067,
176.483420797975));
#42774=CARTESIAN_POINT('Ctrl Pts',(-64.2366848991885,-122.510748423692,
174.830711729305));
#42775=CARTESIAN_POINT('Ctrl Pts',(-63.2295861467226,-122.712393107582,
173.516227941122));
#42776=CARTESIAN_POINT('Ctrl Pts',(-62.2224873942566,-122.914037791473,
172.201744152939));
#42777=CARTESIAN_POINT('Ctrl Pts',(-60.5890285948454,-123.182456641013,
171.99549242084));
#42778=CARTESIAN_POINT('Ctrl Pts',(-58.9555697954342,-123.450875490553,
171.789240688742));
#42779=CARTESIAN_POINT('Ctrl Pts',(-57.6584305426681,-123.683440429506,
172.812040480128));
#42780=CARTESIAN_POINT('Ctrl Pts',(-56.3612912899021,-123.916005368458,
173.834840271514));
#42781=CARTESIAN_POINT('Ctrl Pts',(-56.1661397482382,-124.031091055144,
175.487549340184));
#42782=CARTESIAN_POINT('Ctrl Pts',(-55.9709882065743,-124.14617674183,177.140258408853));
#42783=CARTESIAN_POINT('Ctrl Pts',(-56.9979630848743,-124.13097558725,178.454742197037));
#42784=CARTESIAN_POINT('Ctrl Pts',(-58.0249379631743,-124.11577443267,179.76922598522));
#42785=CARTESIAN_POINT('Ctrl Pts',(-59.6782728884195,-124.03379911244,179.975477717318));
#42786=CARTESIAN_POINT('Ctrl Pts',(-61.3316078136648,-123.951823792211,
180.181729449417));
#42787=CARTESIAN_POINT('Ctrl Pts',(-62.6486231922648,-123.905702382569,
179.158929658031));
#42788=CARTESIAN_POINT('Ctrl Pts',(-63.9656385708649,-123.859580972927,
178.136129866644));
#42789=CARTESIAN_POINT('Ctrl Pts',(-64.1806662383628,-123.930938815552,
176.483420797975));
#42790=CARTESIAN_POINT('Ctrl Pts',(-64.3956939058607,-124.002296658177,
174.830711729305));
#42791=CARTESIAN_POINT('Ctrl Pts',(-63.3885951533948,-124.203941342068,
173.516227941122));
#42792=CARTESIAN_POINT('Ctrl Pts',(-62.3814964009288,-124.405586025959,
172.201744152939));
#42793=CARTESIAN_POINT('Ctrl Pts',(-60.7480376015176,-124.674004875499,
171.99549242084));
#42794=CARTESIAN_POINT('Ctrl Pts',(-59.1145788021064,-124.942423725039,
171.789240688742));
#42795=CARTESIAN_POINT('Ctrl Pts',(-57.8174395493404,-125.174988663992,
172.812040480128));
#42796=CARTESIAN_POINT('Ctrl Pts',(-56.5203002965744,-125.407553602944,
173.834840271514));
#42797=CARTESIAN_POINT('Ctrl Pts',(-56.3251487549105,-125.52263928963,175.487549340184));
#42798=CARTESIAN_POINT('Ctrl Pts',(-56.1299972132466,-125.637724976315,
177.140258408853));
#42799=CARTESIAN_POINT('Ctrl Pts',(-57.1569720915465,-125.622523821735,
178.454742197037));
#42800=CARTESIAN_POINT('Ctrl Pts',(-58.1839469698465,-125.607322667156,
179.76922598522));
#42801=CARTESIAN_POINT('Ctrl Pts',(-59.8372818950918,-125.525347346926,
179.975477717318));
#42802=CARTESIAN_POINT('Ctrl Pts',(-61.490616820337,-125.443372026696,180.181729449417));
#42803=CARTESIAN_POINT('Ctrl Pts',(-62.8076321989371,-125.397250617055,
179.158929658031));
#42804=CARTESIAN_POINT('Ctrl Pts',(-64.1246475775371,-125.351129207413,
178.136129866644));
#42805=CARTESIAN_POINT('Ctrl Pts',(-64.339675245035,-125.422487050038,176.483420797975));
#42806=CARTESIAN_POINT('Ctrl Pts',(-64.5547029125329,-125.493844892663,
174.830711729305));
#42807=CARTESIAN_POINT('Ctrl Pts',(-63.547604160067,-125.695489576554,173.516227941122));
#42808=CARTESIAN_POINT('Ctrl Pts',(-62.5405054076011,-125.897134260444,
172.201744152939));
#42809=CARTESIAN_POINT('Ctrl Pts',(-60.9070466081898,-126.165553109984,
171.99549242084));
#42810=CARTESIAN_POINT('Ctrl Pts',(-59.2735878087786,-126.433971959525,
171.789240688742));
#42811=CARTESIAN_POINT('Ctrl Pts',(-57.9764485560126,-126.666536898477,
172.812040480128));
#42812=CARTESIAN_POINT('Ctrl Pts',(-56.6793093032466,-126.89910183743,173.834840271514));
#42813=CARTESIAN_POINT('Ctrl Pts',(-56.4841577615827,-127.014187524115,
175.487549340184));
#42814=CARTESIAN_POINT('Ctrl Pts',(-56.2890062199188,-127.129273210801,
177.140258408853));
#42815=CARTESIAN_POINT('Ctrl Pts',(-57.3159810982188,-127.114072056221,
178.454742197037));
#42816=CARTESIAN_POINT('Ctrl Pts',(-58.3429559765187,-127.098870901641,
179.76922598522));
#42817=CARTESIAN_POINT('Ctrl Pts',(-59.996290901764,-127.016895581412,179.975477717318));
#42818=CARTESIAN_POINT('Ctrl Pts',(-61.6496258270093,-126.934920261182,
180.181729449417));
#42819=CARTESIAN_POINT('Ctrl Pts',(-62.9666412056093,-126.88879885154,179.158929658031));
#42820=CARTESIAN_POINT('Ctrl Pts',(-64.2836565842093,-126.842677441898,
178.136129866644));
#42821=CARTESIAN_POINT('Ctrl Pts',(-64.4986842517073,-126.914035284523,
176.483420797975));
#42822=CARTESIAN_POINT('Ctrl Pts',(-64.7137119192052,-126.985393127149,
174.830711729305));
#42823=CARTESIAN_POINT('Ctrl Pts',(-63.7066131667392,-127.187037811039,
173.516227941122));
#42824=CARTESIAN_POINT('Ctrl Pts',(-62.6995144142733,-127.38868249493,172.201744152939));
#42825=CARTESIAN_POINT('Ctrl Pts',(-61.0660556148621,-127.65710134447,171.99549242084));
#42826=CARTESIAN_POINT('Ctrl Pts',(-59.4325968154509,-127.92552019401,171.789240688742));
#42827=CARTESIAN_POINT('Ctrl Pts',(-58.1354575626848,-128.158085132963,
172.812040480128));
#42828=CARTESIAN_POINT('Ctrl Pts',(-56.8383183099188,-128.390650071915,
173.834840271514));
#42829=CARTESIAN_POINT('Ctrl Pts',(-56.6431667682549,-128.505735758601,
175.487549340184));
#42830=CARTESIAN_POINT('Ctrl Pts',(-56.448015226591,-128.620821445287,177.140258408853));
#42831=CARTESIAN_POINT('Ctrl Pts',(-57.474990104891,-128.605620290707,178.454742197037));
#42832=CARTESIAN_POINT('Ctrl Pts',(-58.501964983191,-128.590419136127,179.76922598522));
#42833=CARTESIAN_POINT('Ctrl Pts',(-60.1552999084362,-128.508443815897,
179.975477717318));
#42834=CARTESIAN_POINT('Ctrl Pts',(-61.8086348336815,-128.426468495668,
180.181729449417));
#42835=CARTESIAN_POINT('Ctrl Pts',(-63.1256502122815,-128.380347086026,
179.158929658031));
#42836=CARTESIAN_POINT('Ctrl Pts',(-64.4426655908815,-128.334225676384,
178.136129866644));
#42837=CARTESIAN_POINT('Ctrl Pts',(-64.6576932583795,-128.405583519009,
176.483420797975));
#42838=CARTESIAN_POINT('Ctrl Pts',(-64.8727209258774,-128.476941361634,
174.830711729305));
#42839=CARTESIAN_POINT('Ctrl Pts',(-63.8656221734115,-128.678586045525,
173.516227941122));
#42840=CARTESIAN_POINT('Ctrl Pts',(-62.8585234209455,-128.880230729415,
172.201744152939));
#42841=CARTESIAN_POINT('Ctrl Pts',(-61.2250646215343,-129.148649578956,
171.99549242084));
#42842=CARTESIAN_POINT('Ctrl Pts',(-59.5916058221231,-129.417068428496,
171.789240688742));
#42843=CARTESIAN_POINT('Ctrl Pts',(-58.2944665693571,-129.649633367448,
172.812040480128));
#42844=CARTESIAN_POINT('Ctrl Pts',(-56.997327316591,-129.882198306401,173.834840271514));
#42845=CARTESIAN_POINT('Ctrl Pts',(-56.8021757749272,-129.997283993086,
175.487549340184));
#42846=CARTESIAN_POINT('Ctrl Pts',(-56.6070242332633,-130.112369679772,
177.140258408853));
#42847=CARTESIAN_POINT('Ctrl Pts',(-57.6339991115632,-130.097168525192,
178.454742197037));
#42848=CARTESIAN_POINT('Ctrl Pts',(-58.6609739898632,-130.081967370612,
179.76922598522));
#42849=CARTESIAN_POINT('Ctrl Pts',(-60.3143089151084,-129.999992050383,
179.975477717318));
#42850=CARTESIAN_POINT('Ctrl Pts',(-61.9676438403537,-129.918016730153,
180.181729449417));
#42851=CARTESIAN_POINT('Ctrl Pts',(-63.2846592189537,-129.871895320511,
179.158929658031));
#42852=CARTESIAN_POINT('Ctrl Pts',(-64.6016745975538,-129.82577391087,178.136129866644));
#42853=CARTESIAN_POINT('Ctrl Pts',(-64.8167022650517,-129.897131753495,
176.483420797975));
#42854=CARTESIAN_POINT('Ctrl Pts',(-65.0317299325496,-129.96848959612,174.830711729305));
#42855=CARTESIAN_POINT('Ctrl Pts',(-64.0246311800837,-130.17013428001,173.516227941122));
#42856=CARTESIAN_POINT('Ctrl Pts',(-63.0175324276178,-130.371778963901,
172.201744152939));
#42857=CARTESIAN_POINT('Ctrl Pts',(-61.3840736282065,-130.640197813441,
171.99549242084));
#42858=CARTESIAN_POINT('Ctrl Pts',(-59.7506148287953,-130.908616662981,
171.789240688742));
#42859=CARTESIAN_POINT('Ctrl Pts',(-58.4534755760293,-131.141181601934,
172.812040480128));
#42860=CARTESIAN_POINT('Ctrl Pts',(-57.1563363232633,-131.373746540886,
173.834840271514));
#42861=CARTESIAN_POINT('Ctrl Pts',(-56.9611847815994,-131.488832227572,
175.487549340184));
#42862=CARTESIAN_POINT('Ctrl Pts',(-56.7660332399355,-131.603917914258,
177.140258408853));
#42863=CARTESIAN_POINT('Ctrl Pts',(-57.7930081182354,-131.588716759678,
178.454742197037));
#42864=CARTESIAN_POINT('Ctrl Pts',(-58.8199829965354,-131.573515605098,
179.76922598522));
#42865=CARTESIAN_POINT('Ctrl Pts',(-60.4733179217807,-131.491540284868,
179.975477717318));
#42866=CARTESIAN_POINT('Ctrl Pts',(-61.5428145880944,-131.438512715943,
180.108896262184));
#42867=CARTESIAN_POINT('Ctrl Pts',(-62.5366952746482,-131.398006590211,
179.689905107434));
#42868=CARTESIAN_POINT('Ctrl Pts',(-50.1415580290747,-67.5188568440608,
175.487549340184));
#42869=CARTESIAN_POINT('Ctrl Pts',(-49.9464064874108,-67.6339425307465,
177.140258408853));
#42870=CARTESIAN_POINT('Ctrl Pts',(-50.9733813657108,-67.6187413761666,
178.454742197037));
#42871=CARTESIAN_POINT('Ctrl Pts',(-52.0003562440107,-67.6035402215866,
179.76922598522));
#42872=CARTESIAN_POINT('Ctrl Pts',(-53.653691169256,-67.5215649013571,179.975477717318));
#42873=CARTESIAN_POINT('Ctrl Pts',(-55.3070260945012,-67.4395895811276,
180.181729449417));
#42874=CARTESIAN_POINT('Ctrl Pts',(-56.6240414731013,-67.3934681714858,
179.158929658031));
#42875=CARTESIAN_POINT('Ctrl Pts',(-57.9410568517013,-67.347346761844,178.136129866644));
#42876=CARTESIAN_POINT('Ctrl Pts',(-58.1560845191993,-67.418704604469,176.483420797975));
#42877=CARTESIAN_POINT('Ctrl Pts',(-58.3711121866972,-67.4900624470941,
174.830711729305));
#42878=CARTESIAN_POINT('Ctrl Pts',(-57.3640134342312,-67.6917071309847,
173.516227941122));
#42879=CARTESIAN_POINT('Ctrl Pts',(-56.3569146817653,-67.8933518148753,
172.201744152939));
#42880=CARTESIAN_POINT('Ctrl Pts',(-54.7234558823541,-68.1617706644155,
171.99549242084));
#42881=CARTESIAN_POINT('Ctrl Pts',(-53.0899970829429,-68.4301895139558,
171.789240688742));
#42882=CARTESIAN_POINT('Ctrl Pts',(-51.7928578301768,-68.6627544529083,
172.812040480128));
#42883=CARTESIAN_POINT('Ctrl Pts',(-50.4957185774108,-68.8953193918608,
173.834840271514));
#42884=CARTESIAN_POINT('Ctrl Pts',(-50.3005670357469,-69.0104050785464,
175.487549340184));
#42885=CARTESIAN_POINT('Ctrl Pts',(-50.105415494083,-69.1254907652321,177.140258408853));
#42886=CARTESIAN_POINT('Ctrl Pts',(-51.132390372383,-69.1102896106521,178.454742197037));
#42887=CARTESIAN_POINT('Ctrl Pts',(-52.159365250683,-69.0950884560723,179.76922598522));
#42888=CARTESIAN_POINT('Ctrl Pts',(-53.8127001759282,-69.0131131358427,
179.975477717318));
#42889=CARTESIAN_POINT('Ctrl Pts',(-55.4660351011735,-68.9311378156132,
180.181729449417));
#42890=CARTESIAN_POINT('Ctrl Pts',(-56.7830504797735,-68.8850164059714,
179.158929658031));
#42891=CARTESIAN_POINT('Ctrl Pts',(-58.1000658583736,-68.8388949963296,
178.136129866644));
#42892=CARTESIAN_POINT('Ctrl Pts',(-58.3150935258715,-68.9102528389546,
176.483420797975));
#42893=CARTESIAN_POINT('Ctrl Pts',(-58.5301211933694,-68.9816106815797,
174.830711729305));
#42894=CARTESIAN_POINT('Ctrl Pts',(-57.5230224409035,-69.1832553654703,
173.516227941122));
#42895=CARTESIAN_POINT('Ctrl Pts',(-56.5159236884375,-69.3849000493609,
172.201744152939));
#42896=CARTESIAN_POINT('Ctrl Pts',(-54.8824648890263,-69.6533188989011,
171.99549242084));
#42897=CARTESIAN_POINT('Ctrl Pts',(-53.2490060896151,-69.9217377484414,
171.789240688742));
#42898=CARTESIAN_POINT('Ctrl Pts',(-51.9518668368491,-70.1543026873939,
172.812040480128));
#42899=CARTESIAN_POINT('Ctrl Pts',(-50.654727584083,-70.3868676263464,173.834840271514));
#42900=CARTESIAN_POINT('Ctrl Pts',(-50.4595760424191,-70.501953313032,175.487549340184));
#42901=CARTESIAN_POINT('Ctrl Pts',(-50.2644245007553,-70.6170389997177,
177.140258408853));
#42902=CARTESIAN_POINT('Ctrl Pts',(-51.2913993790552,-70.6018378451378,
178.454742197037));
#42903=CARTESIAN_POINT('Ctrl Pts',(-52.3183742573552,-70.5866366905578,
179.76922598522));
#42904=CARTESIAN_POINT('Ctrl Pts',(-53.9717091826004,-70.5046613703283,
179.975477717318));
#42905=CARTESIAN_POINT('Ctrl Pts',(-55.6250441078457,-70.4226860500988,
180.181729449417));
#42906=CARTESIAN_POINT('Ctrl Pts',(-56.9420594864457,-70.376564640457,179.158929658031));
#42907=CARTESIAN_POINT('Ctrl Pts',(-58.2590748650458,-70.3304432308151,
178.136129866644));
#42908=CARTESIAN_POINT('Ctrl Pts',(-58.4741025325437,-70.4018010734402,
176.483420797975));
#42909=CARTESIAN_POINT('Ctrl Pts',(-58.6891302000416,-70.4731589160653,
174.830711729305));
#42910=CARTESIAN_POINT('Ctrl Pts',(-57.6820314475757,-70.6748035999559,
173.516227941122));
#42911=CARTESIAN_POINT('Ctrl Pts',(-56.6749326951098,-70.8764482838465,
172.201744152939));
#42912=CARTESIAN_POINT('Ctrl Pts',(-55.0414738956985,-71.1448671333867,
171.99549242084));
#42913=CARTESIAN_POINT('Ctrl Pts',(-53.4080150962873,-71.413285982927,171.789240688742));
#42914=CARTESIAN_POINT('Ctrl Pts',(-52.1108758435213,-71.6458509218795,
172.812040480128));
#42915=CARTESIAN_POINT('Ctrl Pts',(-50.8137365907553,-71.878415860832,173.834840271514));
#42916=CARTESIAN_POINT('Ctrl Pts',(-50.6185850490914,-71.9935015475176,
175.487549340184));
#42917=CARTESIAN_POINT('Ctrl Pts',(-50.4234335074275,-72.1085872342033,
177.140258408853));
#42918=CARTESIAN_POINT('Ctrl Pts',(-51.4504083857275,-72.0933860796234,
178.454742197037));
#42919=CARTESIAN_POINT('Ctrl Pts',(-52.4773832640274,-72.0781849250434,
179.76922598522));
#42920=CARTESIAN_POINT('Ctrl Pts',(-54.1307181892727,-71.9962096048139,
179.975477717318));
#42921=CARTESIAN_POINT('Ctrl Pts',(-55.7840531145179,-71.9142342845844,
180.181729449417));
#42922=CARTESIAN_POINT('Ctrl Pts',(-57.101068493118,-71.8681128749426,179.158929658031));
#42923=CARTESIAN_POINT('Ctrl Pts',(-58.418083871718,-71.8219914653008,178.136129866644));
#42924=CARTESIAN_POINT('Ctrl Pts',(-58.6331115392159,-71.8933493079258,
176.483420797975));
#42925=CARTESIAN_POINT('Ctrl Pts',(-58.8481392067139,-71.9647071505509,
174.830711729305));
#42926=CARTESIAN_POINT('Ctrl Pts',(-57.8410404542479,-72.1663518344415,
173.516227941122));
#42927=CARTESIAN_POINT('Ctrl Pts',(-56.833941701782,-72.3679965183321,172.201744152939));
#42928=CARTESIAN_POINT('Ctrl Pts',(-55.2004829023707,-72.6364153678723,
171.99549242084));
#42929=CARTESIAN_POINT('Ctrl Pts',(-53.5670241029595,-72.9048342174126,
171.789240688742));
#42930=CARTESIAN_POINT('Ctrl Pts',(-52.2698848501935,-73.1373991563651,
172.812040480128));
#42931=CARTESIAN_POINT('Ctrl Pts',(-50.9727455974275,-73.3699640953176,
173.834840271514));
#42932=CARTESIAN_POINT('Ctrl Pts',(-50.7775940557636,-73.4850497820032,
175.487549340184));
#42933=CARTESIAN_POINT('Ctrl Pts',(-50.5824425140997,-73.6001354686889,
177.140258408853));
#42934=CARTESIAN_POINT('Ctrl Pts',(-51.6094173923997,-73.5849343141089,
178.454742197037));
#42935=CARTESIAN_POINT('Ctrl Pts',(-52.6363922706997,-73.5697331595291,
179.76922598522));
#42936=CARTESIAN_POINT('Ctrl Pts',(-54.2897271959449,-73.4877578392995,
179.975477717318));
#42937=CARTESIAN_POINT('Ctrl Pts',(-55.9430621211902,-73.40578251907,180.181729449417));
#42938=CARTESIAN_POINT('Ctrl Pts',(-57.2600774997902,-73.3596611094282,
179.158929658031));
#42939=CARTESIAN_POINT('Ctrl Pts',(-58.5770928783902,-73.3135396997863,
178.136129866644));
#42940=CARTESIAN_POINT('Ctrl Pts',(-58.7921205458882,-73.3848975424114,
176.483420797975));
#42941=CARTESIAN_POINT('Ctrl Pts',(-59.0071482133861,-73.4562553850365,
174.830711729305));
#42942=CARTESIAN_POINT('Ctrl Pts',(-58.0000494609201,-73.6579000689271,
173.516227941122));
#42943=CARTESIAN_POINT('Ctrl Pts',(-56.9929507084542,-73.8595447528177,
172.201744152939));
#42944=CARTESIAN_POINT('Ctrl Pts',(-55.359491909043,-74.1279636023579,171.99549242084));
#42945=CARTESIAN_POINT('Ctrl Pts',(-53.7260331096318,-74.3963824518981,
171.789240688742));
#42946=CARTESIAN_POINT('Ctrl Pts',(-52.4288938568657,-74.6289473908507,
172.812040480128));
#42947=CARTESIAN_POINT('Ctrl Pts',(-51.1317546040997,-74.8615123298032,
173.834840271514));
#42948=CARTESIAN_POINT('Ctrl Pts',(-50.9366030624358,-74.9765980164889,
175.487549340184));
#42949=CARTESIAN_POINT('Ctrl Pts',(-50.7414515207719,-75.0916837031745,
177.140258408853));
#42950=CARTESIAN_POINT('Ctrl Pts',(-51.7684263990719,-75.0764825485946,
178.454742197037));
#42951=CARTESIAN_POINT('Ctrl Pts',(-52.7954012773719,-75.0612813940147,
179.76922598522));
#42952=CARTESIAN_POINT('Ctrl Pts',(-54.4487362026171,-74.9793060737851,
179.975477717318));
#42953=CARTESIAN_POINT('Ctrl Pts',(-56.1020711278624,-74.8973307535556,
180.181729449417));
#42954=CARTESIAN_POINT('Ctrl Pts',(-57.4190865064624,-74.8512093439138,
179.158929658031));
#42955=CARTESIAN_POINT('Ctrl Pts',(-58.7361018850625,-74.805087934272,178.136129866644));
#42956=CARTESIAN_POINT('Ctrl Pts',(-58.9511295525604,-74.876445776897,176.483420797975));
#42957=CARTESIAN_POINT('Ctrl Pts',(-59.1661572200583,-74.9478036195221,
174.830711729305));
#42958=CARTESIAN_POINT('Ctrl Pts',(-58.1590584675924,-75.1494483034127,
173.516227941122));
#42959=CARTESIAN_POINT('Ctrl Pts',(-57.1519597151264,-75.3510929873033,
172.201744152939));
#42960=CARTESIAN_POINT('Ctrl Pts',(-55.5185009157152,-75.6195118368435,
171.99549242084));
#42961=CARTESIAN_POINT('Ctrl Pts',(-53.885042116304,-75.8879306863838,171.789240688742));
#42962=CARTESIAN_POINT('Ctrl Pts',(-52.587902863538,-76.1204956253363,172.812040480128));
#42963=CARTESIAN_POINT('Ctrl Pts',(-51.290763610772,-76.3530605642888,173.834840271514));
#42964=CARTESIAN_POINT('Ctrl Pts',(-51.0956120691081,-76.4681462509745,
175.487549340184));
#42965=CARTESIAN_POINT('Ctrl Pts',(-50.9004605274442,-76.5832319376601,
177.140258408853));
#42966=CARTESIAN_POINT('Ctrl Pts',(-51.9274354057441,-76.5680307830801,
178.454742197037));
#42967=CARTESIAN_POINT('Ctrl Pts',(-52.9544102840441,-76.5528296285002,
179.76922598522));
#42968=CARTESIAN_POINT('Ctrl Pts',(-54.6077452092894,-76.4708543082707,
179.975477717318));
#42969=CARTESIAN_POINT('Ctrl Pts',(-56.2610801345346,-76.3888789880412,
180.181729449417));
#42970=CARTESIAN_POINT('Ctrl Pts',(-57.5780955131346,-76.3427575783994,
179.158929658031));
#42971=CARTESIAN_POINT('Ctrl Pts',(-58.8951108917347,-76.2966361687575,
178.136129866644));
#42972=CARTESIAN_POINT('Ctrl Pts',(-59.1101385592326,-76.3679940113826,
176.483420797975));
#42973=CARTESIAN_POINT('Ctrl Pts',(-59.3251662267305,-76.4393518540077,
174.830711729305));
#42974=CARTESIAN_POINT('Ctrl Pts',(-58.3180674742646,-76.6409965378983,
173.516227941122));
#42975=CARTESIAN_POINT('Ctrl Pts',(-57.3109687217987,-76.8426412217889,
172.201744152939));
#42976=CARTESIAN_POINT('Ctrl Pts',(-55.6775099223874,-77.1110600713291,
171.99549242084));
#42977=CARTESIAN_POINT('Ctrl Pts',(-54.0440511229762,-77.3794789208693,
171.789240688742));
#42978=CARTESIAN_POINT('Ctrl Pts',(-52.7469118702102,-77.6120438598219,
172.812040480128));
#42979=CARTESIAN_POINT('Ctrl Pts',(-51.4497726174442,-77.8446087987744,
173.834840271514));
#42980=CARTESIAN_POINT('Ctrl Pts',(-51.2546210757803,-77.95969448546,175.487549340184));
#42981=CARTESIAN_POINT('Ctrl Pts',(-51.0594695341164,-78.0747801721457,
177.140258408853));
#42982=CARTESIAN_POINT('Ctrl Pts',(-52.0864444124164,-78.0595790175658,
178.454742197037));
#42983=CARTESIAN_POINT('Ctrl Pts',(-53.1134192907163,-78.0443778629858,
179.76922598522));
#42984=CARTESIAN_POINT('Ctrl Pts',(-54.7667542159616,-77.9624025427563,
179.975477717318));
#42985=CARTESIAN_POINT('Ctrl Pts',(-56.4200891412068,-77.8804272225268,
180.181729449417));
#42986=CARTESIAN_POINT('Ctrl Pts',(-57.7371045198069,-77.834305812885,179.158929658031));
#42987=CARTESIAN_POINT('Ctrl Pts',(-59.0541198984069,-77.7881844032432,
178.136129866644));
#42988=CARTESIAN_POINT('Ctrl Pts',(-59.2691475659048,-77.8595422458682,
176.483420797975));
#42989=CARTESIAN_POINT('Ctrl Pts',(-59.4841752334028,-77.9309000884933,
174.830711729305));
#42990=CARTESIAN_POINT('Ctrl Pts',(-58.4770764809368,-78.1325447723839,
173.516227941122));
#42991=CARTESIAN_POINT('Ctrl Pts',(-57.4699777284709,-78.3341894562745,
172.201744152939));
#42992=CARTESIAN_POINT('Ctrl Pts',(-55.8365189290597,-78.6026083058147,
171.99549242084));
#42993=CARTESIAN_POINT('Ctrl Pts',(-54.2030601296484,-78.871027155355,171.789240688742));
#42994=CARTESIAN_POINT('Ctrl Pts',(-52.9059208768824,-79.1035920943075,
172.812040480128));
#42995=CARTESIAN_POINT('Ctrl Pts',(-51.6087816241164,-79.33615703326,173.834840271514));
#42996=CARTESIAN_POINT('Ctrl Pts',(-51.4136300824525,-79.4512427199456,
175.487549340184));
#42997=CARTESIAN_POINT('Ctrl Pts',(-51.2184785407886,-79.5663284066313,
177.140258408853));
#42998=CARTESIAN_POINT('Ctrl Pts',(-52.2454534190886,-79.5511272520514,
178.454742197037));
#42999=CARTESIAN_POINT('Ctrl Pts',(-53.2724282973886,-79.5359260974714,
179.76922598522));
#43000=CARTESIAN_POINT('Ctrl Pts',(-54.9257632226338,-79.4539507772419,
179.975477717318));
#43001=CARTESIAN_POINT('Ctrl Pts',(-56.5790981478791,-79.3719754570124,
180.181729449417));
#43002=CARTESIAN_POINT('Ctrl Pts',(-57.8961135264791,-79.3258540473706,
179.158929658031));
#43003=CARTESIAN_POINT('Ctrl Pts',(-59.2131289050791,-79.2797326377288,
178.136129866644));
#43004=CARTESIAN_POINT('Ctrl Pts',(-59.4281565725771,-79.3510904803538,
176.483420797975));
#43005=CARTESIAN_POINT('Ctrl Pts',(-59.643184240075,-79.4224483229789,174.830711729305));
#43006=CARTESIAN_POINT('Ctrl Pts',(-58.6360854876091,-79.6240930068695,
173.516227941122));
#43007=CARTESIAN_POINT('Ctrl Pts',(-57.6289867351431,-79.8257376907601,
172.201744152939));
#43008=CARTESIAN_POINT('Ctrl Pts',(-55.9955279357319,-80.0941565403003,
171.99549242084));
#43009=CARTESIAN_POINT('Ctrl Pts',(-54.3620691363207,-80.3625753898405,
171.789240688742));
#43010=CARTESIAN_POINT('Ctrl Pts',(-53.0649298835546,-80.5951403287931,
172.812040480128));
#43011=CARTESIAN_POINT('Ctrl Pts',(-51.7677906307886,-80.8277052677456,
173.834840271514));
#43012=CARTESIAN_POINT('Ctrl Pts',(-51.5726390891247,-80.9427909544312,
175.487549340184));
#43013=CARTESIAN_POINT('Ctrl Pts',(-51.3774875474608,-81.0578766411169,
177.140258408853));
#43014=CARTESIAN_POINT('Ctrl Pts',(-52.4044624257608,-81.042675486537,178.454742197037));
#43015=CARTESIAN_POINT('Ctrl Pts',(-53.4314373040608,-81.027474331957,179.76922598522));
#43016=CARTESIAN_POINT('Ctrl Pts',(-55.084772229306,-80.9454990117275,179.975477717318));
#43017=CARTESIAN_POINT('Ctrl Pts',(-56.7381071545513,-80.863523691498,180.181729449417));
#43018=CARTESIAN_POINT('Ctrl Pts',(-58.0551225331513,-80.8174022818562,
179.158929658031));
#43019=CARTESIAN_POINT('Ctrl Pts',(-59.3721379117514,-80.7712808722144,
178.136129866644));
#43020=CARTESIAN_POINT('Ctrl Pts',(-59.5871655792493,-80.8426387148394,
176.483420797975));
#43021=CARTESIAN_POINT('Ctrl Pts',(-59.8021932467472,-80.9139965574645,
174.830711729305));
#43022=CARTESIAN_POINT('Ctrl Pts',(-58.7950944942813,-81.1156412413551,
173.516227941122));
#43023=CARTESIAN_POINT('Ctrl Pts',(-57.7879957418153,-81.3172859252457,
172.201744152939));
#43024=CARTESIAN_POINT('Ctrl Pts',(-56.1545369424041,-81.5857047747859,
171.99549242084));
#43025=CARTESIAN_POINT('Ctrl Pts',(-54.5210781429929,-81.8541236243262,
171.789240688742));
#43026=CARTESIAN_POINT('Ctrl Pts',(-53.2239388902269,-82.0866885632787,
172.812040480128));
#43027=CARTESIAN_POINT('Ctrl Pts',(-51.9267996374609,-82.3192535022312,
173.834840271514));
#43028=CARTESIAN_POINT('Ctrl Pts',(-51.731648095797,-82.4343391889168,175.487549340184));
#43029=CARTESIAN_POINT('Ctrl Pts',(-51.5364965541331,-82.5494248756025,
177.140258408853));
#43030=CARTESIAN_POINT('Ctrl Pts',(-52.563471432433,-82.5342237210226,178.454742197037));
#43031=CARTESIAN_POINT('Ctrl Pts',(-53.590446310733,-82.5190225664426,179.76922598522));
#43032=CARTESIAN_POINT('Ctrl Pts',(-55.2437812359783,-82.4370472462131,
179.975477717318));
#43033=CARTESIAN_POINT('Ctrl Pts',(-56.8971161612235,-82.3550719259836,
180.181729449417));
#43034=CARTESIAN_POINT('Ctrl Pts',(-58.2141315398236,-82.3089505163418,
179.158929658031));
#43035=CARTESIAN_POINT('Ctrl Pts',(-59.5311469184236,-82.2628291066999,
178.136129866644));
#43036=CARTESIAN_POINT('Ctrl Pts',(-59.7461745859215,-82.334186949325,176.483420797975));
#43037=CARTESIAN_POINT('Ctrl Pts',(-59.9612022534195,-82.4055447919501,
174.830711729305));
#43038=CARTESIAN_POINT('Ctrl Pts',(-58.9541035009535,-82.6071894758407,
173.516227941122));
#43039=CARTESIAN_POINT('Ctrl Pts',(-57.9470047484876,-82.8088341597313,
172.201744152939));
#43040=CARTESIAN_POINT('Ctrl Pts',(-56.3135459490763,-83.0772530092715,
171.99549242084));
#43041=CARTESIAN_POINT('Ctrl Pts',(-54.6800871496651,-83.3456718588118,
171.789240688742));
#43042=CARTESIAN_POINT('Ctrl Pts',(-53.3829478968991,-83.5782367977643,
172.812040480128));
#43043=CARTESIAN_POINT('Ctrl Pts',(-52.0858086441331,-83.8108017367168,
173.834840271514));
#43044=CARTESIAN_POINT('Ctrl Pts',(-51.8906571024692,-83.9258874234024,
175.487549340184));
#43045=CARTESIAN_POINT('Ctrl Pts',(-51.6955055608053,-84.0409731100881,
177.140258408853));
#43046=CARTESIAN_POINT('Ctrl Pts',(-52.7224804391053,-84.0257719555082,
178.454742197037));
#43047=CARTESIAN_POINT('Ctrl Pts',(-53.7494553174052,-84.0105708009282,
179.76922598522));
#43048=CARTESIAN_POINT('Ctrl Pts',(-55.4027902426505,-83.9285954806987,
179.975477717318));
#43049=CARTESIAN_POINT('Ctrl Pts',(-57.0561251678958,-83.8466201604692,
180.181729449417));
#43050=CARTESIAN_POINT('Ctrl Pts',(-58.3731405464958,-83.8004987508274,
179.158929658031));
#43051=CARTESIAN_POINT('Ctrl Pts',(-59.6901559250958,-83.7543773411855,
178.136129866644));
#43052=CARTESIAN_POINT('Ctrl Pts',(-59.9051835925938,-83.8257351838106,
176.483420797975));
#43053=CARTESIAN_POINT('Ctrl Pts',(-60.1202112600917,-83.8970930264357,
174.830711729305));
#43054=CARTESIAN_POINT('Ctrl Pts',(-59.1131125076257,-84.0987377103263,
173.516227941122));
#43055=CARTESIAN_POINT('Ctrl Pts',(-58.1060137551598,-84.3003823942169,
172.201744152939));
#43056=CARTESIAN_POINT('Ctrl Pts',(-56.4725549557486,-84.5688012437571,
171.99549242084));
#43057=CARTESIAN_POINT('Ctrl Pts',(-54.8390961563373,-84.8372200932974,
171.789240688742));
#43058=CARTESIAN_POINT('Ctrl Pts',(-53.5419569035713,-85.0697850322499,
172.812040480128));
#43059=CARTESIAN_POINT('Ctrl Pts',(-52.2448176508053,-85.3023499712024,
173.834840271514));
#43060=CARTESIAN_POINT('Ctrl Pts',(-52.0496661091414,-85.417435657888,175.487549340184));
#43061=CARTESIAN_POINT('Ctrl Pts',(-51.8545145674775,-85.5325213445737,
177.140258408853));
#43062=CARTESIAN_POINT('Ctrl Pts',(-52.8814894457775,-85.5173201899938,
178.454742197037));
#43063=CARTESIAN_POINT('Ctrl Pts',(-53.9084643240775,-85.5021190354138,
179.76922598522));
#43064=CARTESIAN_POINT('Ctrl Pts',(-55.5617992493227,-85.4201437151843,
179.975477717318));
#43065=CARTESIAN_POINT('Ctrl Pts',(-57.215134174568,-85.3381683949548,180.181729449417));
#43066=CARTESIAN_POINT('Ctrl Pts',(-58.532149553168,-85.292046985313,179.158929658031));
#43067=CARTESIAN_POINT('Ctrl Pts',(-59.849164931768,-85.2459255756712,178.136129866644));
#43068=CARTESIAN_POINT('Ctrl Pts',(-60.064192599266,-85.3172834182962,176.483420797975));
#43069=CARTESIAN_POINT('Ctrl Pts',(-60.2792202667639,-85.3886412609213,
174.830711729305));
#43070=CARTESIAN_POINT('Ctrl Pts',(-59.272121514298,-85.5902859448119,173.516227941122));
#43071=CARTESIAN_POINT('Ctrl Pts',(-58.265022761832,-85.7919306287025,172.201744152939));
#43072=CARTESIAN_POINT('Ctrl Pts',(-56.6315639624208,-86.0603494782428,
171.99549242084));
#43073=CARTESIAN_POINT('Ctrl Pts',(-54.9981051630096,-86.328768327783,171.789240688742));
#43074=CARTESIAN_POINT('Ctrl Pts',(-53.7009659102436,-86.5613332667355,
172.812040480128));
#43075=CARTESIAN_POINT('Ctrl Pts',(-52.4038266574776,-86.793898205688,173.834840271514));
#43076=CARTESIAN_POINT('Ctrl Pts',(-52.2086751158136,-86.9089838923736,
175.487549340184));
#43077=CARTESIAN_POINT('Ctrl Pts',(-52.0135235741498,-87.0240695790593,
177.140258408853));
#43078=CARTESIAN_POINT('Ctrl Pts',(-53.0404984524497,-87.0088684244793,
178.454742197037));
#43079=CARTESIAN_POINT('Ctrl Pts',(-54.0674733307497,-86.9936672698994,
179.76922598522));
#43080=CARTESIAN_POINT('Ctrl Pts',(-55.720808255995,-86.9116919496699,179.975477717318));
#43081=CARTESIAN_POINT('Ctrl Pts',(-57.3741431812402,-86.8297166294404,
180.181729449417));
#43082=CARTESIAN_POINT('Ctrl Pts',(-58.6911585598402,-86.7835952197986,
179.158929658031));
#43083=CARTESIAN_POINT('Ctrl Pts',(-60.0081739384403,-86.7374738101568,
178.136129866644));
#43084=CARTESIAN_POINT('Ctrl Pts',(-60.2232016059382,-86.8088316527818,
176.483420797975));
#43085=CARTESIAN_POINT('Ctrl Pts',(-60.4382292734361,-86.8801894954069,
174.830711729305));
#43086=CARTESIAN_POINT('Ctrl Pts',(-59.4311305209702,-87.0818341792975,
173.516227941122));
#43087=CARTESIAN_POINT('Ctrl Pts',(-58.4240317685042,-87.2834788631881,
172.201744152939));
#43088=CARTESIAN_POINT('Ctrl Pts',(-56.790572969093,-87.5518977127283,171.99549242084));
#43089=CARTESIAN_POINT('Ctrl Pts',(-55.1571141696818,-87.8203165622686,
171.789240688742));
#43090=CARTESIAN_POINT('Ctrl Pts',(-53.8599749169158,-88.0528815012211,
172.812040480128));
#43091=CARTESIAN_POINT('Ctrl Pts',(-52.5628356641498,-88.2854464401736,
173.834840271514));
#43092=CARTESIAN_POINT('Ctrl Pts',(-52.3676841224859,-88.4005321268593,
175.487549340184));
#43093=CARTESIAN_POINT('Ctrl Pts',(-52.172532580822,-88.5156178135449,177.140258408853));
#43094=CARTESIAN_POINT('Ctrl Pts',(-53.199507459122,-88.500416658965,178.454742197037));
#43095=CARTESIAN_POINT('Ctrl Pts',(-54.2264823374219,-88.4852155043851,
179.76922598522));
#43096=CARTESIAN_POINT('Ctrl Pts',(-55.8798172626672,-88.4032401841555,
179.975477717318));
#43097=CARTESIAN_POINT('Ctrl Pts',(-57.5331521879124,-88.321264863926,180.181729449417));
#43098=CARTESIAN_POINT('Ctrl Pts',(-58.8501675665125,-88.2751434542842,
179.158929658031));
#43099=CARTESIAN_POINT('Ctrl Pts',(-60.1671829451125,-88.2290220446423,
178.136129866644));
#43100=CARTESIAN_POINT('Ctrl Pts',(-60.3822106126104,-88.3003798872674,
176.483420797975));
#43101=CARTESIAN_POINT('Ctrl Pts',(-60.5972382801084,-88.3717377298925,
174.830711729305));
#43102=CARTESIAN_POINT('Ctrl Pts',(-59.5901395276424,-88.5733824137831,
173.516227941122));
#43103=CARTESIAN_POINT('Ctrl Pts',(-58.5830407751765,-88.7750270976737,
172.201744152939));
#43104=CARTESIAN_POINT('Ctrl Pts',(-56.9495819757652,-89.0434459472139,
171.99549242084));
#43105=CARTESIAN_POINT('Ctrl Pts',(-55.316123176354,-89.3118647967542,171.789240688742));
#43106=CARTESIAN_POINT('Ctrl Pts',(-54.018983923588,-89.5444297357067,172.812040480128));
#43107=CARTESIAN_POINT('Ctrl Pts',(-52.721844670822,-89.7769946746592,173.834840271514));
#43108=CARTESIAN_POINT('Ctrl Pts',(-52.5266931291581,-89.8920803613448,
175.487549340184));
#43109=CARTESIAN_POINT('Ctrl Pts',(-52.3315415874942,-90.0071660480305,
177.140258408853));
#43110=CARTESIAN_POINT('Ctrl Pts',(-53.3585164657942,-89.9919648934506,
178.454742197037));
#43111=CARTESIAN_POINT('Ctrl Pts',(-54.3854913440941,-89.9767637388707,
179.76922598522));
#43112=CARTESIAN_POINT('Ctrl Pts',(-56.0388262693394,-89.8947884186411,
179.975477717318));
#43113=CARTESIAN_POINT('Ctrl Pts',(-57.6921611945847,-89.8128130984116,
180.181729449417));
#43114=CARTESIAN_POINT('Ctrl Pts',(-59.0091765731847,-89.7666916887698,
179.158929658031));
#43115=CARTESIAN_POINT('Ctrl Pts',(-60.3261919517847,-89.720570279128,178.136129866644));
#43116=CARTESIAN_POINT('Ctrl Pts',(-60.5412196192827,-89.791928121753,176.483420797975));
#43117=CARTESIAN_POINT('Ctrl Pts',(-60.7562472867806,-89.8632859643781,
174.830711729305));
#43118=CARTESIAN_POINT('Ctrl Pts',(-59.7491485343146,-90.0649306482687,
173.516227941122));
#43119=CARTESIAN_POINT('Ctrl Pts',(-58.7420497818487,-90.2665753321593,
172.201744152939));
#43120=CARTESIAN_POINT('Ctrl Pts',(-57.1085909824375,-90.5349941816995,
171.99549242084));
#43121=CARTESIAN_POINT('Ctrl Pts',(-55.4751321830263,-90.8034130312398,
171.789240688742));
#43122=CARTESIAN_POINT('Ctrl Pts',(-54.1779929302602,-91.0359779701923,
172.812040480128));
#43123=CARTESIAN_POINT('Ctrl Pts',(-52.8808536774942,-91.2685429091448,
173.834840271514));
#43124=CARTESIAN_POINT('Ctrl Pts',(-52.6857021358303,-91.3836285958304,
175.487549340184));
#43125=CARTESIAN_POINT('Ctrl Pts',(-52.4905505941664,-91.4987142825161,
177.140258408853));
#43126=CARTESIAN_POINT('Ctrl Pts',(-53.5175254724664,-91.4835131279361,
178.454742197037));
#43127=CARTESIAN_POINT('Ctrl Pts',(-54.5445003507664,-91.4683119733563,
179.76922598522));
#43128=CARTESIAN_POINT('Ctrl Pts',(-56.1978352760116,-91.3863366531267,
179.975477717318));
#43129=CARTESIAN_POINT('Ctrl Pts',(-57.8511702012569,-91.3043613328972,
180.181729449417));
#43130=CARTESIAN_POINT('Ctrl Pts',(-59.1681855798569,-91.2582399232554,
179.158929658031));
#43131=CARTESIAN_POINT('Ctrl Pts',(-60.485200958457,-91.2121185136135,178.136129866644));
#43132=CARTESIAN_POINT('Ctrl Pts',(-60.7002286259549,-91.2834763562386,
176.483420797975));
#43133=CARTESIAN_POINT('Ctrl Pts',(-60.9152562934528,-91.3548341988637,
174.830711729305));
#43134=CARTESIAN_POINT('Ctrl Pts',(-59.9081575409869,-91.5564788827543,
173.516227941122));
#43135=CARTESIAN_POINT('Ctrl Pts',(-58.9010587885209,-91.7581235666449,
172.201744152939));
#43136=CARTESIAN_POINT('Ctrl Pts',(-57.2675999891097,-92.0265424161851,
171.99549242084));
#43137=CARTESIAN_POINT('Ctrl Pts',(-55.6341411896985,-92.2949612657254,
171.789240688742));
#43138=CARTESIAN_POINT('Ctrl Pts',(-54.3370019369325,-92.5275262046779,
172.812040480128));
#43139=CARTESIAN_POINT('Ctrl Pts',(-53.0398626841665,-92.7600911436304,
173.834840271514));
#43140=CARTESIAN_POINT('Ctrl Pts',(-52.8447111425026,-92.875176830316,175.487549340184));
#43141=CARTESIAN_POINT('Ctrl Pts',(-52.6495596008387,-92.9902625170017,
177.140258408853));
#43142=CARTESIAN_POINT('Ctrl Pts',(-53.6765344791386,-92.9750613624218,
178.454742197037));
#43143=CARTESIAN_POINT('Ctrl Pts',(-54.7035093574386,-92.9598602078419,
179.76922598522));
#43144=CARTESIAN_POINT('Ctrl Pts',(-56.3568442826839,-92.8778848876123,
179.975477717318));
#43145=CARTESIAN_POINT('Ctrl Pts',(-58.0101792079291,-92.7959095673828,
180.181729449417));
#43146=CARTESIAN_POINT('Ctrl Pts',(-59.3271945865291,-92.749788157741,179.158929658031));
#43147=CARTESIAN_POINT('Ctrl Pts',(-60.6442099651292,-92.7036667480992,
178.136129866644));
#43148=CARTESIAN_POINT('Ctrl Pts',(-60.8592376326271,-92.7750245907242,
176.483420797975));
#43149=CARTESIAN_POINT('Ctrl Pts',(-61.074265300125,-92.8463824333493,174.830711729305));
#43150=CARTESIAN_POINT('Ctrl Pts',(-60.0671665476591,-93.0480271172399,
173.516227941122));
#43151=CARTESIAN_POINT('Ctrl Pts',(-59.0600677951932,-93.2496718011305,
172.201744152939));
#43152=CARTESIAN_POINT('Ctrl Pts',(-57.4266089957819,-93.5180906506707,
171.99549242084));
#43153=CARTESIAN_POINT('Ctrl Pts',(-55.7931501963707,-93.786509500211,171.789240688742));
#43154=CARTESIAN_POINT('Ctrl Pts',(-54.4960109436047,-94.0190744391634,
172.812040480128));
#43155=CARTESIAN_POINT('Ctrl Pts',(-53.1988716908387,-94.251639378116,173.834840271514));
#43156=CARTESIAN_POINT('Ctrl Pts',(-53.0037201491748,-94.3667250648016,
175.487549340184));
#43157=CARTESIAN_POINT('Ctrl Pts',(-52.8085686075109,-94.4818107514873,
177.140258408853));
#43158=CARTESIAN_POINT('Ctrl Pts',(-53.8355434858109,-94.4666095969074,
178.454742197037));
#43159=CARTESIAN_POINT('Ctrl Pts',(-54.8625183641108,-94.4514084423274,
179.76922598522));
#43160=CARTESIAN_POINT('Ctrl Pts',(-56.5158532893561,-94.3694331220979,
179.975477717318));
#43161=CARTESIAN_POINT('Ctrl Pts',(-58.1691882146013,-94.2874578018684,
180.181729449417));
#43162=CARTESIAN_POINT('Ctrl Pts',(-59.4862035932014,-94.2413363922266,
179.158929658031));
#43163=CARTESIAN_POINT('Ctrl Pts',(-60.8032189718014,-94.1952149825848,
178.136129866644));
#43164=CARTESIAN_POINT('Ctrl Pts',(-61.0182466392993,-94.2665728252098,
176.483420797975));
#43165=CARTESIAN_POINT('Ctrl Pts',(-61.2332743067973,-94.3379306678349,
174.830711729305));
#43166=CARTESIAN_POINT('Ctrl Pts',(-60.2261755543313,-94.5395753517255,
173.516227941122));
#43167=CARTESIAN_POINT('Ctrl Pts',(-59.2190768018654,-94.7412200356161,
172.201744152939));
#43168=CARTESIAN_POINT('Ctrl Pts',(-57.5856180024542,-95.0096388851563,
171.99549242084));
#43169=CARTESIAN_POINT('Ctrl Pts',(-55.9521592030429,-95.2780577346965,
171.789240688742));
#43170=CARTESIAN_POINT('Ctrl Pts',(-54.6550199502769,-95.5106226736491,
172.812040480128));
#43171=CARTESIAN_POINT('Ctrl Pts',(-53.3578806975109,-95.7431876126016,
173.834840271514));
#43172=CARTESIAN_POINT('Ctrl Pts',(-53.162729155847,-95.8582732992872,175.487549340184));
#43173=CARTESIAN_POINT('Ctrl Pts',(-52.9675776141831,-95.9733589859729,
177.140258408853));
#43174=CARTESIAN_POINT('Ctrl Pts',(-53.9945524924831,-95.958157831393,178.454742197037));
#43175=CARTESIAN_POINT('Ctrl Pts',(-55.0215273707831,-95.9429566768131,
179.76922598522));
#43176=CARTESIAN_POINT('Ctrl Pts',(-56.6748622960283,-95.8609813565835,
179.975477717318));
#43177=CARTESIAN_POINT('Ctrl Pts',(-58.3281972212736,-95.779006036354,180.181729449417));
#43178=CARTESIAN_POINT('Ctrl Pts',(-59.6452125998736,-95.7328846267122,
179.158929658031));
#43179=CARTESIAN_POINT('Ctrl Pts',(-60.9622279784736,-95.6867632170703,
178.136129866644));
#43180=CARTESIAN_POINT('Ctrl Pts',(-61.1772556459716,-95.7581210596954,
176.483420797975));
#43181=CARTESIAN_POINT('Ctrl Pts',(-61.3922833134695,-95.8294789023205,
174.830711729305));
#43182=CARTESIAN_POINT('Ctrl Pts',(-60.3851845610036,-96.0311235862111,
173.516227941122));
#43183=CARTESIAN_POINT('Ctrl Pts',(-59.3780858085376,-96.2327682701017,
172.201744152939));
#43184=CARTESIAN_POINT('Ctrl Pts',(-57.7446270091264,-96.5011871196419,
171.99549242084));
#43185=CARTESIAN_POINT('Ctrl Pts',(-56.1111682097152,-96.7696059691822,
171.789240688742));
#43186=CARTESIAN_POINT('Ctrl Pts',(-54.8140289569491,-97.0021709081347,
172.812040480128));
#43187=CARTESIAN_POINT('Ctrl Pts',(-53.5168897041831,-97.2347358470872,
173.834840271514));
#43188=CARTESIAN_POINT('Ctrl Pts',(-53.3217381625192,-97.3498215337729,
175.487549340184));
#43189=CARTESIAN_POINT('Ctrl Pts',(-53.1265866208553,-97.4649072204585,
177.140258408853));
#43190=CARTESIAN_POINT('Ctrl Pts',(-54.1535614991553,-97.4497060658786,
178.454742197037));
#43191=CARTESIAN_POINT('Ctrl Pts',(-55.1805363774553,-97.4345049112986,
179.76922598522));
#43192=CARTESIAN_POINT('Ctrl Pts',(-56.8338713027005,-97.3525295910691,
179.975477717318));
#43193=CARTESIAN_POINT('Ctrl Pts',(-58.4872062279458,-97.2705542708396,
180.181729449417));
#43194=CARTESIAN_POINT('Ctrl Pts',(-59.8042216065458,-97.2244328611978,
179.158929658031));
#43195=CARTESIAN_POINT('Ctrl Pts',(-61.1212369851459,-97.178311451556,178.136129866644));
#43196=CARTESIAN_POINT('Ctrl Pts',(-61.3362646526438,-97.249669294181,176.483420797975));
#43197=CARTESIAN_POINT('Ctrl Pts',(-61.5512923201417,-97.3210271368061,
174.830711729305));
#43198=CARTESIAN_POINT('Ctrl Pts',(-60.5441935676758,-97.5226718206967,
173.516227941122));
#43199=CARTESIAN_POINT('Ctrl Pts',(-59.5370948152098,-97.7243165045873,
172.201744152939));
#43200=CARTESIAN_POINT('Ctrl Pts',(-57.9036360157986,-97.9927353541275,
171.99549242084));
#43201=CARTESIAN_POINT('Ctrl Pts',(-56.2701772163874,-98.2611542036678,
171.789240688742));
#43202=CARTESIAN_POINT('Ctrl Pts',(-54.9730379636214,-98.4937191426203,
172.812040480128));
#43203=CARTESIAN_POINT('Ctrl Pts',(-53.6758987108554,-98.7262840815728,
173.834840271514));
#43204=CARTESIAN_POINT('Ctrl Pts',(-53.4807471691915,-98.8413697682584,
175.487549340184));
#43205=CARTESIAN_POINT('Ctrl Pts',(-53.2855956275276,-98.9564554549441,
177.140258408853));
#43206=CARTESIAN_POINT('Ctrl Pts',(-54.3125705058275,-98.9412543003642,
178.454742197037));
#43207=CARTESIAN_POINT('Ctrl Pts',(-55.3395453841275,-98.9260531457843,
179.76922598522));
#43208=CARTESIAN_POINT('Ctrl Pts',(-56.9928803093728,-98.8440778255547,
179.975477717318));
#43209=CARTESIAN_POINT('Ctrl Pts',(-58.646215234618,-98.7621025053252,180.181729449417));
#43210=CARTESIAN_POINT('Ctrl Pts',(-59.9632306132181,-98.7159810956834,
179.158929658031));
#43211=CARTESIAN_POINT('Ctrl Pts',(-61.2802459918181,-98.6698596860415,
178.136129866644));
#43212=CARTESIAN_POINT('Ctrl Pts',(-61.495273659316,-98.7412175286666,176.483420797975));
#43213=CARTESIAN_POINT('Ctrl Pts',(-61.710301326814,-98.8125753712917,174.830711729305));
#43214=CARTESIAN_POINT('Ctrl Pts',(-60.703202574348,-99.0142200551823,173.516227941122));
#43215=CARTESIAN_POINT('Ctrl Pts',(-59.6961038218821,-99.2158647390729,
172.201744152939));
#43216=CARTESIAN_POINT('Ctrl Pts',(-58.0626450224708,-99.4842835886131,
171.99549242084));
#43217=CARTESIAN_POINT('Ctrl Pts',(-56.4291862230596,-99.7527024381534,
171.789240688742));
#43218=CARTESIAN_POINT('Ctrl Pts',(-55.1320469702936,-99.9852673771059,
172.812040480128));
#43219=CARTESIAN_POINT('Ctrl Pts',(-53.8349077175276,-100.217832316058,
173.834840271514));
#43220=CARTESIAN_POINT('Ctrl Pts',(-53.6397561758637,-100.332918002744,
175.487549340184));
#43221=CARTESIAN_POINT('Ctrl Pts',(-53.4446046341998,-100.44800368943,177.140258408853));
#43222=CARTESIAN_POINT('Ctrl Pts',(-54.4715795124998,-100.43280253485,178.454742197037));
#43223=CARTESIAN_POINT('Ctrl Pts',(-55.4985543907998,-100.41760138027,179.76922598522));
#43224=CARTESIAN_POINT('Ctrl Pts',(-57.151889316045,-100.33562606004,179.975477717318));
#43225=CARTESIAN_POINT('Ctrl Pts',(-58.8052242412903,-100.253650739811,
180.181729449417));
#43226=CARTESIAN_POINT('Ctrl Pts',(-60.1222396198903,-100.207529330169,
179.158929658031));
#43227=CARTESIAN_POINT('Ctrl Pts',(-61.4392549984903,-100.161407920527,
178.136129866644));
#43228=CARTESIAN_POINT('Ctrl Pts',(-61.6542826659882,-100.232765763152,
176.483420797975));
#43229=CARTESIAN_POINT('Ctrl Pts',(-61.8693103334862,-100.304123605777,
174.830711729305));
#43230=CARTESIAN_POINT('Ctrl Pts',(-60.8622115810202,-100.505768289668,
173.516227941122));
#43231=CARTESIAN_POINT('Ctrl Pts',(-59.8551128285543,-100.707412973559,
172.201744152939));
#43232=CARTESIAN_POINT('Ctrl Pts',(-58.2216540291431,-100.975831823099,
171.99549242084));
#43233=CARTESIAN_POINT('Ctrl Pts',(-56.5881952297318,-101.244250672639,
171.789240688742));
#43234=CARTESIAN_POINT('Ctrl Pts',(-55.2910559769658,-101.476815611591,
172.812040480128));
#43235=CARTESIAN_POINT('Ctrl Pts',(-53.9939167241998,-101.709380550544,
173.834840271514));
#43236=CARTESIAN_POINT('Ctrl Pts',(-53.7987651825359,-101.82446623723,175.487549340184));
#43237=CARTESIAN_POINT('Ctrl Pts',(-53.603613640872,-101.939551923915,177.140258408853));
#43238=CARTESIAN_POINT('Ctrl Pts',(-54.630588519172,-101.924350769335,178.454742197037));
#43239=CARTESIAN_POINT('Ctrl Pts',(-55.657563397472,-101.909149614755,179.76922598522));
#43240=CARTESIAN_POINT('Ctrl Pts',(-57.3108983227172,-101.827174294526,
179.975477717318));
#43241=CARTESIAN_POINT('Ctrl Pts',(-58.9642332479625,-101.745198974296,
180.181729449417));
#43242=CARTESIAN_POINT('Ctrl Pts',(-60.2812486265625,-101.699077564655,
179.158929658031));
#43243=CARTESIAN_POINT('Ctrl Pts',(-61.5982640051626,-101.652956155013,
178.136129866644));
#43244=CARTESIAN_POINT('Ctrl Pts',(-61.8132916726605,-101.724313997638,
176.483420797975));
#43245=CARTESIAN_POINT('Ctrl Pts',(-62.0283193401584,-101.795671840263,
174.830711729305));
#43246=CARTESIAN_POINT('Ctrl Pts',(-61.0212205876925,-101.997316524153,
173.516227941122));
#43247=CARTESIAN_POINT('Ctrl Pts',(-60.0141218352265,-102.198961208044,
172.201744152939));
#43248=CARTESIAN_POINT('Ctrl Pts',(-58.3806630358153,-102.467380057584,
171.99549242084));
#43249=CARTESIAN_POINT('Ctrl Pts',(-56.7472042364041,-102.735798907125,
171.789240688742));
#43250=CARTESIAN_POINT('Ctrl Pts',(-55.4500649836381,-102.968363846077,
172.812040480128));
#43251=CARTESIAN_POINT('Ctrl Pts',(-54.1529257308721,-103.20092878503,173.834840271514));
#43252=CARTESIAN_POINT('Ctrl Pts',(-53.9577741892082,-103.316014471715,
175.487549340184));
#43253=CARTESIAN_POINT('Ctrl Pts',(-53.7626226475442,-103.431100158401,
177.140258408853));
#43254=CARTESIAN_POINT('Ctrl Pts',(-54.7895975258442,-103.415899003821,
178.454742197037));
#43255=CARTESIAN_POINT('Ctrl Pts',(-55.8165724041442,-103.400697849241,
179.76922598522));
#43256=CARTESIAN_POINT('Ctrl Pts',(-57.4699073293895,-103.318722529012,
179.975477717318));
#43257=CARTESIAN_POINT('Ctrl Pts',(-59.1232422546347,-103.236747208782,
180.181729449417));
#43258=CARTESIAN_POINT('Ctrl Pts',(-60.4402576332347,-103.19062579914,179.158929658031));
#43259=CARTESIAN_POINT('Ctrl Pts',(-61.7572730118348,-103.144504389498,
178.136129866644));
#43260=CARTESIAN_POINT('Ctrl Pts',(-61.9723006793327,-103.215862232123,
176.483420797975));
#43261=CARTESIAN_POINT('Ctrl Pts',(-62.1873283468306,-103.287220074748,
174.830711729305));
#43262=CARTESIAN_POINT('Ctrl Pts',(-61.1802295943647,-103.488864758639,
173.516227941122));
#43263=CARTESIAN_POINT('Ctrl Pts',(-60.1731308418988,-103.69050944253,172.201744152939));
#43264=CARTESIAN_POINT('Ctrl Pts',(-58.5396720424875,-103.95892829207,171.99549242084));
#43265=CARTESIAN_POINT('Ctrl Pts',(-56.9062132430763,-104.22734714161,171.789240688742));
#43266=CARTESIAN_POINT('Ctrl Pts',(-55.6090739903103,-104.459912080563,
172.812040480128));
#43267=CARTESIAN_POINT('Ctrl Pts',(-54.3119347375443,-104.692477019515,
173.834840271514));
#43268=CARTESIAN_POINT('Ctrl Pts',(-54.1167831958804,-104.807562706201,
175.487549340184));
#43269=CARTESIAN_POINT('Ctrl Pts',(-53.9216316542165,-104.922648392887,
177.140258408853));
#43270=CARTESIAN_POINT('Ctrl Pts',(-54.9486065325165,-104.907447238307,
178.454742197037));
#43271=CARTESIAN_POINT('Ctrl Pts',(-55.9755814108164,-104.892246083727,
179.76922598522));
#43272=CARTESIAN_POINT('Ctrl Pts',(-57.6289163360617,-104.810270763497,
179.975477717318));
#43273=CARTESIAN_POINT('Ctrl Pts',(-59.2822512613069,-104.728295443268,
180.181729449417));
#43274=CARTESIAN_POINT('Ctrl Pts',(-60.599266639907,-104.682174033626,179.158929658031));
#43275=CARTESIAN_POINT('Ctrl Pts',(-61.916282018507,-104.636052623984,178.136129866644));
#43276=CARTESIAN_POINT('Ctrl Pts',(-62.1313096860049,-104.707410466609,
176.483420797975));
#43277=CARTESIAN_POINT('Ctrl Pts',(-62.3463373535029,-104.778768309234,
174.830711729305));
#43278=CARTESIAN_POINT('Ctrl Pts',(-61.3392386010369,-104.980412993125,
173.516227941122));
#43279=CARTESIAN_POINT('Ctrl Pts',(-60.332139848571,-105.182057677015,172.201744152939));
#43280=CARTESIAN_POINT('Ctrl Pts',(-58.6986810491597,-105.450476526556,
171.99549242084));
#43281=CARTESIAN_POINT('Ctrl Pts',(-57.0652222497485,-105.718895376096,
171.789240688742));
#43282=CARTESIAN_POINT('Ctrl Pts',(-55.7680829969825,-105.951460315048,
172.812040480128));
#43283=CARTESIAN_POINT('Ctrl Pts',(-54.4709437442165,-106.184025254001,
173.834840271514));
#43284=CARTESIAN_POINT('Ctrl Pts',(-54.2757922025526,-106.299110940686,
175.487549340184));
#43285=CARTESIAN_POINT('Ctrl Pts',(-54.0806406608887,-106.414196627372,
177.140258408853));
#43286=CARTESIAN_POINT('Ctrl Pts',(-55.1076155391887,-106.398995472792,
178.454742197037));
#43287=CARTESIAN_POINT('Ctrl Pts',(-56.1345904174887,-106.383794318212,
179.76922598522));
#43288=CARTESIAN_POINT('Ctrl Pts',(-57.7879253427339,-106.301818997983,
179.975477717318));
#43289=CARTESIAN_POINT('Ctrl Pts',(-59.4412602679792,-106.219843677753,
180.181729449417));
#43290=CARTESIAN_POINT('Ctrl Pts',(-60.7582756465792,-106.173722268111,
179.158929658031));
#43291=CARTESIAN_POINT('Ctrl Pts',(-62.0752910251792,-106.12760085847,178.136129866644));
#43292=CARTESIAN_POINT('Ctrl Pts',(-62.2903186926772,-106.198958701095,
176.483420797975));
#43293=CARTESIAN_POINT('Ctrl Pts',(-62.5053463601751,-106.27031654372,174.830711729305));
#43294=CARTESIAN_POINT('Ctrl Pts',(-61.4982476077091,-106.47196122761,173.516227941122));
#43295=CARTESIAN_POINT('Ctrl Pts',(-60.4911488552432,-106.673605911501,
172.201744152939));
#43296=CARTESIAN_POINT('Ctrl Pts',(-58.857690055832,-106.942024761041,171.99549242084));
#43297=CARTESIAN_POINT('Ctrl Pts',(-57.2242312564208,-107.210443610581,
171.789240688742));
#43298=CARTESIAN_POINT('Ctrl Pts',(-55.9270920036547,-107.443008549534,
172.812040480128));
#43299=CARTESIAN_POINT('Ctrl Pts',(-54.6299527508887,-107.675573488486,
173.834840271514));
#43300=CARTESIAN_POINT('Ctrl Pts',(-54.4348012092248,-107.790659175172,
175.487549340184));
#43301=CARTESIAN_POINT('Ctrl Pts',(-54.2396496675609,-107.905744861858,
177.140258408853));
#43302=CARTESIAN_POINT('Ctrl Pts',(-55.2666245458609,-107.890543707278,
178.454742197037));
#43303=CARTESIAN_POINT('Ctrl Pts',(-56.2935994241609,-107.875342552698,
179.76922598522));
#43304=CARTESIAN_POINT('Ctrl Pts',(-57.9469343494061,-107.793367232468,
179.975477717318));
#43305=CARTESIAN_POINT('Ctrl Pts',(-59.6002692746514,-107.711391912239,
180.181729449417));
#43306=CARTESIAN_POINT('Ctrl Pts',(-60.9172846532514,-107.665270502597,
179.158929658031));
#43307=CARTESIAN_POINT('Ctrl Pts',(-62.2343000318515,-107.619149092955,
178.136129866644));
#43308=CARTESIAN_POINT('Ctrl Pts',(-62.4493276993494,-107.69050693558,176.483420797975));
#43309=CARTESIAN_POINT('Ctrl Pts',(-62.6643553668473,-107.761864778205,
174.830711729305));
#43310=CARTESIAN_POINT('Ctrl Pts',(-61.6572566143814,-107.963509462096,
173.516227941122));
#43311=CARTESIAN_POINT('Ctrl Pts',(-60.6501578619154,-108.165154145987,
172.201744152939));
#43312=CARTESIAN_POINT('Ctrl Pts',(-59.0166990625042,-108.433572995527,
171.99549242084));
#43313=CARTESIAN_POINT('Ctrl Pts',(-57.383240263093,-108.701991845067,171.789240688742));
#43314=CARTESIAN_POINT('Ctrl Pts',(-56.086101010327,-108.934556784019,172.812040480128));
#43315=CARTESIAN_POINT('Ctrl Pts',(-54.788961757561,-109.167121722972,173.834840271514));
#43316=CARTESIAN_POINT('Ctrl Pts',(-54.5938102158971,-109.282207409658,
175.487549340184));
#43317=CARTESIAN_POINT('Ctrl Pts',(-54.3986586742332,-109.397293096343,
177.140258408853));
#43318=CARTESIAN_POINT('Ctrl Pts',(-55.4256335525331,-109.382091941763,
178.454742197037));
#43319=CARTESIAN_POINT('Ctrl Pts',(-56.4526084308331,-109.366890787183,
179.76922598522));
#43320=CARTESIAN_POINT('Ctrl Pts',(-58.1059433560784,-109.284915466954,
179.975477717318));
#43321=CARTESIAN_POINT('Ctrl Pts',(-59.7592782813236,-109.202940146724,
180.181729449417));
#43322=CARTESIAN_POINT('Ctrl Pts',(-61.0762936599236,-109.156818737083,
179.158929658031));
#43323=CARTESIAN_POINT('Ctrl Pts',(-62.3933090385237,-109.110697327441,
178.136129866644));
#43324=CARTESIAN_POINT('Ctrl Pts',(-62.6083367060216,-109.182055170066,
176.483420797975));
#43325=CARTESIAN_POINT('Ctrl Pts',(-62.8233643735195,-109.253413012691,
174.830711729305));
#43326=CARTESIAN_POINT('Ctrl Pts',(-61.8162656210536,-109.455057696581,
173.516227941122));
#43327=CARTESIAN_POINT('Ctrl Pts',(-60.8091668685877,-109.656702380472,
172.201744152939));
#43328=CARTESIAN_POINT('Ctrl Pts',(-59.1757080691764,-109.925121230012,
171.99549242084));
#43329=CARTESIAN_POINT('Ctrl Pts',(-57.5422492697652,-110.193540079553,
171.789240688742));
#43330=CARTESIAN_POINT('Ctrl Pts',(-56.2451100169992,-110.426105018505,
172.812040480128));
#43331=CARTESIAN_POINT('Ctrl Pts',(-54.9479707642332,-110.658669957458,
173.834840271514));
#43332=CARTESIAN_POINT('Ctrl Pts',(-54.7528192225693,-110.773755644143,
175.487549340184));
#43333=CARTESIAN_POINT('Ctrl Pts',(-54.5576676809054,-110.888841330829,
177.140258408853));
#43334=CARTESIAN_POINT('Ctrl Pts',(-55.5846425592054,-110.873640176249,
178.454742197037));
#43335=CARTESIAN_POINT('Ctrl Pts',(-56.6116174375053,-110.858439021669,
179.76922598522));
#43336=CARTESIAN_POINT('Ctrl Pts',(-58.2649523627506,-110.77646370144,179.975477717318));
#43337=CARTESIAN_POINT('Ctrl Pts',(-59.9182872879959,-110.69448838121,180.181729449417));
#43338=CARTESIAN_POINT('Ctrl Pts',(-61.2353026665959,-110.648366971568,
179.158929658031));
#43339=CARTESIAN_POINT('Ctrl Pts',(-62.5523180451959,-110.602245561926,
178.136129866644));
#43340=CARTESIAN_POINT('Ctrl Pts',(-62.7673457126938,-110.673603404551,
176.483420797975));
#43341=CARTESIAN_POINT('Ctrl Pts',(-62.9823733801918,-110.744961247176,
174.830711729305));
#43342=CARTESIAN_POINT('Ctrl Pts',(-61.9752746277258,-110.946605931067,
173.516227941122));
#43343=CARTESIAN_POINT('Ctrl Pts',(-60.9681758752599,-111.148250614958,
172.201744152939));
#43344=CARTESIAN_POINT('Ctrl Pts',(-59.3347170758487,-111.416669464498,
171.99549242084));
#43345=CARTESIAN_POINT('Ctrl Pts',(-57.7012582764374,-111.685088314038,
171.789240688742));
#43346=CARTESIAN_POINT('Ctrl Pts',(-56.4041190236714,-111.917653252991,
172.812040480128));
#43347=CARTESIAN_POINT('Ctrl Pts',(-55.1069797709054,-112.150218191943,
173.834840271514));
#43348=CARTESIAN_POINT('Ctrl Pts',(-54.9118282292415,-112.265303878629,
175.487549340184));
#43349=CARTESIAN_POINT('Ctrl Pts',(-54.7166766875776,-112.380389565314,
177.140258408853));
#43350=CARTESIAN_POINT('Ctrl Pts',(-55.7436515658776,-112.365188410735,
178.454742197037));
#43351=CARTESIAN_POINT('Ctrl Pts',(-56.7706264441776,-112.349987256155,
179.76922598522));
#43352=CARTESIAN_POINT('Ctrl Pts',(-58.4239613694228,-112.268011935925,
179.975477717318));
#43353=CARTESIAN_POINT('Ctrl Pts',(-60.0772962946681,-112.186036615696,
180.181729449417));
#43354=CARTESIAN_POINT('Ctrl Pts',(-61.3943116732681,-112.139915206054,
179.158929658031));
#43355=CARTESIAN_POINT('Ctrl Pts',(-62.7113270518682,-112.093793796412,
178.136129866644));
#43356=CARTESIAN_POINT('Ctrl Pts',(-62.9263547193661,-112.165151639037,
176.483420797975));
#43357=CARTESIAN_POINT('Ctrl Pts',(-63.141382386864,-112.236509481662,174.830711729305));
#43358=CARTESIAN_POINT('Ctrl Pts',(-62.134283634398,-112.438154165553,173.516227941122));
#43359=CARTESIAN_POINT('Ctrl Pts',(-61.1271848819321,-112.639798849443,
172.201744152939));
#43360=CARTESIAN_POINT('Ctrl Pts',(-59.4937260825209,-112.908217698984,
171.99549242084));
#43361=CARTESIAN_POINT('Ctrl Pts',(-57.8602672831097,-113.176636548524,
171.789240688742));
#43362=CARTESIAN_POINT('Ctrl Pts',(-56.5631280303436,-113.409201487476,
172.812040480128));
#43363=CARTESIAN_POINT('Ctrl Pts',(-55.2659887775776,-113.641766426429,
173.834840271514));
#43364=CARTESIAN_POINT('Ctrl Pts',(-55.0708372359137,-113.756852113114,
175.487549340184));
#43365=CARTESIAN_POINT('Ctrl Pts',(-54.8756856942498,-113.8719377998,177.140258408853));
#43366=CARTESIAN_POINT('Ctrl Pts',(-55.9026605725498,-113.85673664522,178.454742197037));
#43367=CARTESIAN_POINT('Ctrl Pts',(-56.9296354508498,-113.84153549064,179.76922598522));
#43368=CARTESIAN_POINT('Ctrl Pts',(-58.582970376095,-113.759560170411,179.975477717318));
#43369=CARTESIAN_POINT('Ctrl Pts',(-60.2363053013403,-113.677584850181,
180.181729449417));
#43370=CARTESIAN_POINT('Ctrl Pts',(-61.5533206799403,-113.631463440539,
179.158929658031));
#43371=CARTESIAN_POINT('Ctrl Pts',(-62.8703360585404,-113.585342030898,
178.136129866644));
#43372=CARTESIAN_POINT('Ctrl Pts',(-63.0853637260383,-113.656699873523,
176.483420797975));
#43373=CARTESIAN_POINT('Ctrl Pts',(-63.3003913935362,-113.728057716148,
174.830711729305));
#43374=CARTESIAN_POINT('Ctrl Pts',(-62.2932926410703,-113.929702400038,
173.516227941122));
#43375=CARTESIAN_POINT('Ctrl Pts',(-61.2861938886043,-114.131347083929,
172.201744152939));
#43376=CARTESIAN_POINT('Ctrl Pts',(-59.6527350891931,-114.399765933469,
171.99549242084));
#43377=CARTESIAN_POINT('Ctrl Pts',(-58.0192762897819,-114.668184783009,
171.789240688742));
#43378=CARTESIAN_POINT('Ctrl Pts',(-56.7221370370159,-114.900749721962,
172.812040480128));
#43379=CARTESIAN_POINT('Ctrl Pts',(-55.4249977842499,-115.133314660914,
173.834840271514));
#43380=CARTESIAN_POINT('Ctrl Pts',(-55.229846242586,-115.2484003476,175.487549340184));
#43381=CARTESIAN_POINT('Ctrl Pts',(-55.0346947009221,-115.363486034286,
177.140258408853));
#43382=CARTESIAN_POINT('Ctrl Pts',(-56.061669579222,-115.348284879706,178.454742197037));
#43383=CARTESIAN_POINT('Ctrl Pts',(-57.088644457522,-115.333083725126,179.76922598522));
#43384=CARTESIAN_POINT('Ctrl Pts',(-58.7419793827673,-115.251108404896,
179.975477717318));
#43385=CARTESIAN_POINT('Ctrl Pts',(-60.3953143080125,-115.169133084667,
180.181729449417));
#43386=CARTESIAN_POINT('Ctrl Pts',(-61.7123296866126,-115.123011675025,
179.158929658031));
#43387=CARTESIAN_POINT('Ctrl Pts',(-63.0293450652126,-115.076890265383,
178.136129866644));
#43388=CARTESIAN_POINT('Ctrl Pts',(-63.2443727327105,-115.148248108008,
176.483420797975));
#43389=CARTESIAN_POINT('Ctrl Pts',(-63.4594004002085,-115.219605950633,
174.830711729305));
#43390=CARTESIAN_POINT('Ctrl Pts',(-62.4523016477425,-115.421250634524,
173.516227941122));
#43391=CARTESIAN_POINT('Ctrl Pts',(-61.4452028952766,-115.622895318415,
172.201744152939));
#43392=CARTESIAN_POINT('Ctrl Pts',(-59.8117440958653,-115.891314167955,
171.99549242084));
#43393=CARTESIAN_POINT('Ctrl Pts',(-58.1782852964541,-116.159733017495,
171.789240688742));
#43394=CARTESIAN_POINT('Ctrl Pts',(-56.8811460436881,-116.392297956447,
172.812040480128));
#43395=CARTESIAN_POINT('Ctrl Pts',(-55.5840067909221,-116.6248628954,173.834840271514));
#43396=CARTESIAN_POINT('Ctrl Pts',(-55.3888552492582,-116.739948582086,
175.487549340184));
#43397=CARTESIAN_POINT('Ctrl Pts',(-55.1937037075943,-116.855034268771,
177.140258408853));
#43398=CARTESIAN_POINT('Ctrl Pts',(-56.2206785858943,-116.839833114191,
178.454742197037));
#43399=CARTESIAN_POINT('Ctrl Pts',(-57.2476534641943,-116.824631959611,
179.76922598522));
#43400=CARTESIAN_POINT('Ctrl Pts',(-58.9009883894395,-116.742656639382,
179.975477717318));
#43401=CARTESIAN_POINT('Ctrl Pts',(-60.5543233146848,-116.660681319152,
180.181729449417));
#43402=CARTESIAN_POINT('Ctrl Pts',(-61.8713386932848,-116.614559909511,
179.158929658031));
#43403=CARTESIAN_POINT('Ctrl Pts',(-63.1883540718848,-116.568438499869,
178.136129866644));
#43404=CARTESIAN_POINT('Ctrl Pts',(-63.4033817393827,-116.639796342494,
176.483420797975));
#43405=CARTESIAN_POINT('Ctrl Pts',(-63.6184094068807,-116.711154185119,
174.830711729305));
#43406=CARTESIAN_POINT('Ctrl Pts',(-62.6113106544147,-116.91279886901,173.516227941122));
#43407=CARTESIAN_POINT('Ctrl Pts',(-61.6042119019488,-117.1144435529,172.201744152939));
#43408=CARTESIAN_POINT('Ctrl Pts',(-59.9707531025376,-117.38286240244,171.99549242084));
#43409=CARTESIAN_POINT('Ctrl Pts',(-58.3372943031263,-117.651281251981,
171.789240688742));
#43410=CARTESIAN_POINT('Ctrl Pts',(-57.0401550503603,-117.883846190933,
172.812040480128));
#43411=CARTESIAN_POINT('Ctrl Pts',(-55.7430157975943,-118.116411129886,
173.834840271514));
#43412=CARTESIAN_POINT('Ctrl Pts',(-55.5478642559304,-118.231496816571,
175.487549340184));
#43413=CARTESIAN_POINT('Ctrl Pts',(-55.3527127142665,-118.346582503257,
177.140258408853));
#43414=CARTESIAN_POINT('Ctrl Pts',(-56.3796875925665,-118.331381348677,
178.454742197037));
#43415=CARTESIAN_POINT('Ctrl Pts',(-57.4066624708665,-118.316180194097,
179.76922598522));
#43416=CARTESIAN_POINT('Ctrl Pts',(-59.0599973961117,-118.234204873868,
179.975477717318));
#43417=CARTESIAN_POINT('Ctrl Pts',(-60.713332321357,-118.152229553638,180.181729449417));
#43418=CARTESIAN_POINT('Ctrl Pts',(-62.030347699957,-118.106108143996,179.158929658031));
#43419=CARTESIAN_POINT('Ctrl Pts',(-63.3473630785571,-118.059986734354,
178.136129866644));
#43420=CARTESIAN_POINT('Ctrl Pts',(-63.562390746055,-118.131344576979,176.483420797975));
#43421=CARTESIAN_POINT('Ctrl Pts',(-63.7774184135529,-118.202702419604,
174.830711729305));
#43422=CARTESIAN_POINT('Ctrl Pts',(-62.770319661087,-118.404347103495,173.516227941122));
#43423=CARTESIAN_POINT('Ctrl Pts',(-61.763220908621,-118.605991787386,172.201744152939));
#43424=CARTESIAN_POINT('Ctrl Pts',(-60.1297621092098,-118.874410636926,
171.99549242084));
#43425=CARTESIAN_POINT('Ctrl Pts',(-58.4963033097986,-119.142829486466,
171.789240688742));
#43426=CARTESIAN_POINT('Ctrl Pts',(-57.1991640570326,-119.375394425419,
172.812040480128));
#43427=CARTESIAN_POINT('Ctrl Pts',(-55.9020248042666,-119.607959364371,
173.834840271514));
#43428=CARTESIAN_POINT('Ctrl Pts',(-55.7068732626027,-119.723045051057,
175.487549340184));
#43429=CARTESIAN_POINT('Ctrl Pts',(-55.5117217209387,-119.838130737742,
177.140258408853));
#43430=CARTESIAN_POINT('Ctrl Pts',(-56.5386965992387,-119.822929583163,
178.454742197037));
#43431=CARTESIAN_POINT('Ctrl Pts',(-57.5656714775387,-119.807728428583,
179.76922598522));
#43432=CARTESIAN_POINT('Ctrl Pts',(-59.219006402784,-119.725753108353,179.975477717318));
#43433=CARTESIAN_POINT('Ctrl Pts',(-60.8723413280292,-119.643777788124,
180.181729449417));
#43434=CARTESIAN_POINT('Ctrl Pts',(-62.1893567066292,-119.597656378482,
179.158929658031));
#43435=CARTESIAN_POINT('Ctrl Pts',(-63.5063720852293,-119.55153496884,178.136129866644));
#43436=CARTESIAN_POINT('Ctrl Pts',(-63.7213997527272,-119.622892811465,
176.483420797975));
#43437=CARTESIAN_POINT('Ctrl Pts',(-63.9364274202251,-119.69425065409,174.830711729305));
#43438=CARTESIAN_POINT('Ctrl Pts',(-62.9293286677592,-119.895895337981,
173.516227941122));
#43439=CARTESIAN_POINT('Ctrl Pts',(-61.9222299152932,-120.097540021871,
172.201744152939));
#43440=CARTESIAN_POINT('Ctrl Pts',(-60.288771115882,-120.365958871412,171.99549242084));
#43441=CARTESIAN_POINT('Ctrl Pts',(-58.6553123164708,-120.634377720952,
171.789240688742));
#43442=CARTESIAN_POINT('Ctrl Pts',(-57.3581730637048,-120.866942659904,
172.812040480128));
#43443=CARTESIAN_POINT('Ctrl Pts',(-56.0610338109388,-121.099507598857,
173.834840271514));
#43444=CARTESIAN_POINT('Ctrl Pts',(-55.8658822692749,-121.214593285542,
175.487549340184));
#43445=CARTESIAN_POINT('Ctrl Pts',(-55.670730727611,-121.329678972228,177.140258408853));
#43446=CARTESIAN_POINT('Ctrl Pts',(-56.697705605911,-121.314477817648,178.454742197037));
#43447=CARTESIAN_POINT('Ctrl Pts',(-57.7246804842109,-121.299276663068,
179.76922598522));
#43448=CARTESIAN_POINT('Ctrl Pts',(-59.3780154094562,-121.217301342839,
179.975477717318));
#43449=CARTESIAN_POINT('Ctrl Pts',(-61.0313503347014,-121.135326022609,
180.181729449417));
#43450=CARTESIAN_POINT('Ctrl Pts',(-62.3483657133015,-121.089204612967,
179.158929658031));
#43451=CARTESIAN_POINT('Ctrl Pts',(-63.6653810919015,-121.043083203326,
178.136129866644));
#43452=CARTESIAN_POINT('Ctrl Pts',(-63.8804087593994,-121.114441045951,
176.483420797975));
#43453=CARTESIAN_POINT('Ctrl Pts',(-64.0954364268974,-121.185798888576,
174.830711729305));
#43454=CARTESIAN_POINT('Ctrl Pts',(-63.0883376744314,-121.387443572466,
173.516227941122));
#43455=CARTESIAN_POINT('Ctrl Pts',(-62.0812389219655,-121.589088256357,
172.201744152939));
#43456=CARTESIAN_POINT('Ctrl Pts',(-60.4477801225542,-121.857507105897,
171.99549242084));
#43457=CARTESIAN_POINT('Ctrl Pts',(-58.814321323143,-122.125925955437,171.789240688742));
#43458=CARTESIAN_POINT('Ctrl Pts',(-57.517182070377,-122.35849089439,172.812040480128));
#43459=CARTESIAN_POINT('Ctrl Pts',(-56.220042817611,-122.591055833342,173.834840271514));
#43460=CARTESIAN_POINT('Ctrl Pts',(-56.0248912759471,-122.706141520028,
175.487549340184));
#43461=CARTESIAN_POINT('Ctrl Pts',(-55.8297397342832,-122.821227206714,
177.140258408853));
#43462=CARTESIAN_POINT('Ctrl Pts',(-56.8567146125832,-122.806026052134,
178.454742197037));
#43463=CARTESIAN_POINT('Ctrl Pts',(-57.8836894908832,-122.790824897554,
179.76922598522));
#43464=CARTESIAN_POINT('Ctrl Pts',(-59.5370244161284,-122.708849577324,
179.975477717318));
#43465=CARTESIAN_POINT('Ctrl Pts',(-61.1903593413737,-122.626874257095,
180.181729449417));
#43466=CARTESIAN_POINT('Ctrl Pts',(-62.5073747199737,-122.580752847453,
179.158929658031));
#43467=CARTESIAN_POINT('Ctrl Pts',(-63.8243900985737,-122.534631437811,
178.136129866644));
#43468=CARTESIAN_POINT('Ctrl Pts',(-64.0394177660717,-122.605989280436,
176.483420797975));
#43469=CARTESIAN_POINT('Ctrl Pts',(-64.2544454335696,-122.677347123061,
174.830711729305));
#43470=CARTESIAN_POINT('Ctrl Pts',(-63.2473466811036,-122.878991806952,
173.516227941122));
#43471=CARTESIAN_POINT('Ctrl Pts',(-62.2402479286377,-123.080636490843,
172.201744152939));
#43472=CARTESIAN_POINT('Ctrl Pts',(-60.6067891292265,-123.349055340383,
171.99549242084));
#43473=CARTESIAN_POINT('Ctrl Pts',(-58.9733303298152,-123.617474189923,
171.789240688742));
#43474=CARTESIAN_POINT('Ctrl Pts',(-57.6761910770492,-123.850039128875,
172.812040480128));
#43475=CARTESIAN_POINT('Ctrl Pts',(-56.3790518242832,-124.082604067828,
173.834840271514));
#43476=CARTESIAN_POINT('Ctrl Pts',(-56.1839002826193,-124.197689754514,
175.487549340184));
#43477=CARTESIAN_POINT('Ctrl Pts',(-55.9887487409554,-124.312775441199,
177.140258408853));
#43478=CARTESIAN_POINT('Ctrl Pts',(-57.0157236192554,-124.297574286619,
178.454742197037));
#43479=CARTESIAN_POINT('Ctrl Pts',(-58.0426984975554,-124.282373132039,
179.76922598522));
#43480=CARTESIAN_POINT('Ctrl Pts',(-59.6960334228006,-124.20039781181,179.975477717318));
#43481=CARTESIAN_POINT('Ctrl Pts',(-61.3493683480459,-124.11842249158,180.181729449417));
#43482=CARTESIAN_POINT('Ctrl Pts',(-62.6663837266459,-124.072301081939,
179.158929658031));
#43483=CARTESIAN_POINT('Ctrl Pts',(-63.983399105246,-124.026179672297,178.136129866644));
#43484=CARTESIAN_POINT('Ctrl Pts',(-64.1984267727439,-124.097537514922,
176.483420797975));
#43485=CARTESIAN_POINT('Ctrl Pts',(-64.4134544402418,-124.168895357547,
174.830711729305));
#43486=CARTESIAN_POINT('Ctrl Pts',(-63.4063556877759,-124.370540041437,
173.516227941122));
#43487=CARTESIAN_POINT('Ctrl Pts',(-62.3992569353099,-124.572184725328,
172.201744152939));
#43488=CARTESIAN_POINT('Ctrl Pts',(-60.7657981358987,-124.840603574868,
171.99549242084));
#43489=CARTESIAN_POINT('Ctrl Pts',(-59.1323393364875,-125.109022424409,
171.789240688742));
#43490=CARTESIAN_POINT('Ctrl Pts',(-57.8352000837215,-125.341587363361,
172.812040480128));
#43491=CARTESIAN_POINT('Ctrl Pts',(-56.5380608309555,-125.574152302314,
173.834840271514));
#43492=CARTESIAN_POINT('Ctrl Pts',(-56.3429092892916,-125.689237988999,
175.487549340184));
#43493=CARTESIAN_POINT('Ctrl Pts',(-56.1477577476277,-125.804323675685,
177.140258408853));
#43494=CARTESIAN_POINT('Ctrl Pts',(-57.1747326259276,-125.789122521105,
178.454742197037));
#43495=CARTESIAN_POINT('Ctrl Pts',(-58.2017075042276,-125.773921366525,
179.76922598522));
#43496=CARTESIAN_POINT('Ctrl Pts',(-59.8550424294729,-125.691946046296,
179.975477717318));
#43497=CARTESIAN_POINT('Ctrl Pts',(-61.5083773547181,-125.609970726066,
180.181729449417));
#43498=CARTESIAN_POINT('Ctrl Pts',(-62.8253927333181,-125.563849316424,
179.158929658031));
#43499=CARTESIAN_POINT('Ctrl Pts',(-64.1424081119182,-125.517727906782,
178.136129866644));
#43500=CARTESIAN_POINT('Ctrl Pts',(-64.3574357794161,-125.589085749407,
176.483420797975));
#43501=CARTESIAN_POINT('Ctrl Pts',(-64.572463446914,-125.660443592032,174.830711729305));
#43502=CARTESIAN_POINT('Ctrl Pts',(-63.5653646944481,-125.862088275923,
173.516227941122));
#43503=CARTESIAN_POINT('Ctrl Pts',(-62.5582659419822,-126.063732959814,
172.201744152939));
#43504=CARTESIAN_POINT('Ctrl Pts',(-60.9248071425709,-126.332151809354,
171.99549242084));
#43505=CARTESIAN_POINT('Ctrl Pts',(-59.2913483431597,-126.600570658894,
171.789240688742));
#43506=CARTESIAN_POINT('Ctrl Pts',(-57.9942090903937,-126.833135597847,
172.812040480128));
#43507=CARTESIAN_POINT('Ctrl Pts',(-56.6970698376277,-127.065700536799,
173.834840271514));
#43508=CARTESIAN_POINT('Ctrl Pts',(-56.5019182959638,-127.180786223485,
175.487549340184));
#43509=CARTESIAN_POINT('Ctrl Pts',(-56.3067667542999,-127.295871910171,
177.140258408853));
#43510=CARTESIAN_POINT('Ctrl Pts',(-57.3337416325999,-127.280670755591,
178.454742197037));
#43511=CARTESIAN_POINT('Ctrl Pts',(-58.3607165108998,-127.265469601011,
179.76922598522));
#43512=CARTESIAN_POINT('Ctrl Pts',(-60.0140514361451,-127.183494280781,
179.975477717318));
#43513=CARTESIAN_POINT('Ctrl Pts',(-61.6673863613903,-127.101518960552,
180.181729449417));
#43514=CARTESIAN_POINT('Ctrl Pts',(-62.9844017399904,-127.05539755091,179.158929658031));
#43515=CARTESIAN_POINT('Ctrl Pts',(-64.3014171185904,-127.009276141268,
178.136129866644));
#43516=CARTESIAN_POINT('Ctrl Pts',(-64.5164447860883,-127.080633983893,
176.483420797975));
#43517=CARTESIAN_POINT('Ctrl Pts',(-64.7314724535863,-127.151991826518,
174.830711729305));
#43518=CARTESIAN_POINT('Ctrl Pts',(-63.7243737011203,-127.353636510409,
173.516227941122));
#43519=CARTESIAN_POINT('Ctrl Pts',(-62.7172749486544,-127.555281194299,
172.201744152939));
#43520=CARTESIAN_POINT('Ctrl Pts',(-61.0838161492432,-127.82370004384,171.99549242084));
#43521=CARTESIAN_POINT('Ctrl Pts',(-59.4503573498319,-128.09211889338,171.789240688742));
#43522=CARTESIAN_POINT('Ctrl Pts',(-58.1532180970659,-128.324683832332,
172.812040480128));
#43523=CARTESIAN_POINT('Ctrl Pts',(-56.8560788442999,-128.557248771285,
173.834840271514));
#43524=CARTESIAN_POINT('Ctrl Pts',(-56.660927302636,-128.67233445797,175.487549340184));
#43525=CARTESIAN_POINT('Ctrl Pts',(-56.4657757609721,-128.787420144656,
177.140258408853));
#43526=CARTESIAN_POINT('Ctrl Pts',(-57.4927506392721,-128.772218990076,
178.454742197037));
#43527=CARTESIAN_POINT('Ctrl Pts',(-58.5197255175721,-128.757017835496,
179.76922598522));
#43528=CARTESIAN_POINT('Ctrl Pts',(-60.1730604428173,-128.675042515267,
179.975477717318));
#43529=CARTESIAN_POINT('Ctrl Pts',(-61.8263953680626,-128.593067195037,
180.181729449417));
#43530=CARTESIAN_POINT('Ctrl Pts',(-63.1434107466626,-128.546945785395,
179.158929658031));
#43531=CARTESIAN_POINT('Ctrl Pts',(-64.4604261252626,-128.500824375754,
178.136129866644));
#43532=CARTESIAN_POINT('Ctrl Pts',(-64.6754537927606,-128.572182218379,
176.483420797975));
#43533=CARTESIAN_POINT('Ctrl Pts',(-64.8904814602585,-128.643540061004,
174.830711729305));
#43534=CARTESIAN_POINT('Ctrl Pts',(-63.8833827077925,-128.845184744894,
173.516227941122));
#43535=CARTESIAN_POINT('Ctrl Pts',(-62.8762839553266,-129.046829428785,
172.201744152939));
#43536=CARTESIAN_POINT('Ctrl Pts',(-61.2428251559154,-129.315248278325,
171.99549242084));
#43537=CARTESIAN_POINT('Ctrl Pts',(-59.6093663565042,-129.583667127865,
171.789240688742));
#43538=CARTESIAN_POINT('Ctrl Pts',(-58.3122271037382,-129.816232066818,
172.812040480128));
#43539=CARTESIAN_POINT('Ctrl Pts',(-57.0150878509721,-130.04879700577,173.834840271514));
#43540=CARTESIAN_POINT('Ctrl Pts',(-56.8199363093082,-130.163882692456,
175.487549340184));
#43541=CARTESIAN_POINT('Ctrl Pts',(-56.6247847676443,-130.278968379142,
177.140258408853));
#43542=CARTESIAN_POINT('Ctrl Pts',(-57.6517596459443,-130.263767224562,
178.454742197037));
#43543=CARTESIAN_POINT('Ctrl Pts',(-58.6787345242443,-130.248566069982,
179.76922598522));
#43544=CARTESIAN_POINT('Ctrl Pts',(-60.3320694494895,-130.166590749752,
179.975477717318));
#43545=CARTESIAN_POINT('Ctrl Pts',(-61.9854043747348,-130.084615429523,
180.181729449417));
#43546=CARTESIAN_POINT('Ctrl Pts',(-63.3024197533348,-130.038494019881,
179.158929658031));
#43547=CARTESIAN_POINT('Ctrl Pts',(-64.6194351319349,-129.992372610239,
178.136129866644));
#43548=CARTESIAN_POINT('Ctrl Pts',(-64.8344627994328,-130.063730452864,
176.483420797975));
#43549=CARTESIAN_POINT('Ctrl Pts',(-65.0494904669307,-130.135088295489,
174.830711729305));
#43550=CARTESIAN_POINT('Ctrl Pts',(-64.0423917144648,-130.33673297938,173.516227941122));
#43551=CARTESIAN_POINT('Ctrl Pts',(-63.0352929619988,-130.538377663271,
172.201744152939));
#43552=CARTESIAN_POINT('Ctrl Pts',(-61.4018341625876,-130.806796512811,
171.99549242084));
#43553=CARTESIAN_POINT('Ctrl Pts',(-59.7683753631764,-131.075215362351,
171.789240688742));
#43554=CARTESIAN_POINT('Ctrl Pts',(-58.4712361104104,-131.307780301304,
172.812040480128));
#43555=CARTESIAN_POINT('Ctrl Pts',(-57.1740968576444,-131.540345240256,
173.834840271514));
#43556=CARTESIAN_POINT('Ctrl Pts',(-56.9789453159805,-131.655430926942,
175.487549340184));
#43557=CARTESIAN_POINT('Ctrl Pts',(-56.7837937743166,-131.770516613627,
177.140258408853));
#43558=CARTESIAN_POINT('Ctrl Pts',(-57.8107686526165,-131.755315459047,
178.454742197037));
#43559=CARTESIAN_POINT('Ctrl Pts',(-58.8377435309165,-131.740114304467,
179.76922598522));
#43560=CARTESIAN_POINT('Ctrl Pts',(-60.4910784561618,-131.658138984238,
179.975477717318));
#43561=CARTESIAN_POINT('Ctrl Pts',(-61.5605751224754,-131.605111415312,
180.108896262184));
#43562=CARTESIAN_POINT('Ctrl Pts',(-62.5544558090293,-131.564605289581,
179.689905107434));
#43563=CARTESIAN_POINT('Ctrl Pts',(-50.1798438064916,-67.6819458883961,
175.490142808619));
#43564=CARTESIAN_POINT('Ctrl Pts',(-49.9857604617556,-67.7969176981527,
177.134243841043));
#43565=CARTESIAN_POINT('Ctrl Pts',(-51.0074381646872,-67.7822812578569,
178.441881219107));
#43566=CARTESIAN_POINT('Ctrl Pts',(-52.0291158676188,-67.7676448175611,
179.74951859717));
#43567=CARTESIAN_POINT('Ctrl Pts',(-53.673891258688,-67.6865820008601,179.954696079469));
#43568=CARTESIAN_POINT('Ctrl Pts',(-55.3186666497572,-67.6055191841591,
180.159873561769));
#43569=CARTESIAN_POINT('Ctrl Pts',(-56.6288741944062,-67.5601235350989,
179.142400961866));
#43570=CARTESIAN_POINT('Ctrl Pts',(-57.9390817390552,-67.5147278860387,
178.124928361964));
#43571=CARTESIAN_POINT('Ctrl Pts',(-58.1530412096253,-67.5861996055927,
176.48082732954));
#43572=CARTESIAN_POINT('Ctrl Pts',(-58.3670006801954,-67.6576713251468,
174.836726297116));
#43573=CARTESIAN_POINT('Ctrl Pts',(-57.3651991030978,-67.8587512947533,
173.529088919052));
#43574=CARTESIAN_POINT('Ctrl Pts',(-56.3633975260002,-68.0598312643598,
172.221451540989));
#43575=CARTESIAN_POINT('Ctrl Pts',(-54.7384982607651,-68.3273376103715,
172.016274058689));
#43576=CARTESIAN_POINT('Ctrl Pts',(-53.1135989955299,-68.5948439563832,
171.81109657639));
#43577=CARTESIAN_POINT('Ctrl Pts',(-51.8232675767149,-68.8266831347541,
172.828569176292));
#43578=CARTESIAN_POINT('Ctrl Pts',(-50.5329361578999,-69.0585223131251,
173.846041776195));
#43579=CARTESIAN_POINT('Ctrl Pts',(-50.3388528131639,-69.1734941228817,
175.490142808619));
#43580=CARTESIAN_POINT('Ctrl Pts',(-50.1447694684278,-69.2884659326383,
177.134243841043));
#43581=CARTESIAN_POINT('Ctrl Pts',(-51.1664471713594,-69.2738294923425,
178.441881219107));
#43582=CARTESIAN_POINT('Ctrl Pts',(-52.188124874291,-69.2591930520467,179.74951859717));
#43583=CARTESIAN_POINT('Ctrl Pts',(-53.8329002653602,-69.1781302353457,
179.954696079469));
#43584=CARTESIAN_POINT('Ctrl Pts',(-55.4776756564294,-69.0970674186447,
180.159873561769));
#43585=CARTESIAN_POINT('Ctrl Pts',(-56.7878832010784,-69.0516717695845,
179.142400961866));
#43586=CARTESIAN_POINT('Ctrl Pts',(-58.0980907457274,-69.0062761205243,
178.124928361964));
#43587=CARTESIAN_POINT('Ctrl Pts',(-58.3120502162975,-69.0777478400783,
176.48082732954));
#43588=CARTESIAN_POINT('Ctrl Pts',(-58.5260096868676,-69.1492195596324,
174.836726297116));
#43589=CARTESIAN_POINT('Ctrl Pts',(-57.52420810977,-69.3502995292389,173.529088919052));
#43590=CARTESIAN_POINT('Ctrl Pts',(-56.5224065326725,-69.5513794988454,
172.221451540989));
#43591=CARTESIAN_POINT('Ctrl Pts',(-54.8975072674373,-69.8188858448571,
172.016274058689));
#43592=CARTESIAN_POINT('Ctrl Pts',(-53.2726080022022,-70.0863921908688,
171.81109657639));
#43593=CARTESIAN_POINT('Ctrl Pts',(-51.9822765833872,-70.3182313692397,
172.828569176292));
#43594=CARTESIAN_POINT('Ctrl Pts',(-50.6919451645722,-70.5500705476106,
173.846041776195));
#43595=CARTESIAN_POINT('Ctrl Pts',(-50.4978618198361,-70.6650423573673,
175.490142808619));
#43596=CARTESIAN_POINT('Ctrl Pts',(-50.3037784751,-70.7800141671239,177.134243841043));
#43597=CARTESIAN_POINT('Ctrl Pts',(-51.3254561780316,-70.7653777268281,
178.441881219107));
#43598=CARTESIAN_POINT('Ctrl Pts',(-52.3471338809632,-70.7507412865323,
179.74951859717));
#43599=CARTESIAN_POINT('Ctrl Pts',(-53.9919092720324,-70.6696784698313,
179.954696079469));
#43600=CARTESIAN_POINT('Ctrl Pts',(-55.6366846631016,-70.5886156531303,
180.159873561769));
#43601=CARTESIAN_POINT('Ctrl Pts',(-56.9468922077507,-70.5432200040701,
179.142400961866));
#43602=CARTESIAN_POINT('Ctrl Pts',(-58.2570997523997,-70.4978243550099,
178.124928361964));
#43603=CARTESIAN_POINT('Ctrl Pts',(-58.4710592229698,-70.5692960745639,
176.48082732954));
#43604=CARTESIAN_POINT('Ctrl Pts',(-58.6850186935399,-70.640767794118,174.836726297116));
#43605=CARTESIAN_POINT('Ctrl Pts',(-57.6832171164423,-70.8418477637245,
173.529088919052));
#43606=CARTESIAN_POINT('Ctrl Pts',(-56.6814155393447,-71.0429277333309,
172.221451540989));
#43607=CARTESIAN_POINT('Ctrl Pts',(-55.0565162741095,-71.3104340793427,
172.016274058689));
#43608=CARTESIAN_POINT('Ctrl Pts',(-53.4316170088744,-71.5779404253544,
171.81109657639));
#43609=CARTESIAN_POINT('Ctrl Pts',(-52.1412855900594,-71.8097796037253,
172.828569176292));
#43610=CARTESIAN_POINT('Ctrl Pts',(-50.8509541712444,-72.0416187820962,
173.846041776195));
#43611=CARTESIAN_POINT('Ctrl Pts',(-50.6568708265083,-72.1565905918529,
175.490142808619));
#43612=CARTESIAN_POINT('Ctrl Pts',(-50.4627874817723,-72.2715624016095,
177.134243841043));
#43613=CARTESIAN_POINT('Ctrl Pts',(-51.4844651847039,-72.2569259613137,
178.441881219107));
#43614=CARTESIAN_POINT('Ctrl Pts',(-52.5061428876355,-72.242289521018,179.74951859717));
#43615=CARTESIAN_POINT('Ctrl Pts',(-54.1509182787047,-72.1612267043169,
179.954696079469));
#43616=CARTESIAN_POINT('Ctrl Pts',(-55.7956936697739,-72.0801638876159,
180.159873561769));
#43617=CARTESIAN_POINT('Ctrl Pts',(-57.1059012144229,-72.0347682385557,
179.142400961866));
#43618=CARTESIAN_POINT('Ctrl Pts',(-58.4161087590719,-71.9893725894955,
178.124928361964));
#43619=CARTESIAN_POINT('Ctrl Pts',(-58.630068229642,-72.0608443090495,176.48082732954));
#43620=CARTESIAN_POINT('Ctrl Pts',(-58.8440277002121,-72.1323160286036,
174.836726297116));
#43621=CARTESIAN_POINT('Ctrl Pts',(-57.8422261231145,-72.3333959982101,
173.529088919052));
#43622=CARTESIAN_POINT('Ctrl Pts',(-56.8404245460169,-72.5344759678166,
172.221451540989));
#43623=CARTESIAN_POINT('Ctrl Pts',(-55.2155252807818,-72.8019823138283,
172.016274058689));
#43624=CARTESIAN_POINT('Ctrl Pts',(-53.5906260155466,-73.06948865984,171.81109657639));
#43625=CARTESIAN_POINT('Ctrl Pts',(-52.3002945967316,-73.3013278382109,
172.828569176292));
#43626=CARTESIAN_POINT('Ctrl Pts',(-51.0099631779166,-73.5331670165818,
173.846041776195));
#43627=CARTESIAN_POINT('Ctrl Pts',(-50.8158798331806,-73.6481388263385,
175.490142808619));
#43628=CARTESIAN_POINT('Ctrl Pts',(-50.6217964884445,-73.7631106360951,
177.134243841043));
#43629=CARTESIAN_POINT('Ctrl Pts',(-51.6434741913761,-73.7484741957993,
178.441881219107));
#43630=CARTESIAN_POINT('Ctrl Pts',(-52.6651518943077,-73.7338377555035,
179.74951859717));
#43631=CARTESIAN_POINT('Ctrl Pts',(-54.3099272853769,-73.6527749388025,
179.954696079469));
#43632=CARTESIAN_POINT('Ctrl Pts',(-55.9547026764461,-73.5717121221015,
180.159873561769));
#43633=CARTESIAN_POINT('Ctrl Pts',(-57.2649102210951,-73.5263164730413,
179.142400961866));
#43634=CARTESIAN_POINT('Ctrl Pts',(-58.5751177657441,-73.4809208239811,
178.124928361964));
#43635=CARTESIAN_POINT('Ctrl Pts',(-58.7890772363142,-73.5523925435351,
176.48082732954));
#43636=CARTESIAN_POINT('Ctrl Pts',(-59.0030367068843,-73.6238642630892,
174.836726297116));
#43637=CARTESIAN_POINT('Ctrl Pts',(-58.0012351297867,-73.8249442326957,
173.529088919052));
#43638=CARTESIAN_POINT('Ctrl Pts',(-56.9994335526892,-74.0260242023022,
172.221451540989));
#43639=CARTESIAN_POINT('Ctrl Pts',(-55.374534287454,-74.2935305483139,172.016274058689));
#43640=CARTESIAN_POINT('Ctrl Pts',(-53.7496350222188,-74.5610368943256,
171.81109657639));
#43641=CARTESIAN_POINT('Ctrl Pts',(-52.4593036034038,-74.7928760726965,
172.828569176292));
#43642=CARTESIAN_POINT('Ctrl Pts',(-51.1689721845888,-75.0247152510674,
173.846041776195));
#43643=CARTESIAN_POINT('Ctrl Pts',(-50.9748888398528,-75.1396870608241,
175.490142808619));
#43644=CARTESIAN_POINT('Ctrl Pts',(-50.7808054951167,-75.2546588705807,
177.134243841043));
#43645=CARTESIAN_POINT('Ctrl Pts',(-51.8024831980483,-75.2400224302849,
178.441881219107));
#43646=CARTESIAN_POINT('Ctrl Pts',(-52.8241609009799,-75.2253859899892,
179.74951859717));
#43647=CARTESIAN_POINT('Ctrl Pts',(-54.4689362920491,-75.1443231732881,
179.954696079469));
#43648=CARTESIAN_POINT('Ctrl Pts',(-56.1137116831183,-75.0632603565871,
180.159873561769));
#43649=CARTESIAN_POINT('Ctrl Pts',(-57.4239192277673,-75.0178647075269,
179.142400961866));
#43650=CARTESIAN_POINT('Ctrl Pts',(-58.7341267724164,-74.9724690584666,
178.124928361964));
#43651=CARTESIAN_POINT('Ctrl Pts',(-58.9480862429864,-75.0439407780207,
176.48082732954));
#43652=CARTESIAN_POINT('Ctrl Pts',(-59.1620457135565,-75.1154124975748,
174.836726297116));
#43653=CARTESIAN_POINT('Ctrl Pts',(-58.1602441364589,-75.3164924671813,
173.529088919052));
#43654=CARTESIAN_POINT('Ctrl Pts',(-57.1584425593614,-75.5175724367878,
172.221451540989));
#43655=CARTESIAN_POINT('Ctrl Pts',(-55.5335432941262,-75.7850787827995,
172.016274058689));
#43656=CARTESIAN_POINT('Ctrl Pts',(-53.9086440288911,-76.0525851288112,
171.81109657639));
#43657=CARTESIAN_POINT('Ctrl Pts',(-52.6183126100761,-76.2844243071821,
172.828569176292));
#43658=CARTESIAN_POINT('Ctrl Pts',(-51.3279811912611,-76.5162634855531,
173.846041776195));
#43659=CARTESIAN_POINT('Ctrl Pts',(-51.133897846525,-76.6312352953097,175.490142808619));
#43660=CARTESIAN_POINT('Ctrl Pts',(-50.939814501789,-76.7462071050663,177.134243841043));
#43661=CARTESIAN_POINT('Ctrl Pts',(-51.9614922047205,-76.7315706647705,
178.441881219107));
#43662=CARTESIAN_POINT('Ctrl Pts',(-52.9831699076522,-76.7169342244747,
179.74951859717));
#43663=CARTESIAN_POINT('Ctrl Pts',(-54.6279452987213,-76.6358714077737,
179.954696079469));
#43664=CARTESIAN_POINT('Ctrl Pts',(-56.2727206897905,-76.5548085910727,
180.159873561769));
#43665=CARTESIAN_POINT('Ctrl Pts',(-57.5829282344396,-76.5094129420125,
179.142400961866));
#43666=CARTESIAN_POINT('Ctrl Pts',(-58.8931357790886,-76.4640172929522,
178.124928361964));
#43667=CARTESIAN_POINT('Ctrl Pts',(-59.1070952496587,-76.5354890125063,
176.48082732954));
#43668=CARTESIAN_POINT('Ctrl Pts',(-59.3210547202288,-76.6069607320604,
174.836726297116));
#43669=CARTESIAN_POINT('Ctrl Pts',(-58.3192531431312,-76.8080407016669,
173.529088919052));
#43670=CARTESIAN_POINT('Ctrl Pts',(-57.3174515660336,-77.0091206712734,
172.221451540989));
#43671=CARTESIAN_POINT('Ctrl Pts',(-55.6925523007984,-77.2766270172851,
172.016274058689));
#43672=CARTESIAN_POINT('Ctrl Pts',(-54.0676530355633,-77.5441333632968,
171.81109657639));
#43673=CARTESIAN_POINT('Ctrl Pts',(-52.7773216167483,-77.7759725416677,
172.828569176292));
#43674=CARTESIAN_POINT('Ctrl Pts',(-51.4869901979333,-78.0078117200386,
173.846041776195));
#43675=CARTESIAN_POINT('Ctrl Pts',(-51.2929068531972,-78.1227835297953,
175.490142808619));
#43676=CARTESIAN_POINT('Ctrl Pts',(-51.0988235084612,-78.2377553395519,
177.134243841043));
#43677=CARTESIAN_POINT('Ctrl Pts',(-52.1205012113928,-78.2231188992561,
178.441881219107));
#43678=CARTESIAN_POINT('Ctrl Pts',(-53.1421789143244,-78.2084824589603,
179.74951859717));
#43679=CARTESIAN_POINT('Ctrl Pts',(-54.7869543053936,-78.1274196422593,
179.954696079469));
#43680=CARTESIAN_POINT('Ctrl Pts',(-56.4317296964628,-78.0463568255583,
180.159873561769));
#43681=CARTESIAN_POINT('Ctrl Pts',(-57.7419372411118,-78.0009611764981,
179.142400961866));
#43682=CARTESIAN_POINT('Ctrl Pts',(-59.0521447857608,-77.9555655274379,
178.124928361964));
#43683=CARTESIAN_POINT('Ctrl Pts',(-59.2661042563309,-78.0270372469919,
176.48082732954));
#43684=CARTESIAN_POINT('Ctrl Pts',(-59.480063726901,-78.098508966546,174.836726297116));
#43685=CARTESIAN_POINT('Ctrl Pts',(-58.4782621498034,-78.2995889361525,
173.529088919052));
#43686=CARTESIAN_POINT('Ctrl Pts',(-57.4764605727058,-78.500668905759,172.221451540989));
#43687=CARTESIAN_POINT('Ctrl Pts',(-55.8515613074707,-78.7681752517707,
172.016274058689));
#43688=CARTESIAN_POINT('Ctrl Pts',(-54.2266620422355,-79.0356815977824,
171.81109657639));
#43689=CARTESIAN_POINT('Ctrl Pts',(-52.9363306234205,-79.2675207761533,
172.828569176292));
#43690=CARTESIAN_POINT('Ctrl Pts',(-51.6459992046055,-79.4993599545243,
173.846041776195));
#43691=CARTESIAN_POINT('Ctrl Pts',(-51.4519158598695,-79.6143317642809,
175.490142808619));
#43692=CARTESIAN_POINT('Ctrl Pts',(-51.2578325151334,-79.7293035740375,
177.134243841043));
#43693=CARTESIAN_POINT('Ctrl Pts',(-52.279510218065,-79.7146671337417,178.441881219107));
#43694=CARTESIAN_POINT('Ctrl Pts',(-53.3011879209966,-79.7000306934459,
179.74951859717));
#43695=CARTESIAN_POINT('Ctrl Pts',(-54.9459633120658,-79.6189678767449,
179.954696079469));
#43696=CARTESIAN_POINT('Ctrl Pts',(-56.590738703135,-79.5379050600439,180.159873561769));
#43697=CARTESIAN_POINT('Ctrl Pts',(-57.900946247784,-79.4925094109837,179.142400961866));
#43698=CARTESIAN_POINT('Ctrl Pts',(-59.211153792433,-79.4471137619235,178.124928361964));
#43699=CARTESIAN_POINT('Ctrl Pts',(-59.4251132630031,-79.5185854814775,
176.48082732954));
#43700=CARTESIAN_POINT('Ctrl Pts',(-59.6390727335732,-79.5900572010316,
174.836726297116));
#43701=CARTESIAN_POINT('Ctrl Pts',(-58.6372711564756,-79.7911371706381,
173.529088919052));
#43702=CARTESIAN_POINT('Ctrl Pts',(-57.6354695793781,-79.9922171402446,
172.221451540989));
#43703=CARTESIAN_POINT('Ctrl Pts',(-56.0105703141429,-80.2597234862563,
172.016274058689));
#43704=CARTESIAN_POINT('Ctrl Pts',(-54.3856710489078,-80.527229832268,171.81109657639));
#43705=CARTESIAN_POINT('Ctrl Pts',(-53.0953396300927,-80.7590690106389,
172.828569176292));
#43706=CARTESIAN_POINT('Ctrl Pts',(-51.8050082112778,-80.9909081890099,
173.846041776195));
#43707=CARTESIAN_POINT('Ctrl Pts',(-51.6109248665417,-81.1058799987665,
175.490142808619));
#43708=CARTESIAN_POINT('Ctrl Pts',(-51.4168415218056,-81.2208518085231,
177.134243841043));
#43709=CARTESIAN_POINT('Ctrl Pts',(-52.4385192247372,-81.2062153682273,
178.441881219107));
#43710=CARTESIAN_POINT('Ctrl Pts',(-53.4601969276688,-81.1915789279315,
179.74951859717));
#43711=CARTESIAN_POINT('Ctrl Pts',(-55.104972318738,-81.1105161112305,179.954696079469));
#43712=CARTESIAN_POINT('Ctrl Pts',(-56.7497477098072,-81.0294532945295,
180.159873561769));
#43713=CARTESIAN_POINT('Ctrl Pts',(-58.0599552544562,-80.9840576454693,
179.142400961866));
#43714=CARTESIAN_POINT('Ctrl Pts',(-59.3701627991053,-80.9386619964091,
178.124928361964));
#43715=CARTESIAN_POINT('Ctrl Pts',(-59.5841222696753,-81.0101337159631,
176.48082732954));
#43716=CARTESIAN_POINT('Ctrl Pts',(-59.7980817402454,-81.0816054355172,
174.836726297116));
#43717=CARTESIAN_POINT('Ctrl Pts',(-58.7962801631479,-81.2826854051237,
173.529088919052));
#43718=CARTESIAN_POINT('Ctrl Pts',(-57.7944785860503,-81.4837653747302,
172.221451540989));
#43719=CARTESIAN_POINT('Ctrl Pts',(-56.1695793208151,-81.7512717207419,
172.016274058689));
#43720=CARTESIAN_POINT('Ctrl Pts',(-54.54468005558,-82.0187780667536,171.81109657639));
#43721=CARTESIAN_POINT('Ctrl Pts',(-53.254348636765,-82.2506172451245,172.828569176292));
#43722=CARTESIAN_POINT('Ctrl Pts',(-51.96401721795,-82.4824564234954,173.846041776195));
#43723=CARTESIAN_POINT('Ctrl Pts',(-51.7699338732139,-82.5974282332521,
175.490142808619));
#43724=CARTESIAN_POINT('Ctrl Pts',(-51.5758505284779,-82.7124000430087,
177.134243841043));
#43725=CARTESIAN_POINT('Ctrl Pts',(-52.5975282314095,-82.6977636027129,
178.441881219107));
#43726=CARTESIAN_POINT('Ctrl Pts',(-53.6192059343411,-82.6831271624172,
179.74951859717));
#43727=CARTESIAN_POINT('Ctrl Pts',(-55.2639813254103,-82.6020643457161,
179.954696079469));
#43728=CARTESIAN_POINT('Ctrl Pts',(-56.9087567164794,-82.5210015290151,
180.159873561769));
#43729=CARTESIAN_POINT('Ctrl Pts',(-58.2189642611285,-82.4756058799549,
179.142400961866));
#43730=CARTESIAN_POINT('Ctrl Pts',(-59.5291718057775,-82.4302102308947,
178.124928361964));
#43731=CARTESIAN_POINT('Ctrl Pts',(-59.7431312763476,-82.5016819504488,
176.48082732954));
#43732=CARTESIAN_POINT('Ctrl Pts',(-59.9570907469177,-82.5731536700028,
174.836726297116));
#43733=CARTESIAN_POINT('Ctrl Pts',(-58.9552891698201,-82.7742336396093,
173.529088919052));
#43734=CARTESIAN_POINT('Ctrl Pts',(-57.9534875927225,-82.9753136092158,
172.221451540989));
#43735=CARTESIAN_POINT('Ctrl Pts',(-56.3285883274873,-83.2428199552275,
172.016274058689));
#43736=CARTESIAN_POINT('Ctrl Pts',(-54.7036890622522,-83.5103263012392,
171.81109657639));
#43737=CARTESIAN_POINT('Ctrl Pts',(-53.4133576434372,-83.7421654796101,
172.828569176292));
#43738=CARTESIAN_POINT('Ctrl Pts',(-52.1230262246222,-83.9740046579811,
173.846041776195));
#43739=CARTESIAN_POINT('Ctrl Pts',(-51.9289428798862,-84.0889764677377,
175.490142808619));
#43740=CARTESIAN_POINT('Ctrl Pts',(-51.7348595351501,-84.2039482774943,
177.134243841043));
#43741=CARTESIAN_POINT('Ctrl Pts',(-52.7565372380817,-84.1893118371985,
178.441881219107));
#43742=CARTESIAN_POINT('Ctrl Pts',(-53.7782149410133,-84.1746753969028,
179.74951859717));
#43743=CARTESIAN_POINT('Ctrl Pts',(-55.4229903320825,-84.0936125802018,
179.954696079469));
#43744=CARTESIAN_POINT('Ctrl Pts',(-57.0677657231517,-84.0125497635007,
180.159873561769));
#43745=CARTESIAN_POINT('Ctrl Pts',(-58.3779732678007,-83.9671541144405,
179.142400961866));
#43746=CARTESIAN_POINT('Ctrl Pts',(-59.6881808124497,-83.9217584653803,
178.124928361964));
#43747=CARTESIAN_POINT('Ctrl Pts',(-59.9021402830198,-83.9932301849343,
176.48082732954));
#43748=CARTESIAN_POINT('Ctrl Pts',(-60.1160997535899,-84.0647019044884,
174.836726297116));
#43749=CARTESIAN_POINT('Ctrl Pts',(-59.1142981764923,-84.2657818740949,
173.529088919052));
#43750=CARTESIAN_POINT('Ctrl Pts',(-58.1124965993947,-84.4668618437014,
172.221451540989));
#43751=CARTESIAN_POINT('Ctrl Pts',(-56.4875973341596,-84.7343681897131,
172.016274058689));
#43752=CARTESIAN_POINT('Ctrl Pts',(-54.8626980689244,-85.0018745357248,
171.81109657639));
#43753=CARTESIAN_POINT('Ctrl Pts',(-53.5723666501094,-85.2337137140957,
172.828569176292));
#43754=CARTESIAN_POINT('Ctrl Pts',(-52.2820352312944,-85.4655528924667,
173.846041776195));
#43755=CARTESIAN_POINT('Ctrl Pts',(-52.0879518865584,-85.5805247022233,
175.490142808619));
#43756=CARTESIAN_POINT('Ctrl Pts',(-51.8938685418223,-85.6954965119799,
177.134243841043));
#43757=CARTESIAN_POINT('Ctrl Pts',(-52.9155462447539,-85.6808600716841,
178.441881219107));
#43758=CARTESIAN_POINT('Ctrl Pts',(-53.9372239476855,-85.6662236313883,
179.74951859717));
#43759=CARTESIAN_POINT('Ctrl Pts',(-55.5819993387547,-85.5851608146873,
179.954696079469));
#43760=CARTESIAN_POINT('Ctrl Pts',(-57.2267747298239,-85.5040979979863,
180.159873561769));
#43761=CARTESIAN_POINT('Ctrl Pts',(-58.5369822744729,-85.4587023489261,
179.142400961866));
#43762=CARTESIAN_POINT('Ctrl Pts',(-59.847189819122,-85.4133066998659,178.124928361964));
#43763=CARTESIAN_POINT('Ctrl Pts',(-60.061149289692,-85.4847784194199,176.48082732954));
#43764=CARTESIAN_POINT('Ctrl Pts',(-60.2751087602621,-85.556250138974,174.836726297116));
#43765=CARTESIAN_POINT('Ctrl Pts',(-59.2733071831645,-85.7573301085805,
173.529088919052));
#43766=CARTESIAN_POINT('Ctrl Pts',(-58.271505606067,-85.9584100781869,172.221451540989));
#43767=CARTESIAN_POINT('Ctrl Pts',(-56.6466063408318,-86.2259164241987,
172.016274058689));
#43768=CARTESIAN_POINT('Ctrl Pts',(-55.0217070755966,-86.4934227702104,
171.81109657639));
#43769=CARTESIAN_POINT('Ctrl Pts',(-53.7313756567816,-86.7252619485813,
172.828569176292));
#43770=CARTESIAN_POINT('Ctrl Pts',(-52.4410442379667,-86.9571011269522,
173.846041776195));
#43771=CARTESIAN_POINT('Ctrl Pts',(-52.2469608932306,-87.0720729367089,
175.490142808619));
#43772=CARTESIAN_POINT('Ctrl Pts',(-52.0528775484945,-87.1870447464655,
177.134243841043));
#43773=CARTESIAN_POINT('Ctrl Pts',(-53.0745552514261,-87.1724083061697,
178.441881219107));
#43774=CARTESIAN_POINT('Ctrl Pts',(-54.0962329543578,-87.1577718658739,
179.74951859717));
#43775=CARTESIAN_POINT('Ctrl Pts',(-55.7410083454269,-87.0767090491729,
179.954696079469));
#43776=CARTESIAN_POINT('Ctrl Pts',(-57.3857837364961,-86.9956462324719,
180.159873561769));
#43777=CARTESIAN_POINT('Ctrl Pts',(-58.6959912811452,-86.9502505834117,
179.142400961866));
#43778=CARTESIAN_POINT('Ctrl Pts',(-60.0061988257942,-86.9048549343515,
178.124928361964));
#43779=CARTESIAN_POINT('Ctrl Pts',(-60.2201582963643,-86.9763266539055,
176.48082732954));
#43780=CARTESIAN_POINT('Ctrl Pts',(-60.4341177669343,-87.0477983734596,
174.836726297116));
#43781=CARTESIAN_POINT('Ctrl Pts',(-59.4323161898368,-87.2488783430661,
173.529088919052));
#43782=CARTESIAN_POINT('Ctrl Pts',(-58.4305146127392,-87.4499583126726,
172.221451540989));
#43783=CARTESIAN_POINT('Ctrl Pts',(-56.805615347504,-87.7174646586843,172.016274058689));
#43784=CARTESIAN_POINT('Ctrl Pts',(-55.1807160822689,-87.984971004696,171.81109657639));
#43785=CARTESIAN_POINT('Ctrl Pts',(-53.8903846634539,-88.2168101830669,
172.828569176292));
#43786=CARTESIAN_POINT('Ctrl Pts',(-52.6000532446389,-88.4486493614378,
173.846041776195));
#43787=CARTESIAN_POINT('Ctrl Pts',(-52.4059698999028,-88.5636211711945,
175.490142808619));
#43788=CARTESIAN_POINT('Ctrl Pts',(-52.2118865551668,-88.6785929809511,
177.134243841043));
#43789=CARTESIAN_POINT('Ctrl Pts',(-53.2335642580984,-88.6639565406553,
178.441881219107));
#43790=CARTESIAN_POINT('Ctrl Pts',(-54.25524196103,-88.6493201003596,179.74951859717));
#43791=CARTESIAN_POINT('Ctrl Pts',(-55.9000173520992,-88.5682572836585,
179.954696079469));
#43792=CARTESIAN_POINT('Ctrl Pts',(-57.5447927431684,-88.4871944669575,
180.159873561769));
#43793=CARTESIAN_POINT('Ctrl Pts',(-58.8550002878174,-88.4417988178973,
179.142400961866));
#43794=CARTESIAN_POINT('Ctrl Pts',(-60.1652078324664,-88.3964031688371,
178.124928361964));
#43795=CARTESIAN_POINT('Ctrl Pts',(-60.3791673030365,-88.4678748883911,
176.48082732954));
#43796=CARTESIAN_POINT('Ctrl Pts',(-60.5931267736066,-88.5393466079452,
174.836726297116));
#43797=CARTESIAN_POINT('Ctrl Pts',(-59.591325196509,-88.7404265775517,173.529088919052));
#43798=CARTESIAN_POINT('Ctrl Pts',(-58.5895236194114,-88.9415065471582,
172.221451540989));
#43799=CARTESIAN_POINT('Ctrl Pts',(-56.9646243541763,-89.2090128931699,
172.016274058689));
#43800=CARTESIAN_POINT('Ctrl Pts',(-55.3397250889411,-89.4765192391816,
171.81109657639));
#43801=CARTESIAN_POINT('Ctrl Pts',(-54.0493936701261,-89.7083584175525,
172.828569176292));
#43802=CARTESIAN_POINT('Ctrl Pts',(-52.7590622513111,-89.9401975959235,
173.846041776195));
#43803=CARTESIAN_POINT('Ctrl Pts',(-52.5649789065751,-90.0551694056801,
175.490142808619));
#43804=CARTESIAN_POINT('Ctrl Pts',(-52.370895561839,-90.1701412154367,177.134243841043));
#43805=CARTESIAN_POINT('Ctrl Pts',(-53.3925732647706,-90.1555047751409,
178.441881219107));
#43806=CARTESIAN_POINT('Ctrl Pts',(-54.4142509677022,-90.1408683348452,
179.74951859717));
#43807=CARTESIAN_POINT('Ctrl Pts',(-56.0590263587714,-90.0598055181441,
179.954696079469));
#43808=CARTESIAN_POINT('Ctrl Pts',(-57.7038017498406,-89.9787427014431,
180.159873561769));
#43809=CARTESIAN_POINT('Ctrl Pts',(-59.0140092944896,-89.9333470523829,
179.142400961866));
#43810=CARTESIAN_POINT('Ctrl Pts',(-60.3242168391386,-89.8879514033226,
178.124928361964));
#43811=CARTESIAN_POINT('Ctrl Pts',(-60.5381763097087,-89.9594231228767,
176.48082732954));
#43812=CARTESIAN_POINT('Ctrl Pts',(-60.7521357802788,-90.0308948424308,
174.836726297116));
#43813=CARTESIAN_POINT('Ctrl Pts',(-59.7503342031812,-90.2319748120373,
173.529088919052));
#43814=CARTESIAN_POINT('Ctrl Pts',(-58.7485326260837,-90.4330547816438,
172.221451540989));
#43815=CARTESIAN_POINT('Ctrl Pts',(-57.1236333608485,-90.7005611276555,
172.016274058689));
#43816=CARTESIAN_POINT('Ctrl Pts',(-55.4987340956133,-90.9680674736672,
171.81109657639));
#43817=CARTESIAN_POINT('Ctrl Pts',(-54.2084026767983,-91.1999066520381,
172.828569176292));
#43818=CARTESIAN_POINT('Ctrl Pts',(-52.9180712579833,-91.431745830409,173.846041776195));
#43819=CARTESIAN_POINT('Ctrl Pts',(-52.7239879132473,-91.5467176401657,
175.490142808619));
#43820=CARTESIAN_POINT('Ctrl Pts',(-52.5299045685112,-91.6616894499223,
177.134243841043));
#43821=CARTESIAN_POINT('Ctrl Pts',(-53.5515822714428,-91.6470530096265,
178.441881219107));
#43822=CARTESIAN_POINT('Ctrl Pts',(-54.5732599743744,-91.6324165693307,
179.74951859717));
#43823=CARTESIAN_POINT('Ctrl Pts',(-56.2180353654436,-91.5513537526297,
179.954696079469));
#43824=CARTESIAN_POINT('Ctrl Pts',(-57.8628107565128,-91.4702909359287,
180.159873561769));
#43825=CARTESIAN_POINT('Ctrl Pts',(-59.1730183011618,-91.4248952868685,
179.142400961866));
#43826=CARTESIAN_POINT('Ctrl Pts',(-60.4832258458109,-91.3794996378083,
178.124928361964));
#43827=CARTESIAN_POINT('Ctrl Pts',(-60.6971853163809,-91.4509713573623,
176.48082732954));
#43828=CARTESIAN_POINT('Ctrl Pts',(-60.911144786951,-91.5224430769164,174.836726297116));
#43829=CARTESIAN_POINT('Ctrl Pts',(-59.9093432098535,-91.7235230465229,
173.529088919052));
#43830=CARTESIAN_POINT('Ctrl Pts',(-58.9075416327559,-91.9246030161294,
172.221451540989));
#43831=CARTESIAN_POINT('Ctrl Pts',(-57.2826423675207,-92.1921093621411,
172.016274058689));
#43832=CARTESIAN_POINT('Ctrl Pts',(-55.6577431022856,-92.4596157081528,
171.81109657639));
#43833=CARTESIAN_POINT('Ctrl Pts',(-54.3674116834706,-92.6914548865237,
172.828569176292));
#43834=CARTESIAN_POINT('Ctrl Pts',(-53.0770802646556,-92.9232940648947,
173.846041776195));
#43835=CARTESIAN_POINT('Ctrl Pts',(-52.8829969199195,-93.0382658746513,
175.490142808619));
#43836=CARTESIAN_POINT('Ctrl Pts',(-52.6889135751835,-93.1532376844079,
177.134243841043));
#43837=CARTESIAN_POINT('Ctrl Pts',(-53.7105912781151,-93.1386012441121,
178.441881219107));
#43838=CARTESIAN_POINT('Ctrl Pts',(-54.7322689810467,-93.1239648038163,
179.74951859717));
#43839=CARTESIAN_POINT('Ctrl Pts',(-56.3770443721158,-93.0429019871153,
179.954696079469));
#43840=CARTESIAN_POINT('Ctrl Pts',(-58.021819763185,-92.9618391704143,180.159873561769));
#43841=CARTESIAN_POINT('Ctrl Pts',(-59.3320273078341,-92.9164435213541,
179.142400961866));
#43842=CARTESIAN_POINT('Ctrl Pts',(-60.6422348524831,-92.8710478722939,
178.124928361964));
#43843=CARTESIAN_POINT('Ctrl Pts',(-60.8561943230532,-92.9425195918479,
176.48082732954));
#43844=CARTESIAN_POINT('Ctrl Pts',(-61.0701537936232,-93.013991311402,174.836726297116));
#43845=CARTESIAN_POINT('Ctrl Pts',(-60.0683522165257,-93.2150712810085,
173.529088919052));
#43846=CARTESIAN_POINT('Ctrl Pts',(-59.0665506394281,-93.416151250615,172.221451540989));
#43847=CARTESIAN_POINT('Ctrl Pts',(-57.4416513741929,-93.6836575966267,
172.016274058689));
#43848=CARTESIAN_POINT('Ctrl Pts',(-55.8167521089578,-93.9511639426384,
171.81109657639));
#43849=CARTESIAN_POINT('Ctrl Pts',(-54.5264206901428,-94.1830031210093,
172.828569176292));
#43850=CARTESIAN_POINT('Ctrl Pts',(-53.2360892713278,-94.4148422993803,
173.846041776195));
#43851=CARTESIAN_POINT('Ctrl Pts',(-53.0420059265917,-94.5298141091369,
175.490142808619));
#43852=CARTESIAN_POINT('Ctrl Pts',(-52.8479225818557,-94.6447859188935,
177.134243841043));
#43853=CARTESIAN_POINT('Ctrl Pts',(-53.8696002847873,-94.6301494785977,
178.441881219107));
#43854=CARTESIAN_POINT('Ctrl Pts',(-54.8912779877189,-94.615513038302,179.74951859717));
#43855=CARTESIAN_POINT('Ctrl Pts',(-56.5360533787881,-94.5344502216009,
179.954696079469));
#43856=CARTESIAN_POINT('Ctrl Pts',(-58.1808287698573,-94.4533874048999,
180.159873561769));
#43857=CARTESIAN_POINT('Ctrl Pts',(-59.4910363145063,-94.4079917558397,
179.142400961866));
#43858=CARTESIAN_POINT('Ctrl Pts',(-60.8012438591553,-94.3625961067795,
178.124928361964));
#43859=CARTESIAN_POINT('Ctrl Pts',(-61.0152033297254,-94.4340678263335,
176.48082732954));
#43860=CARTESIAN_POINT('Ctrl Pts',(-61.2291628002955,-94.5055395458876,
174.836726297116));
#43861=CARTESIAN_POINT('Ctrl Pts',(-60.2273612231979,-94.7066195154941,
173.529088919052));
#43862=CARTESIAN_POINT('Ctrl Pts',(-59.2255596461003,-94.9076994851006,
172.221451540989));
#43863=CARTESIAN_POINT('Ctrl Pts',(-57.6006603808652,-95.1752058311123,
172.016274058689));
#43864=CARTESIAN_POINT('Ctrl Pts',(-55.97576111563,-95.442712177124,171.81109657639));
#43865=CARTESIAN_POINT('Ctrl Pts',(-54.685429696815,-95.6745513554949,172.828569176292));
#43866=CARTESIAN_POINT('Ctrl Pts',(-53.395098278,-95.9063905338659,173.846041776195));
#43867=CARTESIAN_POINT('Ctrl Pts',(-53.201014933264,-96.0213623436225,175.490142808619));
#43868=CARTESIAN_POINT('Ctrl Pts',(-53.0069315885279,-96.1363341533791,
177.134243841043));
#43869=CARTESIAN_POINT('Ctrl Pts',(-54.0286092914595,-96.1216977130833,
178.441881219107));
#43870=CARTESIAN_POINT('Ctrl Pts',(-55.0502869943911,-96.1070612727875,
179.74951859717));
#43871=CARTESIAN_POINT('Ctrl Pts',(-56.6950623854603,-96.0259984560865,
179.954696079469));
#43872=CARTESIAN_POINT('Ctrl Pts',(-58.3398377765295,-95.9449356393855,
180.159873561769));
#43873=CARTESIAN_POINT('Ctrl Pts',(-59.6500453211785,-95.8995399903253,
179.142400961866));
#43874=CARTESIAN_POINT('Ctrl Pts',(-60.9602528658275,-95.8541443412651,
178.124928361964));
#43875=CARTESIAN_POINT('Ctrl Pts',(-61.1742123363976,-95.9256160608192,
176.48082732954));
#43876=CARTESIAN_POINT('Ctrl Pts',(-61.3881718069677,-95.9970877803732,
174.836726297116));
#43877=CARTESIAN_POINT('Ctrl Pts',(-60.3863702298701,-96.1981677499797,
173.529088919052));
#43878=CARTESIAN_POINT('Ctrl Pts',(-59.3845686527726,-96.3992477195862,
172.221451540989));
#43879=CARTESIAN_POINT('Ctrl Pts',(-57.7596693875374,-96.6667540655979,
172.016274058689));
#43880=CARTESIAN_POINT('Ctrl Pts',(-56.1347701223022,-96.9342604116096,
171.81109657639));
#43881=CARTESIAN_POINT('Ctrl Pts',(-54.8444387034872,-97.1660995899806,
172.828569176292));
#43882=CARTESIAN_POINT('Ctrl Pts',(-53.5541072846722,-97.3979387683514,
173.846041776195));
#43883=CARTESIAN_POINT('Ctrl Pts',(-53.3600239399362,-97.5129105781081,
175.490142808619));
#43884=CARTESIAN_POINT('Ctrl Pts',(-53.1659405952001,-97.6278823878647,
177.134243841043));
#43885=CARTESIAN_POINT('Ctrl Pts',(-54.1876182981317,-97.6132459475689,
178.441881219107));
#43886=CARTESIAN_POINT('Ctrl Pts',(-55.2092960010633,-97.5986095072732,
179.74951859717));
#43887=CARTESIAN_POINT('Ctrl Pts',(-56.8540713921325,-97.5175466905721,
179.954696079469));
#43888=CARTESIAN_POINT('Ctrl Pts',(-58.4988467832017,-97.4364838738711,
180.159873561769));
#43889=CARTESIAN_POINT('Ctrl Pts',(-59.8090543278507,-97.3910882248109,
179.142400961866));
#43890=CARTESIAN_POINT('Ctrl Pts',(-61.1192618724998,-97.3456925757507,
178.124928361964));
#43891=CARTESIAN_POINT('Ctrl Pts',(-61.3332213430699,-97.4171642953048,
176.48082732954));
#43892=CARTESIAN_POINT('Ctrl Pts',(-61.5471808136399,-97.4886360148588,
174.836726297116));
#43893=CARTESIAN_POINT('Ctrl Pts',(-60.5453792365424,-97.6897159844653,
173.529088919052));
#43894=CARTESIAN_POINT('Ctrl Pts',(-59.5435776594448,-97.8907959540718,
172.221451540989));
#43895=CARTESIAN_POINT('Ctrl Pts',(-57.9186783942096,-98.1583023000835,
172.016274058689));
#43896=CARTESIAN_POINT('Ctrl Pts',(-56.2937791289745,-98.4258086460952,
171.81109657639));
#43897=CARTESIAN_POINT('Ctrl Pts',(-55.0034477101595,-98.6576478244661,
172.828569176292));
#43898=CARTESIAN_POINT('Ctrl Pts',(-53.7131162913445,-98.8894870028371,
173.846041776195));
#43899=CARTESIAN_POINT('Ctrl Pts',(-53.5190329466084,-99.0044588125937,
175.490142808619));
#43900=CARTESIAN_POINT('Ctrl Pts',(-53.3249496018724,-99.1194306223503,
177.134243841043));
#43901=CARTESIAN_POINT('Ctrl Pts',(-54.346627304804,-99.1047941820545,178.441881219107));
#43902=CARTESIAN_POINT('Ctrl Pts',(-55.3683050077356,-99.0901577417588,
179.74951859717));
#43903=CARTESIAN_POINT('Ctrl Pts',(-57.0130803988047,-99.0090949250577,
179.954696079469));
#43904=CARTESIAN_POINT('Ctrl Pts',(-58.6578557898739,-98.9280321083567,
180.159873561769));
#43905=CARTESIAN_POINT('Ctrl Pts',(-59.968063334523,-98.8826364592965,179.142400961866));
#43906=CARTESIAN_POINT('Ctrl Pts',(-61.278270879172,-98.8372408102363,178.124928361964));
#43907=CARTESIAN_POINT('Ctrl Pts',(-61.4922303497421,-98.9087125297904,
176.48082732954));
#43908=CARTESIAN_POINT('Ctrl Pts',(-61.7061898203122,-98.9801842493444,
174.836726297116));
#43909=CARTESIAN_POINT('Ctrl Pts',(-60.7043882432146,-99.1812642189509,
173.529088919052));
#43910=CARTESIAN_POINT('Ctrl Pts',(-59.702586666117,-99.3823441885574,172.221451540989));
#43911=CARTESIAN_POINT('Ctrl Pts',(-58.0776874008818,-99.6498505345691,
172.016274058689));
#43912=CARTESIAN_POINT('Ctrl Pts',(-56.4527881356467,-99.9173568805808,
171.81109657639));
#43913=CARTESIAN_POINT('Ctrl Pts',(-55.1624567168317,-100.149196058952,
172.828569176292));
#43914=CARTESIAN_POINT('Ctrl Pts',(-53.8721252980167,-100.381035237323,
173.846041776195));
#43915=CARTESIAN_POINT('Ctrl Pts',(-53.6780419532806,-100.496007047079,
175.490142808619));
#43916=CARTESIAN_POINT('Ctrl Pts',(-53.4839586085446,-100.610978856836,
177.134243841043));
#43917=CARTESIAN_POINT('Ctrl Pts',(-54.5056363114762,-100.59634241654,178.441881219107));
#43918=CARTESIAN_POINT('Ctrl Pts',(-55.5273140144078,-100.581705976244,
179.74951859717));
#43919=CARTESIAN_POINT('Ctrl Pts',(-57.172089405477,-100.500643159543,179.954696079469));
#43920=CARTESIAN_POINT('Ctrl Pts',(-58.8168647965462,-100.419580342842,
180.159873561769));
#43921=CARTESIAN_POINT('Ctrl Pts',(-60.1270723411952,-100.374184693782,
179.142400961866));
#43922=CARTESIAN_POINT('Ctrl Pts',(-61.4372798858442,-100.328789044722,
178.124928361964));
#43923=CARTESIAN_POINT('Ctrl Pts',(-61.6512393564143,-100.400260764276,
176.48082732954));
#43924=CARTESIAN_POINT('Ctrl Pts',(-61.8651988269844,-100.47173248383,174.836726297116));
#43925=CARTESIAN_POINT('Ctrl Pts',(-60.8633972498868,-100.672812453437,
173.529088919052));
#43926=CARTESIAN_POINT('Ctrl Pts',(-59.8615956727892,-100.873892423043,
172.221451540989));
#43927=CARTESIAN_POINT('Ctrl Pts',(-58.2366964075541,-101.141398769055,
172.016274058689));
#43928=CARTESIAN_POINT('Ctrl Pts',(-56.6117971423189,-101.408905115066,
171.81109657639));
#43929=CARTESIAN_POINT('Ctrl Pts',(-55.3214657235039,-101.640744293437,
172.828569176292));
#43930=CARTESIAN_POINT('Ctrl Pts',(-54.0311343046889,-101.872583471808,
173.846041776195));
#43931=CARTESIAN_POINT('Ctrl Pts',(-53.8370509599529,-101.987555281565,
175.490142808619));
#43932=CARTESIAN_POINT('Ctrl Pts',(-53.6429676152168,-102.102527091321,
177.134243841043));
#43933=CARTESIAN_POINT('Ctrl Pts',(-54.6646453181484,-102.087890651026,
178.441881219107));
#43934=CARTESIAN_POINT('Ctrl Pts',(-55.68632302108,-102.07325421073,179.74951859717));
#43935=CARTESIAN_POINT('Ctrl Pts',(-57.3310984121492,-101.992191394029,
179.954696079469));
#43936=CARTESIAN_POINT('Ctrl Pts',(-58.9758738032184,-101.911128577328,
180.159873561769));
#43937=CARTESIAN_POINT('Ctrl Pts',(-60.2860813478674,-101.865732928268,
179.142400961866));
#43938=CARTESIAN_POINT('Ctrl Pts',(-61.5962888925164,-101.820337279207,
178.124928361964));
#43939=CARTESIAN_POINT('Ctrl Pts',(-61.8102483630865,-101.891808998762,
176.48082732954));
#43940=CARTESIAN_POINT('Ctrl Pts',(-62.0242078336566,-101.963280718316,
174.836726297116));
#43941=CARTESIAN_POINT('Ctrl Pts',(-61.022406256559,-102.164360687922,173.529088919052));
#43942=CARTESIAN_POINT('Ctrl Pts',(-60.0206046794615,-102.365440657529,
172.221451540989));
#43943=CARTESIAN_POINT('Ctrl Pts',(-58.3957054142263,-102.63294700354,172.016274058689));
#43944=CARTESIAN_POINT('Ctrl Pts',(-56.7708061489911,-102.900453349552,
171.81109657639));
#43945=CARTESIAN_POINT('Ctrl Pts',(-55.4804747301761,-103.132292527923,
172.828569176292));
#43946=CARTESIAN_POINT('Ctrl Pts',(-54.1901433113612,-103.364131706294,
173.846041776195));
#43947=CARTESIAN_POINT('Ctrl Pts',(-53.9960599666251,-103.479103516051,
175.490142808619));
#43948=CARTESIAN_POINT('Ctrl Pts',(-53.801976621889,-103.594075325807,177.134243841043));
#43949=CARTESIAN_POINT('Ctrl Pts',(-54.8236543248206,-103.579438885511,
178.441881219107));
#43950=CARTESIAN_POINT('Ctrl Pts',(-55.8453320277522,-103.564802445216,
179.74951859717));
#43951=CARTESIAN_POINT('Ctrl Pts',(-57.4901074188214,-103.483739628515,
179.954696079469));
#43952=CARTESIAN_POINT('Ctrl Pts',(-59.1348828098906,-103.402676811814,
180.159873561769));
#43953=CARTESIAN_POINT('Ctrl Pts',(-60.4450903545396,-103.357281162753,
179.142400961866));
#43954=CARTESIAN_POINT('Ctrl Pts',(-61.7552978991887,-103.311885513693,
178.124928361964));
#43955=CARTESIAN_POINT('Ctrl Pts',(-61.9692573697588,-103.383357233247,
176.48082732954));
#43956=CARTESIAN_POINT('Ctrl Pts',(-62.1832168403288,-103.454828952801,
174.836726297116));
#43957=CARTESIAN_POINT('Ctrl Pts',(-61.1814152632313,-103.655908922408,
173.529088919052));
#43958=CARTESIAN_POINT('Ctrl Pts',(-60.1796136861337,-103.856988892014,
172.221451540989));
#43959=CARTESIAN_POINT('Ctrl Pts',(-58.5547144208985,-104.124495238026,
172.016274058689));
#43960=CARTESIAN_POINT('Ctrl Pts',(-56.9298151556634,-104.392001584038,
171.81109657639));
#43961=CARTESIAN_POINT('Ctrl Pts',(-55.6394837368484,-104.623840762409,
172.828569176292));
#43962=CARTESIAN_POINT('Ctrl Pts',(-54.3491523180334,-104.855679940779,
173.846041776195));
#43963=CARTESIAN_POINT('Ctrl Pts',(-54.1550689732973,-104.970651750536,
175.490142808619));
#43964=CARTESIAN_POINT('Ctrl Pts',(-53.9609856285613,-105.085623560293,
177.134243841043));
#43965=CARTESIAN_POINT('Ctrl Pts',(-54.9826633314929,-105.070987119997,
178.441881219107));
#43966=CARTESIAN_POINT('Ctrl Pts',(-56.0043410344245,-105.056350679701,
179.74951859717));
#43967=CARTESIAN_POINT('Ctrl Pts',(-57.6491164254937,-104.975287863,179.954696079469));
#43968=CARTESIAN_POINT('Ctrl Pts',(-59.2938918165628,-104.894225046299,
180.159873561769));
#43969=CARTESIAN_POINT('Ctrl Pts',(-60.6040993612119,-104.848829397239,
179.142400961866));
#43970=CARTESIAN_POINT('Ctrl Pts',(-61.9143069058609,-104.803433748179,
178.124928361964));
#43971=CARTESIAN_POINT('Ctrl Pts',(-62.128266376431,-104.874905467733,176.48082732954));
#43972=CARTESIAN_POINT('Ctrl Pts',(-62.3422258470011,-104.946377187287,
174.836726297116));
#43973=CARTESIAN_POINT('Ctrl Pts',(-61.3404242699035,-105.147457156893,
173.529088919052));
#43974=CARTESIAN_POINT('Ctrl Pts',(-60.3386226928059,-105.3485371265,172.221451540989));
#43975=CARTESIAN_POINT('Ctrl Pts',(-58.7137234275708,-105.616043472511,
172.016274058689));
#43976=CARTESIAN_POINT('Ctrl Pts',(-57.0888241623356,-105.883549818523,
171.81109657639));
#43977=CARTESIAN_POINT('Ctrl Pts',(-55.7984927435206,-106.115388996894,
172.828569176292));
#43978=CARTESIAN_POINT('Ctrl Pts',(-54.5081613247056,-106.347228175265,
173.846041776195));
#43979=CARTESIAN_POINT('Ctrl Pts',(-54.3140779799695,-106.462199985022,
175.490142808619));
#43980=CARTESIAN_POINT('Ctrl Pts',(-54.1199946352335,-106.577171794778,
177.134243841043));
#43981=CARTESIAN_POINT('Ctrl Pts',(-55.1416723381651,-106.562535354483,
178.441881219107));
#43982=CARTESIAN_POINT('Ctrl Pts',(-56.1633500410967,-106.547898914187,
179.74951859717));
#43983=CARTESIAN_POINT('Ctrl Pts',(-57.8081254321659,-106.466836097486,
179.954696079469));
#43984=CARTESIAN_POINT('Ctrl Pts',(-59.4529008232351,-106.385773280785,
180.159873561769));
#43985=CARTESIAN_POINT('Ctrl Pts',(-60.7631083678841,-106.340377631725,
179.142400961866));
#43986=CARTESIAN_POINT('Ctrl Pts',(-62.0733159125331,-106.294981982664,
178.124928361964));
#43987=CARTESIAN_POINT('Ctrl Pts',(-62.2872753831032,-106.366453702218,
176.48082732954));
#43988=CARTESIAN_POINT('Ctrl Pts',(-62.5012348536733,-106.437925421772,
174.836726297116));
#43989=CARTESIAN_POINT('Ctrl Pts',(-61.4994332765757,-106.639005391379,
173.529088919052));
#43990=CARTESIAN_POINT('Ctrl Pts',(-60.4976316994782,-106.840085360985,
172.221451540989));
#43991=CARTESIAN_POINT('Ctrl Pts',(-58.872732434243,-107.107591706997,172.016274058689));
#43992=CARTESIAN_POINT('Ctrl Pts',(-57.2478331690078,-107.375098053009,
171.81109657639));
#43993=CARTESIAN_POINT('Ctrl Pts',(-55.9575017501928,-107.60693723138,172.828569176292));
#43994=CARTESIAN_POINT('Ctrl Pts',(-54.6671703313778,-107.838776409751,
173.846041776195));
#43995=CARTESIAN_POINT('Ctrl Pts',(-54.4730869866418,-107.953748219507,
175.490142808619));
#43996=CARTESIAN_POINT('Ctrl Pts',(-54.2790036419057,-108.068720029264,
177.134243841043));
#43997=CARTESIAN_POINT('Ctrl Pts',(-55.3006813448373,-108.054083588968,
178.441881219107));
#43998=CARTESIAN_POINT('Ctrl Pts',(-56.3223590477689,-108.039447148672,
179.74951859717));
#43999=CARTESIAN_POINT('Ctrl Pts',(-57.9671344388381,-107.958384331971,
179.954696079469));
#44000=CARTESIAN_POINT('Ctrl Pts',(-59.6119098299073,-107.87732151527,180.159873561769));
#44001=CARTESIAN_POINT('Ctrl Pts',(-60.9221173745563,-107.83192586621,179.142400961866));
#44002=CARTESIAN_POINT('Ctrl Pts',(-62.2323249192054,-107.78653021715,178.124928361964));
#44003=CARTESIAN_POINT('Ctrl Pts',(-62.4462843897754,-107.858001936704,
176.48082732954));
#44004=CARTESIAN_POINT('Ctrl Pts',(-62.6602438603455,-107.929473656258,
174.836726297116));
#44005=CARTESIAN_POINT('Ctrl Pts',(-61.6584422832479,-108.130553625865,
173.529088919052));
#44006=CARTESIAN_POINT('Ctrl Pts',(-60.6566407061504,-108.331633595471,
172.221451540989));
#44007=CARTESIAN_POINT('Ctrl Pts',(-59.0317414409152,-108.599139941483,
172.016274058689));
#44008=CARTESIAN_POINT('Ctrl Pts',(-57.4068421756801,-108.866646287494,
171.81109657639));
#44009=CARTESIAN_POINT('Ctrl Pts',(-56.1165107568651,-109.098485465865,
172.828569176292));
#44010=CARTESIAN_POINT('Ctrl Pts',(-54.8261793380501,-109.330324644236,
173.846041776195));
#44011=CARTESIAN_POINT('Ctrl Pts',(-54.632095993314,-109.445296453993,175.490142808619));
#44012=CARTESIAN_POINT('Ctrl Pts',(-54.438012648578,-109.56026826375,177.134243841043));
#44013=CARTESIAN_POINT('Ctrl Pts',(-55.4596903515096,-109.545631823454,
178.441881219107));
#44014=CARTESIAN_POINT('Ctrl Pts',(-56.4813680544411,-109.530995383158,
179.74951859717));
#44015=CARTESIAN_POINT('Ctrl Pts',(-58.1261434455103,-109.449932566457,
179.954696079469));
#44016=CARTESIAN_POINT('Ctrl Pts',(-59.7709188365795,-109.368869749756,
180.159873561769));
#44017=CARTESIAN_POINT('Ctrl Pts',(-61.0811263812286,-109.323474100696,
179.142400961866));
#44018=CARTESIAN_POINT('Ctrl Pts',(-62.3913339258776,-109.278078451635,
178.124928361964));
#44019=CARTESIAN_POINT('Ctrl Pts',(-62.6052933964477,-109.34955017119,176.48082732954));
#44020=CARTESIAN_POINT('Ctrl Pts',(-62.8192528670178,-109.421021890744,
174.836726297116));
#44021=CARTESIAN_POINT('Ctrl Pts',(-61.8174512899202,-109.62210186035,173.529088919052));
#44022=CARTESIAN_POINT('Ctrl Pts',(-60.8156497128226,-109.823181829957,
172.221451540989));
#44023=CARTESIAN_POINT('Ctrl Pts',(-59.1907504475874,-110.090688175968,
172.016274058689));
#44024=CARTESIAN_POINT('Ctrl Pts',(-57.5658511823523,-110.35819452198,171.81109657639));
#44025=CARTESIAN_POINT('Ctrl Pts',(-56.2755197635373,-110.590033700351,
172.828569176292));
#44026=CARTESIAN_POINT('Ctrl Pts',(-54.9851883447223,-110.821872878722,
173.846041776195));
#44027=CARTESIAN_POINT('Ctrl Pts',(-54.7911049999862,-110.936844688478,
175.490142808619));
#44028=CARTESIAN_POINT('Ctrl Pts',(-54.5970216552502,-111.051816498235,
177.134243841043));
#44029=CARTESIAN_POINT('Ctrl Pts',(-55.6186993581818,-111.037180057939,
178.441881219107));
#44030=CARTESIAN_POINT('Ctrl Pts',(-56.6403770611134,-111.022543617644,
179.74951859717));
#44031=CARTESIAN_POINT('Ctrl Pts',(-58.2851524521826,-110.941480800943,
179.954696079469));
#44032=CARTESIAN_POINT('Ctrl Pts',(-59.9299278432518,-110.860417984242,
180.159873561769));
#44033=CARTESIAN_POINT('Ctrl Pts',(-61.2401353879008,-110.815022335181,
179.142400961866));
#44034=CARTESIAN_POINT('Ctrl Pts',(-62.5503429325498,-110.769626686121,
178.124928361964));
#44035=CARTESIAN_POINT('Ctrl Pts',(-62.7643024031199,-110.841098405675,
176.48082732954));
#44036=CARTESIAN_POINT('Ctrl Pts',(-62.97826187369,-110.912570125229,174.836726297116));
#44037=CARTESIAN_POINT('Ctrl Pts',(-61.9764602965924,-111.113650094836,
173.529088919052));
#44038=CARTESIAN_POINT('Ctrl Pts',(-60.9746587194948,-111.314730064442,
172.221451540989));
#44039=CARTESIAN_POINT('Ctrl Pts',(-59.3497594542597,-111.582236410454,
172.016274058689));
#44040=CARTESIAN_POINT('Ctrl Pts',(-57.7248601890245,-111.849742756466,
171.81109657639));
#44041=CARTESIAN_POINT('Ctrl Pts',(-56.4345287702095,-112.081581934837,
172.828569176292));
#44042=CARTESIAN_POINT('Ctrl Pts',(-55.1441973513945,-112.313421113207,
173.846041776195));
#44043=CARTESIAN_POINT('Ctrl Pts',(-54.9501140066585,-112.428392922964,
175.490142808619));
#44044=CARTESIAN_POINT('Ctrl Pts',(-54.7560306619224,-112.543364732721,
177.134243841043));
#44045=CARTESIAN_POINT('Ctrl Pts',(-55.777708364854,-112.528728292425,178.441881219107));
#44046=CARTESIAN_POINT('Ctrl Pts',(-56.7993860677856,-112.514091852129,
179.74951859717));
#44047=CARTESIAN_POINT('Ctrl Pts',(-58.4441614588548,-112.433029035428,
179.954696079469));
#44048=CARTESIAN_POINT('Ctrl Pts',(-60.088936849924,-112.351966218727,180.159873561769));
#44049=CARTESIAN_POINT('Ctrl Pts',(-61.399144394573,-112.306570569667,179.142400961866));
#44050=CARTESIAN_POINT('Ctrl Pts',(-62.709351939222,-112.261174920607,178.124928361964));
#44051=CARTESIAN_POINT('Ctrl Pts',(-62.9233114097921,-112.332646640161,
176.48082732954));
#44052=CARTESIAN_POINT('Ctrl Pts',(-63.1372708803622,-112.404118359715,
174.836726297116));
#44053=CARTESIAN_POINT('Ctrl Pts',(-62.1354693032646,-112.605198329321,
173.529088919052));
#44054=CARTESIAN_POINT('Ctrl Pts',(-61.1336677261671,-112.806278298928,
172.221451540989));
#44055=CARTESIAN_POINT('Ctrl Pts',(-59.5087684609319,-113.07378464494,172.016274058689));
#44056=CARTESIAN_POINT('Ctrl Pts',(-57.8838691956967,-113.341290990951,
171.81109657639));
#44057=CARTESIAN_POINT('Ctrl Pts',(-56.5935377768817,-113.573130169322,
172.828569176292));
#44058=CARTESIAN_POINT('Ctrl Pts',(-55.3032063580667,-113.804969347693,
173.846041776195));
#44059=CARTESIAN_POINT('Ctrl Pts',(-55.1091230133307,-113.91994115745,175.490142808619));
#44060=CARTESIAN_POINT('Ctrl Pts',(-54.9150396685946,-114.034912967206,
177.134243841043));
#44061=CARTESIAN_POINT('Ctrl Pts',(-55.9367173715262,-114.020276526911,
178.441881219107));
#44062=CARTESIAN_POINT('Ctrl Pts',(-56.9583950744578,-114.005640086615,
179.74951859717));
#44063=CARTESIAN_POINT('Ctrl Pts',(-58.603170465527,-113.924577269914,179.954696079469));
#44064=CARTESIAN_POINT('Ctrl Pts',(-60.2479458565962,-113.843514453213,
180.159873561769));
#44065=CARTESIAN_POINT('Ctrl Pts',(-61.5581534012452,-113.798118804152,
179.142400961866));
#44066=CARTESIAN_POINT('Ctrl Pts',(-62.8683609458943,-113.752723155092,
178.124928361964));
#44067=CARTESIAN_POINT('Ctrl Pts',(-63.0823204164643,-113.824194874646,
176.48082732954));
#44068=CARTESIAN_POINT('Ctrl Pts',(-63.2962798870344,-113.8956665942,174.836726297116));
#44069=CARTESIAN_POINT('Ctrl Pts',(-62.2944783099369,-114.096746563807,
173.529088919052));
#44070=CARTESIAN_POINT('Ctrl Pts',(-61.2926767328393,-114.297826533413,
172.221451540989));
#44071=CARTESIAN_POINT('Ctrl Pts',(-59.6677774676041,-114.565332879425,
172.016274058689));
#44072=CARTESIAN_POINT('Ctrl Pts',(-58.042878202369,-114.832839225437,171.81109657639));
#44073=CARTESIAN_POINT('Ctrl Pts',(-56.752546783554,-115.064678403808,172.828569176292));
#44074=CARTESIAN_POINT('Ctrl Pts',(-55.462215364739,-115.296517582179,173.846041776195));
#44075=CARTESIAN_POINT('Ctrl Pts',(-55.2681320200029,-115.411489391935,
175.490142808619));
#44076=CARTESIAN_POINT('Ctrl Pts',(-55.0740486752669,-115.526461201692,
177.134243841043));
#44077=CARTESIAN_POINT('Ctrl Pts',(-56.0957263781985,-115.511824761396,
178.441881219107));
#44078=CARTESIAN_POINT('Ctrl Pts',(-57.1174040811301,-115.4971883211,179.74951859717));
#44079=CARTESIAN_POINT('Ctrl Pts',(-58.7621794721992,-115.416125504399,
179.954696079469));
#44080=CARTESIAN_POINT('Ctrl Pts',(-60.4069548632684,-115.335062687698,
180.159873561769));
#44081=CARTESIAN_POINT('Ctrl Pts',(-61.7171624079175,-115.289667038638,
179.142400961866));
#44082=CARTESIAN_POINT('Ctrl Pts',(-63.0273699525665,-115.244271389578,
178.124928361964));
#44083=CARTESIAN_POINT('Ctrl Pts',(-63.2413294231366,-115.315743109132,
176.48082732954));
#44084=CARTESIAN_POINT('Ctrl Pts',(-63.4552888937067,-115.387214828686,
174.836726297116));
#44085=CARTESIAN_POINT('Ctrl Pts',(-62.4534873166091,-115.588294798292,
173.529088919052));
#44086=CARTESIAN_POINT('Ctrl Pts',(-61.4516857395115,-115.789374767899,
172.221451540989));
#44087=CARTESIAN_POINT('Ctrl Pts',(-59.8267864742763,-116.056881113911,
172.016274058689));
#44088=CARTESIAN_POINT('Ctrl Pts',(-58.2018872090412,-116.324387459922,
171.81109657639));
#44089=CARTESIAN_POINT('Ctrl Pts',(-56.9115557902262,-116.556226638293,
172.828569176292));
#44090=CARTESIAN_POINT('Ctrl Pts',(-55.6212243714112,-116.788065816664,
173.846041776195));
#44091=CARTESIAN_POINT('Ctrl Pts',(-55.4271410266751,-116.903037626421,
175.490142808619));
#44092=CARTESIAN_POINT('Ctrl Pts',(-55.2330576819391,-117.018009436177,
177.134243841043));
#44093=CARTESIAN_POINT('Ctrl Pts',(-56.2547353848707,-117.003372995882,
178.441881219107));
#44094=CARTESIAN_POINT('Ctrl Pts',(-57.2764130878023,-116.988736555586,
179.74951859717));
#44095=CARTESIAN_POINT('Ctrl Pts',(-58.9211884788715,-116.907673738885,
179.954696079469));
#44096=CARTESIAN_POINT('Ctrl Pts',(-60.5659638699407,-116.826610922184,
180.159873561769));
#44097=CARTESIAN_POINT('Ctrl Pts',(-61.8761714145897,-116.781215273124,
179.142400961866));
#44098=CARTESIAN_POINT('Ctrl Pts',(-63.1863789592387,-116.735819624063,
178.124928361964));
#44099=CARTESIAN_POINT('Ctrl Pts',(-63.4003384298088,-116.807291343618,
176.48082732954));
#44100=CARTESIAN_POINT('Ctrl Pts',(-63.6142979003789,-116.878763063172,
174.836726297116));
#44101=CARTESIAN_POINT('Ctrl Pts',(-62.6124963232813,-117.079843032778,
173.529088919052));
#44102=CARTESIAN_POINT('Ctrl Pts',(-61.6106947461837,-117.280923002385,
172.221451540989));
#44103=CARTESIAN_POINT('Ctrl Pts',(-59.9857954809486,-117.548429348396,
172.016274058689));
#44104=CARTESIAN_POINT('Ctrl Pts',(-58.3608962157134,-117.815935694408,
171.81109657639));
#44105=CARTESIAN_POINT('Ctrl Pts',(-57.0705647968984,-118.047774872779,
172.828569176292));
#44106=CARTESIAN_POINT('Ctrl Pts',(-55.7802333780834,-118.27961405115,173.846041776195));
#44107=CARTESIAN_POINT('Ctrl Pts',(-55.5861500333474,-118.394585860907,
175.490142808619));
#44108=CARTESIAN_POINT('Ctrl Pts',(-55.3920666886113,-118.509557670663,
177.134243841043));
#44109=CARTESIAN_POINT('Ctrl Pts',(-56.4137443915429,-118.494921230367,
178.441881219107));
#44110=CARTESIAN_POINT('Ctrl Pts',(-57.4354220944745,-118.480284790072,
179.74951859717));
#44111=CARTESIAN_POINT('Ctrl Pts',(-59.0801974855437,-118.399221973371,
179.954696079469));
#44112=CARTESIAN_POINT('Ctrl Pts',(-60.7249728766129,-118.31815915667,180.159873561769));
#44113=CARTESIAN_POINT('Ctrl Pts',(-62.0351804212619,-118.272763507609,
179.142400961866));
#44114=CARTESIAN_POINT('Ctrl Pts',(-63.345387965911,-118.227367858549,178.124928361964));
#44115=CARTESIAN_POINT('Ctrl Pts',(-63.559347436481,-118.298839578103,176.48082732954));
#44116=CARTESIAN_POINT('Ctrl Pts',(-63.7733069070511,-118.370311297657,
174.836726297116));
#44117=CARTESIAN_POINT('Ctrl Pts',(-62.7715053299535,-118.571391267264,
173.529088919052));
#44118=CARTESIAN_POINT('Ctrl Pts',(-61.769703752856,-118.77247123687,172.221451540989));
#44119=CARTESIAN_POINT('Ctrl Pts',(-60.1448044876208,-119.039977582882,
172.016274058689));
#44120=CARTESIAN_POINT('Ctrl Pts',(-58.5199052223856,-119.307483928894,
171.81109657639));
#44121=CARTESIAN_POINT('Ctrl Pts',(-57.2295738035707,-119.539323107265,
172.828569176292));
#44122=CARTESIAN_POINT('Ctrl Pts',(-55.9392423847557,-119.771162285635,
173.846041776195));
#44123=CARTESIAN_POINT('Ctrl Pts',(-55.7451590400196,-119.886134095392,
175.490142808619));
#44124=CARTESIAN_POINT('Ctrl Pts',(-55.5510756952835,-120.001105905149,
177.134243841043));
#44125=CARTESIAN_POINT('Ctrl Pts',(-56.5727533982151,-119.986469464853,
178.441881219107));
#44126=CARTESIAN_POINT('Ctrl Pts',(-57.5944311011467,-119.971833024557,
179.74951859717));
#44127=CARTESIAN_POINT('Ctrl Pts',(-59.2392064922159,-119.890770207856,
179.954696079469));
#44128=CARTESIAN_POINT('Ctrl Pts',(-60.8839818832851,-119.809707391155,
180.159873561769));
#44129=CARTESIAN_POINT('Ctrl Pts',(-62.1941894279341,-119.764311742095,
179.142400961866));
#44130=CARTESIAN_POINT('Ctrl Pts',(-63.5043969725832,-119.718916093035,
178.124928361964));
#44131=CARTESIAN_POINT('Ctrl Pts',(-63.7183564431533,-119.790387812589,
176.48082732954));
#44132=CARTESIAN_POINT('Ctrl Pts',(-63.9323159137233,-119.861859532143,
174.836726297116));
#44133=CARTESIAN_POINT('Ctrl Pts',(-62.9305143366258,-120.062939501749,
173.529088919052));
#44134=CARTESIAN_POINT('Ctrl Pts',(-61.9287127595282,-120.264019471356,
172.221451540989));
#44135=CARTESIAN_POINT('Ctrl Pts',(-60.303813494293,-120.531525817368,172.016274058689));
#44136=CARTESIAN_POINT('Ctrl Pts',(-58.6789142290579,-120.799032163379,
171.81109657639));
#44137=CARTESIAN_POINT('Ctrl Pts',(-57.3885828102429,-121.03087134175,172.828569176292));
#44138=CARTESIAN_POINT('Ctrl Pts',(-56.0982513914279,-121.262710520121,
173.846041776195));
#44139=CARTESIAN_POINT('Ctrl Pts',(-55.9041680466918,-121.377682329878,
175.490142808619));
#44140=CARTESIAN_POINT('Ctrl Pts',(-55.7100847019558,-121.492654139634,
177.134243841043));
#44141=CARTESIAN_POINT('Ctrl Pts',(-56.7317624048874,-121.478017699339,
178.441881219107));
#44142=CARTESIAN_POINT('Ctrl Pts',(-57.753440107819,-121.463381259043,179.74951859717));
#44143=CARTESIAN_POINT('Ctrl Pts',(-59.3982154988882,-121.382318442342,
179.954696079469));
#44144=CARTESIAN_POINT('Ctrl Pts',(-61.0429908899573,-121.301255625641,
180.159873561769));
#44145=CARTESIAN_POINT('Ctrl Pts',(-62.3531984346064,-121.25585997658,179.142400961866));
#44146=CARTESIAN_POINT('Ctrl Pts',(-63.6634059792554,-121.21046432752,178.124928361964));
#44147=CARTESIAN_POINT('Ctrl Pts',(-63.8773654498255,-121.281936047074,
176.48082732954));
#44148=CARTESIAN_POINT('Ctrl Pts',(-64.0913249203956,-121.353407766628,
174.836726297116));
#44149=CARTESIAN_POINT('Ctrl Pts',(-63.089523343298,-121.554487736235,173.529088919052));
#44150=CARTESIAN_POINT('Ctrl Pts',(-62.0877217662004,-121.755567705841,
172.221451540989));
#44151=CARTESIAN_POINT('Ctrl Pts',(-60.4628225009653,-122.023074051853,
172.016274058689));
#44152=CARTESIAN_POINT('Ctrl Pts',(-58.8379232357301,-122.290580397865,
171.81109657639));
#44153=CARTESIAN_POINT('Ctrl Pts',(-57.5475918169151,-122.522419576236,
172.828569176292));
#44154=CARTESIAN_POINT('Ctrl Pts',(-56.2572603981001,-122.754258754607,
173.846041776195));
#44155=CARTESIAN_POINT('Ctrl Pts',(-56.0631770533641,-122.869230564363,
175.490142808619));
#44156=CARTESIAN_POINT('Ctrl Pts',(-55.869093708628,-122.98420237412,177.134243841043));
#44157=CARTESIAN_POINT('Ctrl Pts',(-56.8907714115596,-122.969565933824,
178.441881219107));
#44158=CARTESIAN_POINT('Ctrl Pts',(-57.9124491144912,-122.954929493528,
179.74951859717));
#44159=CARTESIAN_POINT('Ctrl Pts',(-59.5572245055604,-122.873866676827,
179.954696079469));
#44160=CARTESIAN_POINT('Ctrl Pts',(-61.2019998966296,-122.792803860126,
180.159873561769));
#44161=CARTESIAN_POINT('Ctrl Pts',(-62.5122074412786,-122.747408211066,
179.142400961866));
#44162=CARTESIAN_POINT('Ctrl Pts',(-63.8224149859276,-122.702012562006,
178.124928361964));
#44163=CARTESIAN_POINT('Ctrl Pts',(-64.0363744564977,-122.77348428156,176.48082732954));
#44164=CARTESIAN_POINT('Ctrl Pts',(-64.2503339270678,-122.844956001114,
174.836726297116));
#44165=CARTESIAN_POINT('Ctrl Pts',(-63.2485323499702,-123.046035970721,
173.529088919052));
#44166=CARTESIAN_POINT('Ctrl Pts',(-62.2467307728726,-123.247115940327,
172.221451540989));
#44167=CARTESIAN_POINT('Ctrl Pts',(-60.6218315076375,-123.514622286339,
172.016274058689));
#44168=CARTESIAN_POINT('Ctrl Pts',(-58.9969322424023,-123.78212863235,171.81109657639));
#44169=CARTESIAN_POINT('Ctrl Pts',(-57.7066008235873,-124.013967810721,
172.828569176292));
#44170=CARTESIAN_POINT('Ctrl Pts',(-56.4162694047723,-124.245806989092,
173.846041776195));
#44171=CARTESIAN_POINT('Ctrl Pts',(-56.2221860600363,-124.360778798849,
175.490142808619));
#44172=CARTESIAN_POINT('Ctrl Pts',(-56.0281027153002,-124.475750608606,
177.134243841043));
#44173=CARTESIAN_POINT('Ctrl Pts',(-57.0497804182318,-124.46111416831,178.441881219107));
#44174=CARTESIAN_POINT('Ctrl Pts',(-58.0714581211634,-124.446477728014,
179.74951859717));
#44175=CARTESIAN_POINT('Ctrl Pts',(-59.7162335122326,-124.365414911313,
179.954696079469));
#44176=CARTESIAN_POINT('Ctrl Pts',(-61.3610089033018,-124.284352094612,
180.159873561769));
#44177=CARTESIAN_POINT('Ctrl Pts',(-62.6712164479508,-124.238956445552,
179.142400961866));
#44178=CARTESIAN_POINT('Ctrl Pts',(-63.9814239925999,-124.193560796491,
178.124928361964));
#44179=CARTESIAN_POINT('Ctrl Pts',(-64.1953834631699,-124.265032516046,
176.48082732954));
#44180=CARTESIAN_POINT('Ctrl Pts',(-64.40934293374,-124.3365042356,174.836726297116));
#44181=CARTESIAN_POINT('Ctrl Pts',(-63.4075413566424,-124.537584205206,
173.529088919052));
#44182=CARTESIAN_POINT('Ctrl Pts',(-62.4057397795449,-124.738664174813,
172.221451540989));
#44183=CARTESIAN_POINT('Ctrl Pts',(-60.7808405143097,-125.006170520824,
172.016274058689));
#44184=CARTESIAN_POINT('Ctrl Pts',(-59.1559412490746,-125.273676866836,
171.81109657639));
#44185=CARTESIAN_POINT('Ctrl Pts',(-57.8656098302596,-125.505516045207,
172.828569176292));
#44186=CARTESIAN_POINT('Ctrl Pts',(-56.5752784114446,-125.737355223578,
173.846041776195));
#44187=CARTESIAN_POINT('Ctrl Pts',(-56.3811950667085,-125.852327033334,
175.490142808619));
#44188=CARTESIAN_POINT('Ctrl Pts',(-56.1871117219724,-125.967298843091,
177.134243841043));
#44189=CARTESIAN_POINT('Ctrl Pts',(-57.208789424904,-125.952662402795,178.441881219107));
#44190=CARTESIAN_POINT('Ctrl Pts',(-58.2304671278357,-125.9380259625,179.74951859717));
#44191=CARTESIAN_POINT('Ctrl Pts',(-59.8752425189048,-125.856963145799,
179.954696079469));
#44192=CARTESIAN_POINT('Ctrl Pts',(-61.520017909974,-125.775900329098,180.159873561769));
#44193=CARTESIAN_POINT('Ctrl Pts',(-62.8302254546231,-125.730504680037,
179.142400961866));
#44194=CARTESIAN_POINT('Ctrl Pts',(-64.1404329992721,-125.685109030977,
178.124928361964));
#44195=CARTESIAN_POINT('Ctrl Pts',(-64.3543924698422,-125.756580750531,
176.48082732954));
#44196=CARTESIAN_POINT('Ctrl Pts',(-64.5683519404122,-125.828052470085,
174.836726297116));
#44197=CARTESIAN_POINT('Ctrl Pts',(-63.5665503633147,-126.029132439692,
173.529088919052));
#44198=CARTESIAN_POINT('Ctrl Pts',(-62.5647487862171,-126.230212409298,
172.221451540989));
#44199=CARTESIAN_POINT('Ctrl Pts',(-60.9398495209819,-126.49771875531,172.016274058689));
#44200=CARTESIAN_POINT('Ctrl Pts',(-59.3149502557468,-126.765225101322,
171.81109657639));
#44201=CARTESIAN_POINT('Ctrl Pts',(-58.0246188369318,-126.997064279693,
172.828569176292));
#44202=CARTESIAN_POINT('Ctrl Pts',(-56.7342874181168,-127.228903458063,
173.846041776195));
#44203=CARTESIAN_POINT('Ctrl Pts',(-56.5402040733807,-127.34387526782,175.490142808619));
#44204=CARTESIAN_POINT('Ctrl Pts',(-56.3461207286447,-127.458847077577,
177.134243841043));
#44205=CARTESIAN_POINT('Ctrl Pts',(-57.3677984315763,-127.444210637281,
178.441881219107));
#44206=CARTESIAN_POINT('Ctrl Pts',(-58.3894761345079,-127.429574196985,
179.74951859717));
#44207=CARTESIAN_POINT('Ctrl Pts',(-60.0342515255771,-127.348511380284,
179.954696079469));
#44208=CARTESIAN_POINT('Ctrl Pts',(-61.6790269166463,-127.267448563583,
180.159873561769));
#44209=CARTESIAN_POINT('Ctrl Pts',(-62.9892344612953,-127.222052914523,
179.142400961866));
#44210=CARTESIAN_POINT('Ctrl Pts',(-64.2994420059443,-127.176657265463,
178.124928361964));
#44211=CARTESIAN_POINT('Ctrl Pts',(-64.5134014765144,-127.248128985017,
176.48082732954));
#44212=CARTESIAN_POINT('Ctrl Pts',(-64.7273609470845,-127.319600704571,
174.836726297116));
#44213=CARTESIAN_POINT('Ctrl Pts',(-63.7255593699869,-127.520680674177,
173.529088919052));
#44214=CARTESIAN_POINT('Ctrl Pts',(-62.7237577928893,-127.721760643784,
172.221451540989));
#44215=CARTESIAN_POINT('Ctrl Pts',(-61.0988585276542,-127.989266989795,
172.016274058689));
#44216=CARTESIAN_POINT('Ctrl Pts',(-59.473959262419,-128.256773335807,171.81109657639));
#44217=CARTESIAN_POINT('Ctrl Pts',(-58.183627843604,-128.488612514178,172.828569176292));
#44218=CARTESIAN_POINT('Ctrl Pts',(-56.893296424789,-128.720451692549,173.846041776195));
#44219=CARTESIAN_POINT('Ctrl Pts',(-56.699213080053,-128.835423502306,175.490142808619));
#44220=CARTESIAN_POINT('Ctrl Pts',(-56.5051297353169,-128.950395312062,
177.134243841043));
#44221=CARTESIAN_POINT('Ctrl Pts',(-57.5268074382485,-128.935758871767,
178.441881219107));
#44222=CARTESIAN_POINT('Ctrl Pts',(-58.5484851411801,-128.921122431471,
179.74951859717));
#44223=CARTESIAN_POINT('Ctrl Pts',(-60.1932605322493,-128.84005961477,179.954696079469));
#44224=CARTESIAN_POINT('Ctrl Pts',(-61.8380359233185,-128.758996798069,
180.159873561769));
#44225=CARTESIAN_POINT('Ctrl Pts',(-63.1482434679675,-128.713601149008,
179.142400961866));
#44226=CARTESIAN_POINT('Ctrl Pts',(-64.4584510126165,-128.668205499948,
178.124928361964));
#44227=CARTESIAN_POINT('Ctrl Pts',(-64.6724104831866,-128.739677219502,
176.48082732954));
#44228=CARTESIAN_POINT('Ctrl Pts',(-64.8863699537567,-128.811148939056,
174.836726297116));
#44229=CARTESIAN_POINT('Ctrl Pts',(-63.8845683766591,-129.012228908663,
173.529088919052));
#44230=CARTESIAN_POINT('Ctrl Pts',(-62.8827667995616,-129.213308878269,
172.221451540989));
#44231=CARTESIAN_POINT('Ctrl Pts',(-61.2578675343264,-129.480815224281,
172.016274058689));
#44232=CARTESIAN_POINT('Ctrl Pts',(-59.6329682690912,-129.748321570293,
171.81109657639));
#44233=CARTESIAN_POINT('Ctrl Pts',(-58.3426368502762,-129.980160748664,
172.828569176292));
#44234=CARTESIAN_POINT('Ctrl Pts',(-57.0523054314612,-130.211999927035,
173.846041776195));
#44235=CARTESIAN_POINT('Ctrl Pts',(-56.8582220867252,-130.326971736791,
175.490142808619));
#44236=CARTESIAN_POINT('Ctrl Pts',(-56.6641387419891,-130.441943546548,
177.134243841043));
#44237=CARTESIAN_POINT('Ctrl Pts',(-57.6858164449207,-130.427307106252,
178.441881219107));
#44238=CARTESIAN_POINT('Ctrl Pts',(-58.7074941478523,-130.412670665956,
179.74951859717));
#44239=CARTESIAN_POINT('Ctrl Pts',(-60.3522695389215,-130.331607849255,
179.954696079469));
#44240=CARTESIAN_POINT('Ctrl Pts',(-61.9970449299907,-130.250545032554,
180.159873561769));
#44241=CARTESIAN_POINT('Ctrl Pts',(-63.3072524746397,-130.205149383494,
179.142400961866));
#44242=CARTESIAN_POINT('Ctrl Pts',(-64.6174600192888,-130.159753734434,
178.124928361964));
#44243=CARTESIAN_POINT('Ctrl Pts',(-64.8314194898588,-130.231225453988,
176.48082732954));
#44244=CARTESIAN_POINT('Ctrl Pts',(-65.0453789604289,-130.302697173542,
174.836726297116));
#44245=CARTESIAN_POINT('Ctrl Pts',(-64.0435773833314,-130.503777143149,
173.529088919052));
#44246=CARTESIAN_POINT('Ctrl Pts',(-63.0417758062338,-130.704857112755,
172.221451540989));
#44247=CARTESIAN_POINT('Ctrl Pts',(-61.4168765409986,-130.972363458767,
172.016274058689));
#44248=CARTESIAN_POINT('Ctrl Pts',(-59.7919772757635,-131.239869804778,
171.81109657639));
#44249=CARTESIAN_POINT('Ctrl Pts',(-58.5016458569485,-131.471708983149,
172.828569176292));
#44250=CARTESIAN_POINT('Ctrl Pts',(-57.2113144381335,-131.70354816152,173.846041776195));
#44251=CARTESIAN_POINT('Ctrl Pts',(-57.0172310933974,-131.818519971277,
175.490142808619));
#44252=CARTESIAN_POINT('Ctrl Pts',(-56.8231477486614,-131.933491781033,
177.134243841043));
#44253=CARTESIAN_POINT('Ctrl Pts',(-57.844825451593,-131.918855340738,178.441881219107));
#44254=CARTESIAN_POINT('Ctrl Pts',(-58.8665031545246,-131.904218900442,
179.74951859717));
#44255=CARTESIAN_POINT('Ctrl Pts',(-60.5112785455938,-131.823156083741,
179.954696079469));
#44256=CARTESIAN_POINT('Ctrl Pts',(-61.5752382858275,-131.770718788127,
180.087419721831));
#44257=CARTESIAN_POINT('Ctrl Pts',(-62.5639783363627,-131.730760688539,
179.670610857428));
#44258=CARTESIAN_POINT('Origin',(-65.8133517206249,-123.652567188025,171.594677789993));
#44259=CARTESIAN_POINT('Origin',(-64.6054323897224,-123.781339458681,170.37181129294));
#44260=CARTESIAN_POINT('Origin',(-63.1416108368898,-123.937392615849,169.475191110882));
#44261=CARTESIAN_POINT('Origin',(-61.5069590500029,-124.111657417267,168.956925549718));
#44262=CARTESIAN_POINT('Origin',(-59.7964770491983,-124.294006226103,168.847134320046));
#44263=CARTESIAN_POINT('Origin',(-58.1095718310134,-124.473841592396,169.152198089058));
#44264=CARTESIAN_POINT('Origin',(-56.5442801950783,-124.640712138335,169.854387659362));
#44265=CARTESIAN_POINT('Origin',(-55.1915712016699,-124.784919954338,170.912894325486));
#44266=CARTESIAN_POINT('Origin',(-54.1300593805879,-124.898084206314,172.26620152751));
#44267=CARTESIAN_POINT('Origin',(-53.4214359404352,-124.973628199272,173.835659969925));
#44268=CARTESIAN_POINT('Origin',(-53.1068834998121,-125.007161590934,175.530058432807));
#44269=CARTESIAN_POINT('Origin',(-53.2046827032159,-124.996735542465,177.25092463638));
#44270=CARTESIAN_POINT('Origin',(-53.7091498164305,-124.942955977905,178.898248091987));
#44271=CARTESIAN_POINT('Origin',(-54.5909670444992,-124.848948370066,180.376292348166));
#44272=CARTESIAN_POINT('Origin',(-55.7988863754018,-124.72017609941,181.599158845219));
#44273=CARTESIAN_POINT('Origin',(-66.6951689486936,-123.558559580185,173.072722046172));
#44274=CARTESIAN_POINT('Origin',(-54.0803126256813,-66.8261507513496,175.985485069079));
#44275=CARTESIAN_POINT('',(0.,0.,0.));
#44276=CARTESIAN_POINT('Origin',(-53.8258982150057,-64.4396735761727,175.985485069079));
#44277=CARTESIAN_POINT('',(-53.4018741972131,-60.4622116175444,179.985485069079));
#44278=CARTESIAN_POINT('',(-51.6251552267953,-62.6629546057548,179.449586684217));
#44279=CARTESIAN_POINT('Ctrl Pts',(-53.4018741972131,-60.4622116175444,
179.985485069079));
#44280=CARTESIAN_POINT('Ctrl Pts',(-53.6563428684955,-60.4350835571074,
179.985485069079));
#44281=CARTESIAN_POINT('Ctrl Pts',(-53.9303211793164,-60.458242890839,179.958669005781));
#44282=CARTESIAN_POINT('Ctrl Pts',(-54.4409372535361,-60.6105704641806,
179.862014751158));
#44283=CARTESIAN_POINT('Ctrl Pts',(-54.6778490486358,-60.7394791031505,
179.79321828922));
#44284=CARTESIAN_POINT('Ctrl Pts',(-55.0631092638411,-61.0505100306915,
179.660886004177));
#44285=CARTESIAN_POINT('Ctrl Pts',(-55.2387001635013,-61.2547981540133,
179.587877094001));
#44286=CARTESIAN_POINT('Ctrl Pts',(-55.4948940947938,-61.7211552694728,
179.481135940985));
#44287=CARTESIAN_POINT('Ctrl Pts',(-55.5754149704257,-61.9837663264949,
179.449586684217));
#44288=CARTESIAN_POINT('Ctrl Pts',(-55.6026171854236,-62.2389305879622,
179.449586684217));
#44289=CARTESIAN_POINT('Ctrl Pts',(-55.6298194004214,-62.4940948494295,
179.449586684217));
#44290=CARTESIAN_POINT('Ctrl Pts',(-55.6064711817378,-62.7677790458441,
179.481135940985));
#44291=CARTESIAN_POINT('Ctrl Pts',(-55.4543512989582,-63.2776651417851,
179.587877094001));
#44292=CARTESIAN_POINT('Ctrl Pts',(-55.3257742211671,-63.5143796036173,
179.660886004177));
#44293=CARTESIAN_POINT('Ctrl Pts',(-55.0147432936261,-63.8996398188226,
179.79321828922));
#44294=CARTESIAN_POINT('Ctrl Pts',(-54.8103321708864,-64.0755964292659,
179.862014751158));
#44295=CARTESIAN_POINT('Ctrl Pts',(-54.343305267868,-64.3321472755105,179.958669005781));
#44296=CARTESIAN_POINT('Ctrl Pts',(-54.080366886288,-64.4125455157357,179.985485069079));
#44297=CARTESIAN_POINT('Ctrl Pts',(-53.5714295437234,-64.4668016366096,
179.985485069079));
#44298=CARTESIAN_POINT('Ctrl Pts',(-53.2974512329025,-64.443642302878,179.958669005781));
#44299=CARTESIAN_POINT('Ctrl Pts',(-52.7868351586827,-64.2913147295365,
179.862014751158));
#44300=CARTESIAN_POINT('Ctrl Pts',(-52.549923363583,-64.1624060905666,179.79321828922));
#44301=CARTESIAN_POINT('Ctrl Pts',(-52.1646631483778,-63.8513751630256,
179.660886004177));
#44302=CARTESIAN_POINT('Ctrl Pts',(-51.9890722487176,-63.6470870397037,
179.587877094001));
#44303=CARTESIAN_POINT('Ctrl Pts',(-51.732878317425,-63.1807299242443,179.481135940985));
#44304=CARTESIAN_POINT('Ctrl Pts',(-51.6523574417932,-62.9181188672221,
179.449586684217));
#44305=CARTESIAN_POINT('Ctrl Pts',(-51.6251552267953,-62.6629546057548,
179.449586684217));
#44306=CARTESIAN_POINT('Ctrl Pts',(-51.6251552267953,-62.6629546057548,
179.449586684217));
#44307=CARTESIAN_POINT('Ctrl Pts',(-51.5979530117974,-62.4077903442875,
179.449586684217));
#44308=CARTESIAN_POINT('Ctrl Pts',(-51.6213012304811,-62.1341061478729,
179.481135940985));
#44309=CARTESIAN_POINT('Ctrl Pts',(-51.7734211132606,-61.6242200519319,
179.587877094001));
#44310=CARTESIAN_POINT('Ctrl Pts',(-51.9019981910518,-61.3875055900997,
179.660886004177));
#44311=CARTESIAN_POINT('Ctrl Pts',(-52.2130291185928,-61.0022453748944,
179.79321828922));
#44312=CARTESIAN_POINT('Ctrl Pts',(-52.4174402413325,-60.8262887644511,
179.862014751158));
#44313=CARTESIAN_POINT('Ctrl Pts',(-52.8844671443509,-60.5697379182066,
179.958669005781));
#44314=CARTESIAN_POINT('Ctrl Pts',(-53.1474055259308,-60.4893396779814,
179.985485069079));
#44315=CARTESIAN_POINT('Ctrl Pts',(-53.4018741972131,-60.4622116175444,
179.985485069079));
#44316=CARTESIAN_POINT('Origin',(-53.6138862061094,-62.4509425968585,185.985485069079));
#44317=CARTESIAN_POINT('',(-51.6251552267953,-62.6629546057548,172.521383453942));
#44318=CARTESIAN_POINT('Ctrl Pts',(-55.6026171854236,-62.2389305879622,
172.521383453942));
#44319=CARTESIAN_POINT('Ctrl Pts',(-55.5754149704257,-61.9837663264949,
172.521383453942));
#44320=CARTESIAN_POINT('Ctrl Pts',(-55.4948940947938,-61.7211552694728,
172.489834197174));
#44321=CARTESIAN_POINT('Ctrl Pts',(-55.2387001635013,-61.2547981540133,
172.383093044158));
#44322=CARTESIAN_POINT('Ctrl Pts',(-55.0631092638411,-61.0505100306915,
172.310084133982));
#44323=CARTESIAN_POINT('Ctrl Pts',(-54.6778490486358,-60.7394791031505,
172.177751848938));
#44324=CARTESIAN_POINT('Ctrl Pts',(-54.4409372535361,-60.6105704641806,
172.108955387));
#44325=CARTESIAN_POINT('Ctrl Pts',(-53.9303211793164,-60.458242890839,172.012301132378));
#44326=CARTESIAN_POINT('Ctrl Pts',(-53.6563428684955,-60.4350835571074,
171.985485069079));
#44327=CARTESIAN_POINT('Ctrl Pts',(-53.1474055259308,-60.4893396779814,
171.985485069079));
#44328=CARTESIAN_POINT('Ctrl Pts',(-52.8844671443509,-60.5697379182066,
172.012301132378));
#44329=CARTESIAN_POINT('Ctrl Pts',(-52.4174402413325,-60.8262887644511,
172.108955387));
#44330=CARTESIAN_POINT('Ctrl Pts',(-52.2130291185928,-61.0022453748944,
172.177751848938));
#44331=CARTESIAN_POINT('Ctrl Pts',(-51.9019981910518,-61.3875055900997,
172.310084133982));
#44332=CARTESIAN_POINT('Ctrl Pts',(-51.7734211132606,-61.6242200519319,
172.383093044158));
#44333=CARTESIAN_POINT('Ctrl Pts',(-51.6213012304811,-62.1341061478729,
172.489834197174));
#44334=CARTESIAN_POINT('Ctrl Pts',(-51.5979530117974,-62.4077903442875,
172.521383453942));
#44335=CARTESIAN_POINT('Ctrl Pts',(-51.6523574417932,-62.9181188672221,
172.521383453942));
#44336=CARTESIAN_POINT('Ctrl Pts',(-51.732878317425,-63.1807299242443,172.489834197174));
#44337=CARTESIAN_POINT('Ctrl Pts',(-51.9890722487176,-63.6470870397037,
172.383093044158));
#44338=CARTESIAN_POINT('Ctrl Pts',(-52.1646631483778,-63.8513751630256,
172.310084133982));
#44339=CARTESIAN_POINT('Ctrl Pts',(-52.549923363583,-64.1624060905665,172.177751848938));
#44340=CARTESIAN_POINT('Ctrl Pts',(-52.7868351586827,-64.2913147295365,
172.108955387));
#44341=CARTESIAN_POINT('Ctrl Pts',(-53.2974512329024,-64.443642302878,172.012301132378));
#44342=CARTESIAN_POINT('Ctrl Pts',(-53.5714295437234,-64.4668016366096,
171.985485069079));
#44343=CARTESIAN_POINT('Ctrl Pts',(-54.080366886288,-64.4125455157357,171.985485069079));
#44344=CARTESIAN_POINT('Ctrl Pts',(-54.343305267868,-64.3321472755105,172.012301132378));
#44345=CARTESIAN_POINT('Ctrl Pts',(-54.8103321708864,-64.0755964292659,
172.108955387));
#44346=CARTESIAN_POINT('Ctrl Pts',(-55.0147432936261,-63.8996398188226,
172.177751848938));
#44347=CARTESIAN_POINT('Ctrl Pts',(-55.3257742211671,-63.5143796036173,
172.310084133982));
#44348=CARTESIAN_POINT('Ctrl Pts',(-55.4543512989582,-63.2776651417851,
172.383093044158));
#44349=CARTESIAN_POINT('Ctrl Pts',(-55.6064711817378,-62.7677790458441,
172.489834197174));
#44350=CARTESIAN_POINT('Ctrl Pts',(-55.6298194004214,-62.4940948494295,
172.521383453942));
#44351=CARTESIAN_POINT('Ctrl Pts',(-55.6026171854236,-62.2389305879622,
172.521383453942));
#44352=CARTESIAN_POINT('',(-51.6251552267953,-62.6629546057548,185.985485069079));
#44353=CARTESIAN_POINT('Origin',(-53.8258982150057,-64.4396735761727,175.985485069079));
#44354=CARTESIAN_POINT('',(0.,0.,0.));
#44355=CARTESIAN_POINT('Origin',(-69.9391102914966,14.1820463536532,177.985485069079));
#44356=CARTESIAN_POINT('',(-73.3730842378033,18.9797356866641,178.485485069079));
#44357=CARTESIAN_POINT('',(-67.58190263219,8.77338921431569,178.485485069079));
#44358=CARTESIAN_POINT('Origin',(-69.9391102914966,14.1820463536532,178.485485069079));
#44359=CARTESIAN_POINT('',(-73.6640989790157,19.3863195284447,177.985485069079));
#44360=CARTESIAN_POINT('Origin',(-73.3730842378033,18.9797356866641,177.985485069079));
#44361=CARTESIAN_POINT('',(-67.3821392712318,8.31502843979556,177.985485069079));
#44362=CARTESIAN_POINT('Origin',(-69.9391102914966,14.1820463536532,177.985485069079));
#44363=CARTESIAN_POINT('Origin',(-67.58190263219,8.77338921431569,177.985485069079));
#44364=CARTESIAN_POINT('Origin',(-69.9391102914966,14.1820463536532,173.985485069079));
#44365=CARTESIAN_POINT('',(-73.6640989790157,19.3863195284447,173.985485069079));
#44366=CARTESIAN_POINT('',(-67.3821392712318,8.31502843979556,173.985485069079));
#44367=CARTESIAN_POINT('Origin',(-69.9391102914966,14.1820463536532,173.985485069079));
#44368=CARTESIAN_POINT('',(-73.3730842378033,18.9797356866641,173.485485069079));
#44369=CARTESIAN_POINT('Origin',(-73.3730842378033,18.9797356866641,173.985485069079));
#44370=CARTESIAN_POINT('',(-67.58190263219,8.77338921431569,173.485485069079));
#44371=CARTESIAN_POINT('Origin',(-69.9391102914966,14.1820463536532,173.485485069079));
#44372=CARTESIAN_POINT('Origin',(-67.58190263219,8.77338921431569,173.985485069079));
#44373=CARTESIAN_POINT('Origin',(-55.2165279528263,6.30034797823479,177.185485069079));
#44374=CARTESIAN_POINT('',(-53.7305455470457,6.09575988055917,177.185485069079));
#44375=CARTESIAN_POINT('Origin',(-55.2165279528263,6.30034797823479,177.185485069079));
#44376=CARTESIAN_POINT('',(-53.7305455470457,6.09575988055917,174.785485069079));
#44377=CARTESIAN_POINT('',(-53.7305455470457,6.09575988055917,177.185485069079));
#44378=CARTESIAN_POINT('Origin',(-55.2165279528263,6.30034797823479,174.785485069079));
#44379=CARTESIAN_POINT('Origin',(-69.9391102914966,14.1820463536532,171.985485069079));
#44380=CARTESIAN_POINT('',(-71.9204201658707,14.4548304838874,173.485485069079));
#44381=CARTESIAN_POINT('Origin',(-69.9391102914966,14.1820463536532,173.485485069079));
#44382=CARTESIAN_POINT('',(-71.9204201658707,14.4548304838874,178.485485069079));
#44383=CARTESIAN_POINT('',(-71.9204201658707,14.4548304838874,171.985485069079));
#44384=CARTESIAN_POINT('Origin',(-69.9391102914966,14.1820463536532,178.485485069079));
#44385=CARTESIAN_POINT('Origin',(-38.9776940652673,8.40516957928931,171.985485069079));
#44386=CARTESIAN_POINT('',(-40.9590039396414,8.67795370952346,173.485485069079));
#44387=CARTESIAN_POINT('Origin',(-38.9776940652673,8.40516957928931,173.485485069079));
#44388=CARTESIAN_POINT('',(-40.9590039396414,8.67795370952346,178.485485069079));
#44389=CARTESIAN_POINT('',(-40.9590039396414,8.67795370952346,171.985485069079));
#44390=CARTESIAN_POINT('Origin',(-38.9776940652673,8.40516957928931,178.485485069079));
#44391=CARTESIAN_POINT('Origin',(-36.5934363437889,54.2142642791517,172.485485069079));
#44392=CARTESIAN_POINT('',(-50.6604618554941,55.4734714302896,172.985485069079));
#44393=CARTESIAN_POINT('',(-49.7994785223376,59.2209856988867,172.985485069079));
#44394=CARTESIAN_POINT('Origin',(-36.5934363437889,54.2142642791517,172.985485069079));
#44395=CARTESIAN_POINT('',(-51.5230382845183,55.5506847976022,173.485485069079));
#44396=CARTESIAN_POINT('Origin',(-51.5230382845184,55.5506847976013,172.485485069079));
#44397=CARTESIAN_POINT('',(-51.2438457370578,57.3835762739523,173.485485069079));
#44398=CARTESIAN_POINT('Origin',(-36.5934363437889,54.2142642791517,173.485485069079));
#44399=CARTESIAN_POINT('Ctrl Pts',(-51.2438457370578,57.3835762739523,173.485485069079));
#44400=CARTESIAN_POINT('Ctrl Pts',(-51.1924620128878,57.4555875576865,173.485485069079));
#44401=CARTESIAN_POINT('Ctrl Pts',(-51.1407466430462,57.5273107046625,173.48365231973));
#44402=CARTESIAN_POINT('Ctrl Pts',(-51.088733797749,57.5986654010425,173.480047403934));
#44403=CARTESIAN_POINT('Ctrl Pts',(-51.0368178468029,57.6698871712776,173.476449203709));
#44404=CARTESIAN_POINT('Ctrl Pts',(-50.9846044885947,57.7407416201286,173.471085313099));
#44405=CARTESIAN_POINT('Ctrl Pts',(-50.9321306284918,57.8111529948007,173.463964962461));
#44406=CARTESIAN_POINT('Ctrl Pts',(-50.8803221459752,57.8806715411113,173.456934899095));
#44407=CARTESIAN_POINT('Ctrl Pts',(-50.8282588216532,57.9497578739147,173.448192322867));
#44408=CARTESIAN_POINT('Ctrl Pts',(-50.7759933930428,58.0183471515507,173.437699729118));
#44409=CARTESIAN_POINT('Ctrl Pts',(-50.7252918589377,58.0848840898626,173.427521096436));
#44410=CARTESIAN_POINT('Ctrl Pts',(-50.6743994664868,58.1509529687663,173.41569511002));
#44411=CARTESIAN_POINT('Ctrl Pts',(-50.6233919622077,58.2165066509814,173.402149742799));
#44412=CARTESIAN_POINT('Ctrl Pts',(-50.5902712724658,58.2590726067317,173.393354332956));
#44413=CARTESIAN_POINT('Ctrl Pts',(-50.5571026313059,58.3014215878905,173.383833224202));
#44414=CARTESIAN_POINT('Ctrl Pts',(-50.5239152725159,58.3435445498383,173.373559351834));
#44415=CARTESIAN_POINT('Ctrl Pts',(-50.4846204001192,58.3934194562805,173.361394765124));
#44416=CARTESIAN_POINT('Ctrl Pts',(-50.4452379534982,58.4430651051017,173.348160519015));
#44417=CARTESIAN_POINT('Ctrl Pts',(-50.4057859651512,58.4923925183112,173.333744171839));
#44418=CARTESIAN_POINT('Ctrl Pts',(-50.3671961550944,58.5406419370631,173.319642877519));
#44419=CARTESIAN_POINT('Ctrl Pts',(-50.3285393960941,58.5885865961815,173.304410206274));
#44420=CARTESIAN_POINT('Ctrl Pts',(-50.2898712506386,58.6361573428422,173.287913558918));
#44421=CARTESIAN_POINT('Ctrl Pts',(-50.2524971554251,58.6821361089333,173.271968980721));
#44422=CARTESIAN_POINT('Ctrl Pts',(-50.2151121387377,58.7277653266149,173.254843160663));
#44423=CARTESIAN_POINT('Ctrl Pts',(-50.1778078229766,58.7729996473115,173.23639656982));
#44424=CARTESIAN_POINT('Ctrl Pts',(-50.1707542187054,58.7815526790764,173.232908636875));
#44425=CARTESIAN_POINT('Ctrl Pts',(-50.1637036296667,58.7900916492096,173.229373436177));
#44426=CARTESIAN_POINT('Ctrl Pts',(-50.1566568626439,58.7986163344981,173.225789962875));
#44427=CARTESIAN_POINT('Ctrl Pts',(-50.1292096274332,58.8318200776407,173.211832294876));
#44428=CARTESIAN_POINT('Ctrl Pts',(-50.1019214691877,58.8647828422331,173.197227737558));
#44429=CARTESIAN_POINT('Ctrl Pts',(-50.0747632184024,58.8974130720074,173.181821868794));
#44430=CARTESIAN_POINT('Ctrl Pts',(-50.0486290122832,58.9288129275201,173.166996902603));
#44431=CARTESIAN_POINT('Ctrl Pts',(-50.0226148881682,58.9599046602197,173.15142954025));
#44432=CARTESIAN_POINT('Ctrl Pts',(-49.9967338141118,58.990619871463,173.134958085307));
#44433=CARTESIAN_POINT('Ctrl Pts',(-49.9715189975838,59.0205443797903,173.11891065569));
#44434=CARTESIAN_POINT('Ctrl Pts',(-49.9464301568035,59.0501112772456,173.10200475355));
#44435=CARTESIAN_POINT('Ctrl Pts',(-49.9215209152558,59.0792731406212,173.084072502622));
#44436=CARTESIAN_POINT('Ctrl Pts',(-49.8976983277173,59.10716283135,173.066922537752));
#44437=CARTESIAN_POINT('Ctrl Pts',(-49.8740398428972,59.1346818980189,173.0488334264));
#44438=CARTESIAN_POINT('Ctrl Pts',(-49.8506341911061,59.1618061936532,173.029646546259));
#44439=CARTESIAN_POINT('Ctrl Pts',(-49.8334276260605,59.1817465038532,173.015541393191));
#44440=CARTESIAN_POINT('Ctrl Pts',(-49.8163585066683,59.2014737900901,173.000842678105));
#44441=CARTESIAN_POINT('Ctrl Pts',(-49.7994785223376,59.2209856988867,172.985485069079));
#44442=CARTESIAN_POINT('Origin',(-36.5934363437889,54.2142642791517,179.485485069079));
#44443=CARTESIAN_POINT('',(-51.5230382845183,55.5506847976022,178.485485069079));
#44444=CARTESIAN_POINT('',(-51.2438457370575,57.3835762739533,178.485485069079));
#44445=CARTESIAN_POINT('Origin',(-36.5934363437889,54.2142642791517,178.485485069079));
#44446=CARTESIAN_POINT('',(-50.6604618554941,55.4734714302896,178.985485069079));
#44447=CARTESIAN_POINT('Origin',(-51.5230382845183,55.5506847976022,179.485485069079));
#44448=CARTESIAN_POINT('',(-49.7994785223364,59.2209856988899,178.985485069079));
#44449=CARTESIAN_POINT('Origin',(-36.5934363437889,54.2142642791517,178.985485069079));
#44450=CARTESIAN_POINT('Ctrl Pts',(-49.7994785223364,59.2209856988899,178.985485069079));
#44451=CARTESIAN_POINT('Ctrl Pts',(-49.9141823963008,59.0883972151807,178.881126130375));
#44452=CARTESIAN_POINT('Ctrl Pts',(-50.034723824992,58.9461165755505,178.807211858702));
#44453=CARTESIAN_POINT('Ctrl Pts',(-50.2779781597796,58.6518561196932,178.683459642416));
#44454=CARTESIAN_POINT('Ctrl Pts',(-50.4016974430789,58.4986739453797,178.635233133972));
#44455=CARTESIAN_POINT('Ctrl Pts',(-50.7690434736068,58.0324067380221,178.521551735829));
#44456=CARTESIAN_POINT('Ctrl Pts',(-51.0091426506735,57.7124989205671,178.485485069079));
#44457=CARTESIAN_POINT('Ctrl Pts',(-51.2438457370575,57.3835762739533,178.485485069079));
#44458=CARTESIAN_POINT('Origin',(54.4964231308939,46.060372587574,178.485485069079));
#44459=CARTESIAN_POINT('',(-44.6376627105729,59.1917481581946,179.985485069079));
#44460=CARTESIAN_POINT('',(-44.3552179209134,61.1717279657211,179.985485069079));
#44461=CARTESIAN_POINT('Origin',(54.4964231308939,46.060372587574,179.985485069079));
#44462=CARTESIAN_POINT('',(-44.6376627105729,59.1917481581946,171.985485069079));
#44463=CARTESIAN_POINT('',(-44.6376627105729,59.1917481581946,178.485485069079));
#44464=CARTESIAN_POINT('',(-44.3552179209134,61.1717279657211,171.985485069079));
#44465=CARTESIAN_POINT('Origin',(54.4964231308939,46.060372587574,171.985485069079));
#44466=CARTESIAN_POINT('',(-44.3552179209134,61.1717279657211,178.485485069079));
#44467=CARTESIAN_POINT('Origin',(-69.9391102914966,14.1820463536532,178.485485069079));
#44468=CARTESIAN_POINT('',(-73.6640989790157,19.3863195284447,178.485485069079));
#44469=CARTESIAN_POINT('',(-67.3821392712318,8.31502843979556,178.485485069079));
#44470=CARTESIAN_POINT('Origin',(54.4964231308939,46.060372587574,178.485485069079));
#44471=CARTESIAN_POINT('',(-45.4928245268247,44.5939644440383,171.985485069079));
#44472=CARTESIAN_POINT('',(-45.4934286935833,44.6357561061623,171.985485069079));
#44473=CARTESIAN_POINT('Origin',(54.4964231308939,46.060372587574,171.985485069079));
#44474=CARTESIAN_POINT('',(-45.4934286935833,44.6357561061623,179.985485069079));
#44475=CARTESIAN_POINT('',(-45.4934286935833,44.6357561061623,178.485485069079));
#44476=CARTESIAN_POINT('',(-45.4928245268247,44.5939644440384,179.985485069079));
#44477=CARTESIAN_POINT('Origin',(54.4964231308939,46.060372587574,179.985485069079));
#44478=CARTESIAN_POINT('',(-45.4928245268247,44.5939644440383,178.485485069079));
#44479=CARTESIAN_POINT('Origin',(54.4964231308939,46.060372587574,178.485485069079));
#44480=CARTESIAN_POINT('',(-45.0253923549998,36.292658300611,179.985485069079));
#44481=CARTESIAN_POINT('',(-45.451589062978,42.836266743522,179.985485069079));
#44482=CARTESIAN_POINT('Origin',(54.4964231308939,46.060372587574,179.985485069079));
#44483=CARTESIAN_POINT('',(-44.9520576904499,35.5723002038223,178.735485069079));
#44484=CARTESIAN_POINT('Origin',(330.563412065017,138.023170518389,142.559792216127));
#44485=CARTESIAN_POINT('',(-44.8071649770098,34.2791422233116,177.985485069079));
#44486=CARTESIAN_POINT('Ctrl Pts',(-44.9520576904499,35.5723002038223,178.735485069079));
#44487=CARTESIAN_POINT('Ctrl Pts',(-44.9499126757554,35.5519610561786,178.70015248117));
#44488=CARTESIAN_POINT('Ctrl Pts',(-44.9476202963097,35.5302873872292,178.665928645697));
#44489=CARTESIAN_POINT('Ctrl Pts',(-44.9451866758168,35.5073596552394,178.632760823269));
#44490=CARTESIAN_POINT('Ctrl Pts',(-44.9426873271152,35.4838126817709,178.598697190849));
#44491=CARTESIAN_POINT('Ctrl Pts',(-44.9400389751137,35.4589425734026,178.565746780528));
#44492=CARTESIAN_POINT('Ctrl Pts',(-44.9372429317707,35.4327874712696,178.533876632703));
#44493=CARTESIAN_POINT('Ctrl Pts',(-44.9353113405311,35.4147187362919,178.511859771449));
#44494=CARTESIAN_POINT('Ctrl Pts',(-44.9333091525668,35.3960357141058,178.490358963154));
#44495=CARTESIAN_POINT('Ctrl Pts',(-44.9312354927774,35.3767394852785,178.469372146658));
#44496=CARTESIAN_POINT('Ctrl Pts',(-44.9298545854397,35.3638895934528,178.455396445803));
#44497=CARTESIAN_POINT('Ctrl Pts',(-44.9284419618016,35.3507675824538,178.44164883223));
#44498=CARTESIAN_POINT('Ctrl Pts',(-44.9269971286527,35.3373718075001,178.428130798924));
#44499=CARTESIAN_POINT('Ctrl Pts',(-44.9253730263247,35.3223139378043,178.412935501545));
#44500=CARTESIAN_POINT('Ctrl Pts',(-44.9237088282253,35.3069157690946,178.398036553842));
#44501=CARTESIAN_POINT('Ctrl Pts',(-44.9220065207789,35.2911999094899,178.383460539299));
#44502=CARTESIAN_POINT('Ctrl Pts',(-44.918400844352,35.2579119716227,178.352586919996));
#44503=CARTESIAN_POINT('Ctrl Pts',(-44.9146235494019,35.2231928856741,178.323158754952));
#44504=CARTESIAN_POINT('Ctrl Pts',(-44.9106921304939,35.1872437159977,178.295385385406));
#44505=CARTESIAN_POINT('Ctrl Pts',(-44.9063770122815,35.1477859730238,178.264901385722));
#44506=CARTESIAN_POINT('Ctrl Pts',(-44.9018762872234,35.1068472166844,178.236413498132));
#44507=CARTESIAN_POINT('Ctrl Pts',(-44.8972185382424,35.0647396054761,178.210178749903));
#44508=CARTESIAN_POINT('Ctrl Pts',(-44.8957587852626,35.0515429494971,178.201956698423));
#44509=CARTESIAN_POINT('Ctrl Pts',(-44.8942836344116,35.0382316780069,178.193955623614));
#44510=CARTESIAN_POINT('Ctrl Pts',(-44.8927940303359,35.0248158702409,178.18618248533));
#44511=CARTESIAN_POINT('Ctrl Pts',(-44.8927687237777,35.0245879520142,178.186050429182));
#44512=CARTESIAN_POINT('Ctrl Pts',(-44.8927434126584,35.0243600001049,178.185918436739));
#44513=CARTESIAN_POINT('Ctrl Pts',(-44.8927180969803,35.0241320145436,178.18578650803));
#44514=CARTESIAN_POINT('Ctrl Pts',(-44.8821478779092,34.9289397260715,178.130701459469));
#44515=CARTESIAN_POINT('Ctrl Pts',(-44.8705984589575,34.8262343682704,178.085693995916));
#44516=CARTESIAN_POINT('Ctrl Pts',(-44.8585873663329,34.7209813356256,178.052814110577));
#44517=CARTESIAN_POINT('Ctrl Pts',(-44.8564349967444,34.702120151748,178.046922084973));
#44518=CARTESIAN_POINT('Ctrl Pts',(-44.8542678150691,34.6831772657595,178.04141942219));
#44519=CARTESIAN_POINT('Ctrl Pts',(-44.8520888140828,34.6641813681723,178.036317803549));
#44520=CARTESIAN_POINT('Ctrl Pts',(-44.8520700304822,34.6640176181987,178.036273826163));
#44521=CARTESIAN_POINT('Ctrl Pts',(-44.8520512460038,34.66385386429,178.036229878571));
#44522=CARTESIAN_POINT('Ctrl Pts',(-44.8520324606494,34.6636901064642,178.036185960779));
#44523=CARTESIAN_POINT('Ctrl Pts',(-44.8376820744672,34.5385932893174,178.002636566354));
#44524=CARTESIAN_POINT('Ctrl Pts',(-44.8227435745058,34.4104536891947,177.985485079909));
#44525=CARTESIAN_POINT('Ctrl Pts',(-44.8071649770098,34.2791422233116,177.985485069079));
#44526=CARTESIAN_POINT('',(-42.790908491833,22.9265206443813,177.985485069079));
#44527=CARTESIAN_POINT('Origin',(54.4964231308939,46.060372587574,177.985485069079));
#44528=CARTESIAN_POINT('',(-42.790908491833,22.9265206443813,173.985485069079));
#44529=CARTESIAN_POINT('',(-42.790908491833,22.9265206443813,178.485485069079));
#44530=CARTESIAN_POINT('',(-44.8071649770098,34.2791422233116,173.985485069079));
#44531=CARTESIAN_POINT('Origin',(54.4964231308939,46.060372587574,173.985485069079));
#44532=CARTESIAN_POINT('',(-44.9520576904499,35.5723002038223,173.235485069079));
#44533=CARTESIAN_POINT('Ctrl Pts',(-44.8071649770098,34.2791422233116,173.985485069079));
#44534=CARTESIAN_POINT('Ctrl Pts',(-44.8119869746675,34.3197866767732,173.985485066031));
#44535=CARTESIAN_POINT('Ctrl Pts',(-44.8167478717134,34.3601484678123,173.98376136592));
#44536=CARTESIAN_POINT('Ctrl Pts',(-44.8214510473818,34.4002312816899,173.980411411577));
#44537=CARTESIAN_POINT('Ctrl Pts',(-44.8262327788271,34.4409835871633,173.977005503919));
#44538=CARTESIAN_POINT('Ctrl Pts',(-44.8309549221569,34.4814482509048,173.971918425354));
#44539=CARTESIAN_POINT('Ctrl Pts',(-44.8356207182126,34.5216340913495,173.96519866512));
#44540=CARTESIAN_POINT('Ctrl Pts',(-44.840324783733,34.5621495412727,173.958423788541));
#44541=CARTESIAN_POINT('Ctrl Pts',(-44.8449716560963,34.6023823536389,173.949989180473));
#44542=CARTESIAN_POINT('Ctrl Pts',(-44.8495631331995,34.6423350907661,173.939892529448));
#44543=CARTESIAN_POINT('Ctrl Pts',(-44.8504282877738,34.6498632331274,173.937990055881));
#44544=CARTESIAN_POINT('Ctrl Pts',(-44.8512914691809,34.6573813936389,173.936028428795));
#44545=CARTESIAN_POINT('Ctrl Pts',(-44.8521526796834,34.6648895283819,173.934007434543));
#44546=CARTESIAN_POINT('Ctrl Pts',(-44.8577166639521,34.7133969995249,173.920950487154));
#44547=CARTESIAN_POINT('Ctrl Pts',(-44.863192299931,34.7614335526644,173.905424660321));
#44548=CARTESIAN_POINT('Ctrl Pts',(-44.868534832102,34.8085874640509,173.887514455428));
#44549=CARTESIAN_POINT('Ctrl Pts',(-44.873830087861,34.8553241074322,173.869762739094));
#44550=CARTESIAN_POINT('Ctrl Pts',(-44.878994490974,34.9011927505699,173.849668972682));
#44551=CARTESIAN_POINT('Ctrl Pts',(-44.8839868989568,34.9458079142411,173.827363567394));
#44552=CARTESIAN_POINT('Ctrl Pts',(-44.8869886981608,34.9726337993163,173.813951933556));
#44553=CARTESIAN_POINT('Ctrl Pts',(-44.8899283696412,34.9990068755471,173.799741635272));
#44554=CARTESIAN_POINT('Ctrl Pts',(-44.8927976120671,35.0248481275786,173.784768767412));
#44555=CARTESIAN_POINT('Ctrl Pts',(-44.8928230557535,35.0250772809982,173.784635991962));
#44556=CARTESIAN_POINT('Ctrl Pts',(-44.8928484950895,35.0253064026888,173.784503151269));
#44557=CARTESIAN_POINT('Ctrl Pts',(-44.8928739300679,35.0255354925777,173.784370245394));
#44558=CARTESIAN_POINT('Ctrl Pts',(-44.9042559455637,35.1280519808853,173.724895584076));
#44559=CARTESIAN_POINT('Ctrl Pts',(-44.9148445610927,35.2249133976643,173.651948159166));
#44560=CARTESIAN_POINT('Ctrl Pts',(-44.9241349512787,35.3108325653701,173.569559139244));
#44561=CARTESIAN_POINT('Ctrl Pts',(-44.9250117892063,35.3189417172401,173.561783166864));
#44562=CARTESIAN_POINT('Ctrl Pts',(-44.925877066944,35.3269534368476,173.55392308958));
#44563=CARTESIAN_POINT('Ctrl Pts',(-44.9267303628307,35.3348633053383,173.545982294554));
#44564=CARTESIAN_POINT('Ctrl Pts',(-44.9267467660432,35.3350153595733,173.545829645807));
#44565=CARTESIAN_POINT('Ctrl Pts',(-44.9267631651733,35.3351673791874,173.54567696713));
#44566=CARTESIAN_POINT('Ctrl Pts',(-44.9267795602214,35.3353193641777,173.545524258522));
#44567=CARTESIAN_POINT('Ctrl Pts',(-44.9366852808817,35.427147143843,173.453259276234));
#44568=CARTESIAN_POINT('Ctrl Pts',(-44.9451008609219,35.5063351625277,173.350077657882));
#44569=CARTESIAN_POINT('Ctrl Pts',(-44.9520576904499,35.5723002038223,173.235485069079));
#44570=CARTESIAN_POINT('',(-45.0253923549998,36.2926583006112,171.985485069079));
#44571=CARTESIAN_POINT('Origin',(330.563412025084,138.023170571188,209.41117795471));
#44572=CARTESIAN_POINT('',(-45.451589062978,42.836266743522,171.985485069079));
#44573=CARTESIAN_POINT('Origin',(54.4964231308939,46.060372587574,171.985485069079));
#44574=CARTESIAN_POINT('',(-45.451589062978,42.836266743522,178.485485069079));
#44575=CARTESIAN_POINT('Origin',(54.4964231308939,46.060372587574,178.485485069079));
#44576=CARTESIAN_POINT('',(-45.5029364314847,46.4182651889755,171.985485069079));
#44577=CARTESIAN_POINT('',(-45.5028724868992,46.4357070320802,171.985485069079));
#44578=CARTESIAN_POINT('Origin',(54.4964231308939,46.060372587574,171.985485069079));
#44579=CARTESIAN_POINT('',(-45.5028724868992,46.4357070320802,179.985485069079));
#44580=CARTESIAN_POINT('',(-45.5028724868992,46.4357070320801,178.485485069079));
#44581=CARTESIAN_POINT('',(-45.5029364314846,46.4182651889755,179.985485069079));
#44582=CARTESIAN_POINT('Origin',(54.4964231308939,46.060372587574,179.985485069079));
#44583=CARTESIAN_POINT('',(-45.5029364314846,46.4182651889755,178.485485069079));
#44584=CARTESIAN_POINT('Origin',(-55.2932569457149,10.3110887801052,178.485485069079));
#44585=CARTESIAN_POINT('',(-56.491837111464,13.061253427226,173.985485069079));
#44586=CARTESIAN_POINT('',(-56.491837111464,13.061253427226,174.785485069079));
#44587=CARTESIAN_POINT('',(-56.491837111464,13.061253427226,178.485485069079));
#44588=CARTESIAN_POINT('',(-52.503810530151,11.4151669905134,173.985485069079));
#44589=CARTESIAN_POINT('Origin',(-55.2932569457149,10.3110887801052,173.985485069079));
#44590=CARTESIAN_POINT('',(-52.503810530151,11.4151669905134,174.785485069079));
#44591=CARTESIAN_POINT('',(-52.503810530151,11.4151669905134,178.485485069079));
#44592=CARTESIAN_POINT('Origin',(-55.2932569457149,10.3110887801052,174.785485069079));
#44593=CARTESIAN_POINT('Origin',(-69.9391102914966,14.1820463536532,178.485485069079));
#44594=CARTESIAN_POINT('',(-36.2883138077383,14.3227057076466,178.485485069079));
#44595=CARTESIAN_POINT('',(-43.2773451499467,22.8108513846653,178.485485069079));
#44596=CARTESIAN_POINT('Origin',(-31.1164286971058,25.7025828775644,178.485485069079));
#44597=CARTESIAN_POINT('',(-45.3036829175493,34.2202360714903,178.485485069079));
#44598=CARTESIAN_POINT('Origin',(54.4964231308939,46.060372587574,178.485485069079));
#44599=CARTESIAN_POINT('',(-51.7918181085456,40.3156359630969,178.485485069079));
#44600=CARTESIAN_POINT('Origin',(-45.3578332448047,40.663384199939,178.485485069079));
#44601=CARTESIAN_POINT('Origin',(54.4964231308939,46.060372587574,178.485485069079));
#44602=CARTESIAN_POINT('',(-58.9792278552929,42.2495403530246,178.485485069079));
#44603=CARTESIAN_POINT('Origin',(-31.8232466514532,37.9133340783293,178.485485069079));
#44604=CARTESIAN_POINT('Origin',(-94.0351308638859,47.8471884530858,178.485485069079));
#44605=CARTESIAN_POINT('',(-56.6916004724222,13.5196142017461,178.485485069079));
#44606=CARTESIAN_POINT('',(-67.58190263219,8.77338921431569,178.485485069079));
#44607=CARTESIAN_POINT('',(-52.0389027942237,11.5991800255814,178.485485069079));
#44608=CARTESIAN_POINT('Origin',(-55.2932569457149,10.3110887801052,178.485485069079));
#44609=CARTESIAN_POINT('',(-39.8623336503921,1.96564996953346,178.485485069079));
#44610=CARTESIAN_POINT('Origin',(-37.6267629804773,17.3035841126903,178.485485069079));
#44611=CARTESIAN_POINT('Origin',(-38.9776940652673,8.40516957928931,178.485485069079));
#44612=CARTESIAN_POINT('Origin',(-69.9391102914966,14.1820463536532,173.485485069079));
#44613=CARTESIAN_POINT('',(-43.2773451499467,22.8108513846653,173.485485069079));
#44614=CARTESIAN_POINT('',(-36.2883138077383,14.3227057076466,173.485485069079));
#44615=CARTESIAN_POINT('Origin',(-31.1164286971058,25.7025828775644,173.485485069079));
#44616=CARTESIAN_POINT('',(-39.8623336503919,1.96564996953342,173.485485069079));
#44617=CARTESIAN_POINT('Origin',(-38.9776940652673,8.40516957928931,173.485485069079));
#44618=CARTESIAN_POINT('',(-52.0389027942237,11.5991800255814,173.485485069079));
#44619=CARTESIAN_POINT('Origin',(-37.6267629804773,17.3035841126903,173.485485069079));
#44620=CARTESIAN_POINT('',(-56.6916004724222,13.5196142017461,173.485485069079));
#44621=CARTESIAN_POINT('Origin',(-55.2932569457149,10.3110887801052,173.485485069079));
#44622=CARTESIAN_POINT('',(-67.58190263219,8.77338921431569,173.485485069079));
#44623=CARTESIAN_POINT('',(-58.9792278552929,42.2495403530246,173.485485069079));
#44624=CARTESIAN_POINT('Origin',(-94.0351308638859,47.8471884530858,173.485485069079));
#44625=CARTESIAN_POINT('Origin',(-31.8232466514532,37.9133340783293,173.485485069079));
#44626=CARTESIAN_POINT('',(-51.7918181085456,40.3156359630969,173.485485069079));
#44627=CARTESIAN_POINT('Origin',(54.4964231308939,46.060372587574,173.485485069079));
#44628=CARTESIAN_POINT('',(-45.3036829175493,34.2202360714903,173.485485069079));
#44629=CARTESIAN_POINT('Origin',(-45.3578332448047,40.663384199939,173.485485069079));
#44630=CARTESIAN_POINT('Origin',(54.4964231308939,46.060372587574,173.485485069079));
#44631=CARTESIAN_POINT('Origin',(-67.3821392712318,8.31502843979556,178.485485069079));
#44632=CARTESIAN_POINT('',(-56.491837111464,13.061253427226,173.985485069079));
#44633=CARTESIAN_POINT('',(-63.4605999891139,10.0241185510634,174.785485069079));
#44634=CARTESIAN_POINT('',(-63.4605999891139,10.0241185510634,174.785485069079));
#44635=CARTESIAN_POINT('',(-63.4605999891139,10.0241185510634,177.185485069079));
#44636=CARTESIAN_POINT('',(-63.4605999891139,10.0241185510634,177.185485069079));
#44637=CARTESIAN_POINT('',(-56.491837111464,13.061253427226,177.185485069079));
#44638=CARTESIAN_POINT('',(-63.4605999891139,10.0241185510634,177.185485069079));
#44639=CARTESIAN_POINT('',(-56.491837111464,13.061253427226,177.985485069079));
#44640=CARTESIAN_POINT('',(-56.491837111464,13.061253427226,178.485485069079));
#44641=CARTESIAN_POINT('',(-67.3821392712318,8.31502843979556,177.985485069079));
#44642=CARTESIAN_POINT('Origin',(-37.6267629804773,17.3035841126903,178.485485069079));
#44643=CARTESIAN_POINT('',(-39.9344488332926,1.47087790039936,173.985485069079));
#44644=CARTESIAN_POINT('Origin',(-37.6267629804773,17.3035841126903,173.985485069079));
#44645=CARTESIAN_POINT('',(-39.9344488332926,1.47087790039936,177.985485069079));
#44646=CARTESIAN_POINT('',(-39.9344488332926,1.47087790039936,178.485485069079));
#44647=CARTESIAN_POINT('',(-52.503810530151,11.4151669905134,177.985485069079));
#44648=CARTESIAN_POINT('Origin',(-37.6267629804773,17.3035841126903,177.985485069079));
#44649=CARTESIAN_POINT('',(-52.503810530151,11.4151669905134,177.185485069079));
#44650=CARTESIAN_POINT('',(-52.503810530151,11.4151669905134,178.485485069079));
#44651=CARTESIAN_POINT('',(-51.1450921368114,8.74468366806501,177.185485069079));
#44652=CARTESIAN_POINT('Origin',(-37.6267629804773,17.3035841126903,177.185485069079));
#44653=CARTESIAN_POINT('',(-51.1450921368114,8.74468366806501,174.785485069079));
#44654=CARTESIAN_POINT('',(-51.1450921368114,8.74468366806501,178.485485069079));
#44655=CARTESIAN_POINT('Origin',(-37.6267629804773,17.3035841126903,174.785485069079));
#44656=CARTESIAN_POINT('Origin',(-38.9776940652673,8.40516957928931,178.485485069079));
#44657=CARTESIAN_POINT('',(-36.081438403313,14.7779007944433,177.985485069079));
#44658=CARTESIAN_POINT('',(-36.081438403313,14.7779007944433,173.985485069079));
#44659=CARTESIAN_POINT('',(-36.081438403313,14.7779007944433,178.485485069079));
#44660=CARTESIAN_POINT('',(-39.9303828492479,1.47030230724454,177.985485069079));
#44661=CARTESIAN_POINT('Origin',(-38.9776940652673,8.40516957928931,177.985485069079));
#44662=CARTESIAN_POINT('',(-39.9303828492479,1.47030230724454,173.985485069079));
#44663=CARTESIAN_POINT('',(-39.9303828492479,1.47030230724454,178.485485069079));
#44664=CARTESIAN_POINT('Origin',(-38.9776940652673,8.40516957928931,173.985485069079));
#44665=CARTESIAN_POINT('Origin',(-31.1164286971058,25.7025828775644,178.485485069079));
#44666=CARTESIAN_POINT('Origin',(-31.1164286971058,25.7025828775644,177.985485069079));
#44667=CARTESIAN_POINT('Origin',(-31.1164286971058,25.7025828775644,173.985485069079));
#44668=CARTESIAN_POINT('Origin',(-46.8813880107404,61.5195277317696,178.485485069079));
#44669=CARTESIAN_POINT('',(-46.8813880107404,61.5195277317696,171.985485069079));
#44670=CARTESIAN_POINT('',(-31.948047029133,59.4635250419104,171.985485069079));
#44671=CARTESIAN_POINT('',(-46.8813880107404,61.5195277317696,179.985485069079));
#44672=CARTESIAN_POINT('',(-46.8813880107404,61.5195277317696,178.485485069079));
#44673=CARTESIAN_POINT('',(-31.948047029133,59.4635250419104,179.985485069079));
#44674=CARTESIAN_POINT('Origin',(-31.8232466514532,37.9133340783293,178.485485069079));
#44675=CARTESIAN_POINT('',(-48.5106524275047,60.3973392500139,172.002119756093));
#44676=CARTESIAN_POINT('Origin',(-31.8232468038171,37.913334302383,123.527223858898));
#44677=CARTESIAN_POINT('',(-49.7140665684645,59.4521029079787,173.235485069079));
#44678=CARTESIAN_POINT('Ctrl Pts',(-48.5106524258229,60.397339249151,172.002119757177));
#44679=CARTESIAN_POINT('Ctrl Pts',(-48.7316538537475,60.2333141799307,172.21440215845));
#44680=CARTESIAN_POINT('Ctrl Pts',(-48.9480214903638,60.0676803472184,172.429976071149));
#44681=CARTESIAN_POINT('Ctrl Pts',(-49.1601443335358,59.9004207148303,172.648442205403));
#44682=CARTESIAN_POINT('Ctrl Pts',(-49.3480302095647,59.7522720190766,172.841946593724));
#44683=CARTESIAN_POINT('Ctrl Pts',(-49.5325856738131,59.6028469932263,173.037720036652));
#44684=CARTESIAN_POINT('Ctrl Pts',(-49.7140665684645,59.4521029079787,173.235485069079));
#44685=CARTESIAN_POINT('',(-51.5969475386142,57.7375806775091,173.985485069079));
#44686=CARTESIAN_POINT('Ctrl Pts',(-49.7140665684645,59.4521029079787,173.235485069079));
#44687=CARTESIAN_POINT('Ctrl Pts',(-49.7702877045322,59.40540375684,173.296750850855));
#44688=CARTESIAN_POINT('Ctrl Pts',(-49.8290566284154,59.3562043812518,173.351977274771));
#44689=CARTESIAN_POINT('Ctrl Pts',(-49.8897735927165,59.3049226058545,173.402403825032));
#44690=CARTESIAN_POINT('Ctrl Pts',(-49.9574087083972,59.2477977338977,173.458576026648));
#44691=CARTESIAN_POINT('Ctrl Pts',(-50.0274613646153,59.1880887736131,173.508791806356));
#44692=CARTESIAN_POINT('Ctrl Pts',(-50.0991284022786,59.1263501189538,173.554708958926));
#44693=CARTESIAN_POINT('Ctrl Pts',(-50.1165153850139,59.1113718394314,173.565848818547));
#44694=CARTESIAN_POINT('Ctrl Pts',(-50.1339974820091,59.0962740044815,173.57673545706));
#44695=CARTESIAN_POINT('Ctrl Pts',(-50.1515633825625,59.0810643724353,173.587392186236));
#44696=CARTESIAN_POINT('Ctrl Pts',(-50.1520299561151,59.0806603844908,173.587675243059));
#44697=CARTESIAN_POINT('Ctrl Pts',(-50.1524965742564,59.0802563304049,173.587958114495));
#44698=CARTESIAN_POINT('Ctrl Pts',(-50.1529632368644,59.0798522102724,173.588240800684));
#44699=CARTESIAN_POINT('Ctrl Pts',(-50.2598834533621,58.9872615220365,173.65300893928));
#44700=CARTESIAN_POINT('Ctrl Pts',(-50.3690847000011,58.8912502411584,173.708028845801));
#44701=CARTESIAN_POINT('Ctrl Pts',(-50.4789853714511,58.7930624806832,173.754884245436));
#44702=CARTESIAN_POINT('Ctrl Pts',(-50.5283832256402,58.748929313787,173.775944682726));
#44703=CARTESIAN_POINT('Ctrl Pts',(-50.5779226519178,58.7043561380883,173.795354969797));
#44704=CARTESIAN_POINT('Ctrl Pts',(-50.6274609387914,58.6594548008981,173.813255995888));
#44705=CARTESIAN_POINT('Ctrl Pts',(-50.6279626824395,58.6590000221371,173.813437304663));
#44706=CARTESIAN_POINT('Ctrl Pts',(-50.6284644410244,58.6585451959672,173.813618467378));
#44707=CARTESIAN_POINT('Ctrl Pts',(-50.6289662145065,58.6580903224183,173.813799484048));
#44708=CARTESIAN_POINT('Ctrl Pts',(-50.7487120446439,58.5495369359429,173.856998242433));
#44709=CARTESIAN_POINT('Ctrl Pts',(-50.8693781916856,58.4382190449704,173.891907000424));
#44710=CARTESIAN_POINT('Ctrl Pts',(-50.9902670073361,58.3246866825487,173.918668263286));
#44711=CARTESIAN_POINT('Ctrl Pts',(-51.1134618427744,58.208988628678,173.945940011766));
#44712=CARTESIAN_POINT('Ctrl Pts',(-51.2368872549444,58.0909912797521,173.964750480356));
#44713=CARTESIAN_POINT('Ctrl Pts',(-51.3598062968599,57.9712894091945,173.975303121585));
#44714=CARTESIAN_POINT('Ctrl Pts',(-51.4391294462271,57.8940423918909,173.982113040727));
#44715=CARTESIAN_POINT('Ctrl Pts',(-51.5182417735722,57.816085767135,173.985485068216));
#44716=CARTESIAN_POINT('Ctrl Pts',(-51.5969475386142,57.7375806775091,173.985485069079));
#44717=CARTESIAN_POINT('',(-59.47297296809,42.32838046711,173.985485069079));
#44718=CARTESIAN_POINT('Origin',(-31.8232466514532,37.9133340783293,173.985485069079));
#44719=CARTESIAN_POINT('',(-59.47297296809,42.32838046711,177.985485069079));
#44720=CARTESIAN_POINT('',(-59.47297296809,42.32838046711,178.485485069079));
#44721=CARTESIAN_POINT('',(-51.5969475386134,57.7375806775099,177.985485069079));
#44722=CARTESIAN_POINT('Origin',(-31.8232466514532,37.9133340783293,177.985485069079));
#44723=CARTESIAN_POINT('',(-49.7140665684619,59.4521029079808,178.735485069082));
#44724=CARTESIAN_POINT('Ctrl Pts',(-51.5969475386134,57.7375806775099,177.985485069079));
#44725=CARTESIAN_POINT('Ctrl Pts',(-51.433703588371,57.9004084060484,177.985485071801));
#44726=CARTESIAN_POINT('Ctrl Pts',(-51.2699997021575,58.0596677833207,177.999692054503));
#44727=CARTESIAN_POINT('Ctrl Pts',(-51.1060428182335,58.2153933063291,178.028948066425));
#44728=CARTESIAN_POINT('Ctrl Pts',(-50.9473469135473,58.3661219745319,178.057265323794));
#44729=CARTESIAN_POINT('Ctrl Pts',(-50.788413804564,58.5135399732425,178.099681112438));
#44730=CARTESIAN_POINT('Ctrl Pts',(-50.6294298361607,58.6576700285617,178.157004738339));
#44731=CARTESIAN_POINT('Ctrl Pts',(-50.6289321865702,58.6581211826229,178.157184172021));
#44732=CARTESIAN_POINT('Ctrl Pts',(-50.6284345366926,58.6585723042698,178.157363751845));
#44733=CARTESIAN_POINT('Ctrl Pts',(-50.6279368865303,58.6590233935062,178.157543477836));
#44734=CARTESIAN_POINT('Ctrl Pts',(-50.5201533201667,58.7567225611635,178.196469433668));
#44735=CARTESIAN_POINT('Ctrl Pts',(-50.4124428574924,58.8527839753199,178.242613327577));
#44736=CARTESIAN_POINT('Ctrl Pts',(-50.3069537754469,58.9455000636963,178.296772170668));
#44737=CARTESIAN_POINT('Ctrl Pts',(-50.2547510309871,58.9913819139786,178.323573430014));
#44738=CARTESIAN_POINT('Ctrl Pts',(-50.2030925436158,59.0364442219574,178.352338018868));
#44739=CARTESIAN_POINT('Ctrl Pts',(-50.1522410770556,59.0804775615926,178.383166052784));
#44740=CARTESIAN_POINT('Ctrl Pts',(-50.151769832075,59.0808856223957,178.383451738866));
#44741=CARTESIAN_POINT('Ctrl Pts',(-50.1512986579747,59.0812935934674,178.383737601257));
#44742=CARTESIAN_POINT('Ctrl Pts',(-50.1508275549506,59.0817014746528,178.384023640042));
#44743=CARTESIAN_POINT('Ctrl Pts',(-50.0801323160474,59.1429094405883,178.426947542415));
#44744=CARTESIAN_POINT('Ctrl Pts',(-50.0105901739914,59.2024832025505,178.473668141392));
#44745=CARTESIAN_POINT('Ctrl Pts',(-49.9429408461552,59.2599050601864,178.52593231009));
#44746=CARTESIAN_POINT('Ctrl Pts',(-49.8833761345708,59.3104645631132,178.571950507672));
#44747=CARTESIAN_POINT('Ctrl Pts',(-49.8252786144112,59.3593558598453,178.622266054504));
#44748=CARTESIAN_POINT('Ctrl Pts',(-49.7691680069517,59.4062115438254,178.678108553083));
#44749=CARTESIAN_POINT('Ctrl Pts',(-49.7505761117354,59.421736878629,178.696611612116));
#44750=CARTESIAN_POINT('Ctrl Pts',(-49.7322025031268,59.4370385956386,178.715721822545));
#44751=CARTESIAN_POINT('Ctrl Pts',(-49.7140665684645,59.4521029079787,178.735485069079));
#44752=CARTESIAN_POINT('',(-48.5106524275049,60.3973392500138,179.968850382066));
#44753=CARTESIAN_POINT('Ctrl Pts',(-49.7140665684619,59.4521029079808,178.735485069082));
#44754=CARTESIAN_POINT('Ctrl Pts',(-49.509174938667,59.622292730814,178.958761463483));
#44755=CARTESIAN_POINT('Ctrl Pts',(-49.3003647583648,59.790802054021,179.179499303694));
#44756=CARTESIAN_POINT('Ctrl Pts',(-49.0872665483285,59.9576897504803,179.397299299844));
#44757=CARTESIAN_POINT('Ctrl Pts',(-48.898516749987,60.1055090073713,179.590213662405));
#44758=CARTESIAN_POINT('Ctrl Pts',(-48.7064024274161,60.2520555382595,179.78082317782));
#44759=CARTESIAN_POINT('Ctrl Pts',(-48.510652425823,60.3973392491509,179.968850380982));
#44760=CARTESIAN_POINT('Origin',(-31.8232463273633,37.9133336074862,228.443747738763));
#44761=CARTESIAN_POINT('Origin',(-94.0351308638859,47.8471884530858,178.485485069079));
#44762=CARTESIAN_POINT('Origin',(-94.0351308638859,47.8471884530858,177.985485069079));
#44763=CARTESIAN_POINT('Origin',(-94.0351308638859,47.8471884530858,173.985485069079));
#44764=CARTESIAN_POINT('Origin',(-38.9776940652673,8.4051695792893,171.985485069079));
#44765=CARTESIAN_POINT('',(-45.5229719821255,35.6661118192205,171.985485119952));
#44766=CARTESIAN_POINT('Ctrl Pts',(-45.0253923549778,36.2926583001986,171.985485069079));
#44767=CARTESIAN_POINT('Ctrl Pts',(-45.0176017947525,36.2132814174925,171.985485069079));
#44768=CARTESIAN_POINT('Ctrl Pts',(-45.0239871095741,36.1325427086669,171.985485069079));
#44769=CARTESIAN_POINT('Ctrl Pts',(-45.0636400627614,35.9874810744531,171.985485069079));
#44770=CARTESIAN_POINT('Ctrl Pts',(-45.0937395261308,35.9226089710175,171.985485069079));
#44771=CARTESIAN_POINT('Ctrl Pts',(-45.1741039151965,35.811784947861,171.985485069079));
#44772=CARTESIAN_POINT('Ctrl Pts',(-45.2225142153187,35.7657141441877,171.985485069079));
#44773=CARTESIAN_POINT('Ctrl Pts',(-45.3170765407724,35.7079918417109,171.985485069079));
#44774=CARTESIAN_POINT('Ctrl Pts',(-45.35816069493,35.6904301269908,171.985485069079));
#44775=CARTESIAN_POINT('Ctrl Pts',(-45.4411069174444,35.6692181889851,171.985485069079));
#44776=CARTESIAN_POINT('Ctrl Pts',(-45.4819542285517,35.6647560993595,171.985485069079));
#44777=CARTESIAN_POINT('Ctrl Pts',(-45.5229716741717,35.666111487147,171.985485069079));
#44778=CARTESIAN_POINT('',(-50.3505460635896,40.3935347805572,171.985485069079));
#44779=CARTESIAN_POINT('Origin',(-45.3578332448047,40.663384199939,171.985485069079));
#44780=CARTESIAN_POINT('',(-50.0854109028112,55.4219958520818,171.985485069079));
#44781=CARTESIAN_POINT('Origin',(54.4964231308939,46.060372587574,171.985485069079));
#44782=CARTESIAN_POINT('',(-48.8396164156005,60.0041865017348,171.985485044813));
#44783=CARTESIAN_POINT('Origin',(-36.5934363437889,54.2142642791517,171.985485069079));
#44784=CARTESIAN_POINT('',(-48.5925895957766,60.3286139604208,171.985485069079));
#44785=CARTESIAN_POINT('Ctrl Pts',(-48.8396208834494,60.0041886143,171.985485069079));
#44786=CARTESIAN_POINT('Ctrl Pts',(-48.8104873581851,60.0658028957206,171.985485069079));
#44787=CARTESIAN_POINT('Ctrl Pts',(-48.7734354054051,60.1243517973398,171.985485071599));
#44788=CARTESIAN_POINT('Ctrl Pts',(-48.6900390743796,60.2323373406952,171.985485071599));
#44789=CARTESIAN_POINT('Ctrl Pts',(-48.6430278708974,60.2826903631409,171.985485069079));
#44790=CARTESIAN_POINT('Ctrl Pts',(-48.5925895957754,60.3286139604194,171.985485069079));
#44791=CARTESIAN_POINT('',(-66.4598969965647,47.8938297558071,171.985485069079));
#44792=CARTESIAN_POINT('',(-45.7483677109949,58.3231663243772,171.985485069079));
#44793=CARTESIAN_POINT('',(-44.6376627105729,59.1917481581946,171.985485069079));
#44794=CARTESIAN_POINT('',(-44.949586852714,57.3017198020218,171.985485069079));
#44795=CARTESIAN_POINT('',(-45.7483677109949,58.3231663243772,171.985485069079));
#44796=CARTESIAN_POINT('',(-45.9329959574027,56.5326845647457,171.985485069079));
#44797=CARTESIAN_POINT('',(-44.8222909569807,57.4012663985631,171.985485069079));
#44798=CARTESIAN_POINT('',(-45.1205026113461,55.4937031042329,171.985485069079));
#44799=CARTESIAN_POINT('',(-45.9329959574027,56.5326845647457,171.985485069079));
#44800=CARTESIAN_POINT('',(-46.0853673634888,54.7391697263481,171.985485069079));
#44801=CARTESIAN_POINT('',(-44.9746623630668,55.6077515601656,171.985485069079));
#44802=CARTESIAN_POINT('',(-45.2594247703932,53.6829899485823,171.985485069079));
#44803=CARTESIAN_POINT('',(-46.0853673634888,54.7391697263481,171.985485069079));
#44804=CARTESIAN_POINT('',(-46.2054325622506,52.9432028923028,171.985485069079));
#44805=CARTESIAN_POINT('',(-45.0947275618286,53.8117847261202,171.985485069079));
#44806=CARTESIAN_POINT('',(-45.3663083202907,51.8701669902924,171.985485069079));
#44807=CARTESIAN_POINT('',(-46.2054325622506,52.9432028923028,171.985485069079));
#44808=CARTESIAN_POINT('',(-46.293152653614,51.1453659401528,171.985485069079));
#44809=CARTESIAN_POINT('',(-45.182447653192,52.0139477739702,171.985485069079));
#44810=CARTESIAN_POINT('',(-45.4411186317038,50.0558215681434,171.985485069079));
#44811=CARTESIAN_POINT('',(-46.293152653614,51.1453659401528,171.985485069079));
#44812=CARTESIAN_POINT('',(-46.3484992170368,49.3462413533434,171.985485069079));
#44813=CARTESIAN_POINT('',(-45.2377942166148,50.2148231871608,171.985485069079));
#44814=CARTESIAN_POINT('',(-45.4838314667458,48.2405415141803,171.985485069079));
#44815=CARTESIAN_POINT('',(-46.3484992170368,49.3462413533434,171.985485069079));
#44816=CARTESIAN_POINT('',(-46.3714543207166,47.5464120325021,171.985485069079));
#44817=CARTESIAN_POINT('',(-45.2607493202947,48.4149938663196,171.985485069079));
#44818=CARTESIAN_POINT('',(-46.3714543207166,47.5464120325021,171.985485069079));
#44819=CARTESIAN_POINT('',(-46.3620105274007,45.7464611065843,171.985485069079));
#44820=CARTESIAN_POINT('',(-45.2513055269787,46.6150429404017,171.985485069079));
#44821=CARTESIAN_POINT('',(-46.3620105274007,45.7464611065843,171.985485069079));
#44822=CARTESIAN_POINT('',(-46.3201708967954,43.9469717439439,171.985485069079));
#44823=CARTESIAN_POINT('',(-45.2094658963734,44.8155535777614,171.985485069079));
#44824=CARTESIAN_POINT('',(-46.3201708967954,43.9469717439439,171.985485069079));
#44825=CARTESIAN_POINT('Origin',(54.4964231308939,46.060372587574,171.985485069079));
#44826=CARTESIAN_POINT('',(-50.927054881572,40.3623752535731,172.985485069079));
#44827=CARTESIAN_POINT('',(-50.3505460635896,40.3935347805572,171.985485069079));
#44828=CARTESIAN_POINT('Origin',(54.4964231308939,46.060372587574,172.985485069079));
#44829=CARTESIAN_POINT('',(-50.0854109028112,55.4219958520819,171.985485069079));
#44830=CARTESIAN_POINT('Origin',(-36.5934363437889,54.2142642791517,171.985485069079));
#44831=CARTESIAN_POINT('Ctrl Pts',(-49.7994785223376,59.2209856988867,172.985485069079));
#44832=CARTESIAN_POINT('Ctrl Pts',(-49.4892805846571,59.4856670319597,172.645618020514));
#44833=CARTESIAN_POINT('Ctrl Pts',(-49.1697658047785,59.7466931532137,172.311831139785));
#44834=CARTESIAN_POINT('Ctrl Pts',(-48.8396130608551,60.0041835729237,171.985486127831));
#44835=CARTESIAN_POINT('Origin',(-66.4598969965647,47.8938297558071,171.985485069079));
#44836=CARTESIAN_POINT('Ctrl Pts',(-48.5925895957742,60.3286139604199,171.985485069075));
#44837=CARTESIAN_POINT('Ctrl Pts',(-48.5801791134111,60.3407485993548,171.990457348712));
#44838=CARTESIAN_POINT('Ctrl Pts',(-48.5668415570095,60.3526167618077,171.994133545212));
#44839=CARTESIAN_POINT('Ctrl Pts',(-48.5394083236438,60.3754624609016,171.99946969614));
#44840=CARTESIAN_POINT('Ctrl Pts',(-48.525119006316,60.3866023176528,172.001168825203));
#44841=CARTESIAN_POINT('Ctrl Pts',(-48.5106524368776,60.3973392472798,172.002119759697));
#44842=CARTESIAN_POINT('Origin',(-45.3578332448047,40.663384199939,171.985485069079));
#44843=CARTESIAN_POINT('',(-45.4569991048231,35.0869155900178,172.985485069079));
#44844=CARTESIAN_POINT('Origin',(488.633838875382,289.196466346075,284.259200636902));
#44845=CARTESIAN_POINT('Origin',(-45.3578332448047,40.663384199939,172.985485069079));
#44846=CARTESIAN_POINT('Origin',(-45.3578332448047,40.663384199939,179.985485069079));
#44847=CARTESIAN_POINT('',(-50.927054881572,40.3623752535731,178.985485069079));
#44848=CARTESIAN_POINT('',(-45.4569991048231,35.0869155900178,178.985485069079));
#44849=CARTESIAN_POINT('Origin',(-45.3578332448047,40.663384199939,178.985485069079));
#44850=CARTESIAN_POINT('',(-45.5229719821697,35.6661118192729,179.985485018174));
#44851=CARTESIAN_POINT('Origin',(488.633838896208,289.196466334528,67.7117695084859));
#44852=CARTESIAN_POINT('',(-50.3505460635896,40.3935347805572,179.985485069079));
#44853=CARTESIAN_POINT('Origin',(-45.3578332448047,40.663384199939,179.985485069079));
#44854=CARTESIAN_POINT('',(-50.3505460635896,40.3935347805572,179.985485069079));
#44855=CARTESIAN_POINT('Origin',(-66.4598969965647,47.8938297558071,179.985485069079));
#44856=CARTESIAN_POINT('',(-48.5925895957765,60.3286139604208,179.985485069079));
#44857=CARTESIAN_POINT('Ctrl Pts',(-48.5106524368779,60.3973392472796,179.968850378462));
#44858=CARTESIAN_POINT('Ctrl Pts',(-48.5251190063152,60.3866023176534,179.969801312955));
#44859=CARTESIAN_POINT('Ctrl Pts',(-48.5394083236435,60.3754624609018,179.971500442019));
#44860=CARTESIAN_POINT('Ctrl Pts',(-48.5668415570078,60.3526167618089,179.976836592946));
#44861=CARTESIAN_POINT('Ctrl Pts',(-48.5801791134102,60.3407485993553,179.980512789447));
#44862=CARTESIAN_POINT('Ctrl Pts',(-48.5925895957738,60.3286139604199,179.985485069084));
#44863=CARTESIAN_POINT('',(-66.4598969965647,47.8938297558071,179.985485069079));
#44864=CARTESIAN_POINT('Origin',(-36.5934363437889,54.2142642791517,179.985485069079));
#44865=CARTESIAN_POINT('',(-48.8396164156006,60.0041865017348,179.985485093346));
#44866=CARTESIAN_POINT('',(-50.0854109028112,55.4219958520818,179.985485069079));
#44867=CARTESIAN_POINT('Origin',(-36.5934363437889,54.2142642791517,179.985485069079));
#44868=CARTESIAN_POINT('Ctrl Pts',(-48.8396130608551,60.0041835729237,179.985484010327));
#44869=CARTESIAN_POINT('Ctrl Pts',(-49.1697658047781,59.7466931532141,179.659138998374));
#44870=CARTESIAN_POINT('Ctrl Pts',(-49.489280584655,59.4856670319615,179.325352117647));
#44871=CARTESIAN_POINT('Ctrl Pts',(-49.7994785223364,59.2209856988899,178.985485069079));
#44872=CARTESIAN_POINT('',(-50.0854109028112,55.4219958520818,179.985485069079));
#44873=CARTESIAN_POINT('Origin',(54.4964231308939,46.060372587574,179.985485069079));
#44874=CARTESIAN_POINT('Origin',(54.4964231308939,46.060372587574,178.985485069079));
#44875=CARTESIAN_POINT('Origin',(54.4964231308939,46.060372587574,179.985485069079));
#44876=CARTESIAN_POINT('Origin',(-38.9776940652673,8.4051695792893,179.985485069079));
#44877=CARTESIAN_POINT('Ctrl Pts',(-45.5229716741763,35.6661114871472,179.985485069079));
#44878=CARTESIAN_POINT('Ctrl Pts',(-45.4821910556965,35.6647639251181,179.985485069079));
#44879=CARTESIAN_POINT('Ctrl Pts',(-45.4415765396099,35.6691667965979,179.985485069079));
#44880=CARTESIAN_POINT('Ctrl Pts',(-45.3590894448663,35.6901192458687,179.985485069079));
#44881=CARTESIAN_POINT('Ctrl Pts',(-45.3182137267096,35.7074699102648,179.985485069079));
#44882=CARTESIAN_POINT('Ctrl Pts',(-45.2237659769383,35.7647003566238,179.985485069079));
#44883=CARTESIAN_POINT('Ctrl Pts',(-45.175266512742,35.8105527807682,179.985485069079));
#44884=CARTESIAN_POINT('Ctrl Pts',(-45.0946358711023,35.9209880541501,179.985485069079));
#44885=CARTESIAN_POINT('Ctrl Pts',(-45.0643644570102,35.9856925299171,179.985485069079));
#44886=CARTESIAN_POINT('Ctrl Pts',(-45.0240949599695,36.1311938017274,179.985485069079));
#44887=CARTESIAN_POINT('Ctrl Pts',(-45.017536669623,36.2126178670405,179.985485069079));
#44888=CARTESIAN_POINT('Ctrl Pts',(-45.0253923549778,36.2926583001987,179.985485069079));
#44889=CARTESIAN_POINT('',(-46.3201708967954,43.9469717439439,179.985485069079));
#44890=CARTESIAN_POINT('',(-44.1642119224607,41.1900243611352,179.985485069079));
#44891=CARTESIAN_POINT('',(-45.2094658963734,44.8155535777614,179.985485069079));
#44892=CARTESIAN_POINT('',(-46.3620105274007,45.7464611065843,179.985485069079));
#44893=CARTESIAN_POINT('',(-44.206051553066,42.9895137237755,179.985485069079));
#44894=CARTESIAN_POINT('',(-45.2513055269787,46.6150429404017,179.985485069079));
#44895=CARTESIAN_POINT('',(-46.3714543207166,47.5464120325021,179.985485069079));
#44896=CARTESIAN_POINT('',(-44.2154953463819,44.7894646496933,179.985485069079));
#44897=CARTESIAN_POINT('',(-45.4838314667458,48.2405415141803,179.985485069079));
#44898=CARTESIAN_POINT('',(-45.2607493202947,48.4149938663196,179.985485069079));
#44899=CARTESIAN_POINT('',(-46.3484992170368,49.3462413533434,179.985485069079));
#44900=CARTESIAN_POINT('',(-44.1925402427021,46.5892939705346,179.985485069079));
#44901=CARTESIAN_POINT('',(-45.4411186317038,50.0558215681434,179.985485069079));
#44902=CARTESIAN_POINT('',(-45.2377942166148,50.2148231871608,179.985485069079));
#44903=CARTESIAN_POINT('',(-46.293152653614,51.1453659401528,179.985485069079));
#44904=CARTESIAN_POINT('',(-44.1371936792793,48.388418557344,179.985485069079));
#44905=CARTESIAN_POINT('',(-45.3663083202907,51.8701669902924,179.985485069079));
#44906=CARTESIAN_POINT('',(-45.182447653192,52.0139477739702,179.985485069079));
#44907=CARTESIAN_POINT('',(-46.2054325622506,52.9432028923028,179.985485069079));
#44908=CARTESIAN_POINT('',(-44.0494735879158,50.186255509494,179.985485069079));
#44909=CARTESIAN_POINT('',(-45.2594247703932,53.6829899485823,179.985485069079));
#44910=CARTESIAN_POINT('',(-45.0947275618286,53.8117847261202,179.985485069079));
#44911=CARTESIAN_POINT('',(-46.0853673634888,54.7391697263481,179.985485069079));
#44912=CARTESIAN_POINT('',(-43.9294083891541,51.9822223435394,179.985485069079));
#44913=CARTESIAN_POINT('',(-45.1205026113461,55.4937031042329,179.985485069079));
#44914=CARTESIAN_POINT('',(-44.9746623630668,55.6077515601656,179.985485069079));
#44915=CARTESIAN_POINT('',(-45.9329959574027,56.5326845647457,179.985485069079));
#44916=CARTESIAN_POINT('',(-43.777036983068,53.7757371819369,179.985485069079));
#44917=CARTESIAN_POINT('',(-44.949586852714,57.3017198020218,179.985485069079));
#44918=CARTESIAN_POINT('',(-44.8222909569807,57.4012663985631,179.985485069079));
#44919=CARTESIAN_POINT('',(-45.7483677109949,58.3231663243772,179.985485069079));
#44920=CARTESIAN_POINT('',(-43.5924087366602,55.5662189415684,179.985485069079));
#44921=CARTESIAN_POINT('',(-65.7700217936225,42.6660431345655,179.985485069079));
#44922=CARTESIAN_POINT('Ctrl Pts',(-48.5925895957752,60.3286139604194,179.985485069079));
#44923=CARTESIAN_POINT('Ctrl Pts',(-48.6430370917591,60.2826819676288,179.985485069079));
#44924=CARTESIAN_POINT('Ctrl Pts',(-48.6900563305759,60.232318868423,179.985485066651));
#44925=CARTESIAN_POINT('Ctrl Pts',(-48.7734488840562,60.1243304643096,179.985485066651));
#44926=CARTESIAN_POINT('Ctrl Pts',(-48.8104926495586,60.0657917050398,179.985485069079));
#44927=CARTESIAN_POINT('Ctrl Pts',(-48.8396208834495,60.0041886143001,179.985485069079));
#44928=CARTESIAN_POINT('Origin',(-45.3578332448047,40.663384199939,179.485485069079));
#44929=CARTESIAN_POINT('Ctrl Pts',(-45.3036829175493,34.2202360714903,178.485485069079));
#44930=CARTESIAN_POINT('Ctrl Pts',(-45.3189505131708,34.3080655568667,178.485485069079));
#44931=CARTESIAN_POINT('Ctrl Pts',(-45.3338848762283,34.3938033049738,178.496890676795));
#44932=CARTESIAN_POINT('Ctrl Pts',(-45.3485335977834,34.4775333459783,178.519211521199));
#44933=CARTESIAN_POINT('Ctrl Pts',(-45.3485497210739,34.4776255044486,178.519236088903));
#44934=CARTESIAN_POINT('Ctrl Pts',(-45.3485658440143,34.4777176604645,178.519260669829));
#44935=CARTESIAN_POINT('Ctrl Pts',(-45.348581966605,34.4778098140261,178.519285263975));
#44936=CARTESIAN_POINT('Ctrl Pts',(-45.3614851957113,34.5515621375495,178.53896844682));
#44937=CARTESIAN_POINT('Ctrl Pts',(-45.3742367759305,34.6241378461091,178.56762577006));
#44938=CARTESIAN_POINT('Ctrl Pts',(-45.3862037841395,34.6918764218863,178.603791729928));
#44939=CARTESIAN_POINT('Ctrl Pts',(-45.387807086225,34.7009518230151,178.608637131374));
#44940=CARTESIAN_POINT('Ctrl Pts',(-45.3893962981546,34.7099403541399,178.613617373854));
#44941=CARTESIAN_POINT('Ctrl Pts',(-45.3909698892282,34.7188331600865,178.618728986713));
#44942=CARTESIAN_POINT('Ctrl Pts',(-45.3909996250014,34.719001205308,178.618825579635));
#44943=CARTESIAN_POINT('Ctrl Pts',(-45.3910293556473,34.7191692188888,178.61892222093));
#44944=CARTESIAN_POINT('Ctrl Pts',(-45.3910590811527,34.7193372007523,178.61901891057));
#44945=CARTESIAN_POINT('Ctrl Pts',(-45.3968750896393,34.7522040580152,178.637936932599));
#44946=CARTESIAN_POINT('Ctrl Pts',(-45.4025476904675,34.7841474493449,178.658893238736));
#44947=CARTESIAN_POINT('Ctrl Pts',(-45.4080183431112,34.8148573132726,178.681656749639));
#44948=CARTESIAN_POINT('Ctrl Pts',(-45.4135433861197,34.8458725010455,178.704646580094));
#44949=CARTESIAN_POINT('Ctrl Pts',(-45.4188622767047,34.8756286399688,178.729479042991));
#44950=CARTESIAN_POINT('Ctrl Pts',(-45.4239193913347,34.903835066337,178.755872459173));
#44951=CARTESIAN_POINT('Ctrl Pts',(-45.4253049650645,34.9115632050574,178.763103860234));
#44952=CARTESIAN_POINT('Ctrl Pts',(-45.4266709229058,34.9191752174847,178.770452222341));
#44953=CARTESIAN_POINT('Ctrl Pts',(-45.4280162071684,34.9266656301276,178.777911297277));
#44954=CARTESIAN_POINT('Ctrl Pts',(-45.431900150492,34.9482910508554,178.799446243539));
#44955=CARTESIAN_POINT('Ctrl Pts',(-45.4356071123145,34.9688770623761,178.821871912933));
#44956=CARTESIAN_POINT('Ctrl Pts',(-45.4391361091639,34.9884275421567,178.845188937286));
#44957=CARTESIAN_POINT('Ctrl Pts',(-45.4425882966433,35.0075525015699,178.867998461624));
#44958=CARTESIAN_POINT('Ctrl Pts',(-45.4458702772851,35.0256869893978,178.891661629521));
#44959=CARTESIAN_POINT('Ctrl Pts',(-45.4489746253575,35.042796910032,178.916209181352));
#44960=CARTESIAN_POINT('Ctrl Pts',(-45.4518004907941,35.0583719461472,178.938554638967));
#44961=CARTESIAN_POINT('Ctrl Pts',(-45.4544791600941,35.0730979247513,178.961633558394));
#44962=CARTESIAN_POINT('Ctrl Pts',(-45.4569991048231,35.0869155900178,178.985485069079));
#44963=CARTESIAN_POINT('Origin',(-51.7918181085456,40.3156359630969,179.485485069079));
#44964=CARTESIAN_POINT('Origin',(54.4964231308939,46.060372587574,179.485485069079));
#44965=CARTESIAN_POINT('Origin',(-45.3578332448047,40.663384199939,172.485485069079));
#44966=CARTESIAN_POINT('Ctrl Pts',(-45.4569991048231,35.0869155900178,172.985485069079));
#44967=CARTESIAN_POINT('Ctrl Pts',(-45.4494550799535,35.0455492823621,173.056889963465));
#44968=CARTESIAN_POINT('Ctrl Pts',(-45.4405646313053,34.9965213246108,173.121515548973));
#44969=CARTESIAN_POINT('Ctrl Pts',(-45.4304424047398,34.9402282867916,173.179712320665));
#44970=CARTESIAN_POINT('Ctrl Pts',(-45.4296958966764,34.9360767094311,173.184004297243));
#44971=CARTESIAN_POINT('Ctrl Pts',(-45.4289426856633,34.9318855998601,173.188261292746));
#44972=CARTESIAN_POINT('Ctrl Pts',(-45.4281828161243,34.9276551088421,173.192483440716));
#44973=CARTESIAN_POINT('Ctrl Pts',(-45.4281583546134,34.9275189220408,173.192619358941));
#44974=CARTESIAN_POINT('Ctrl Pts',(-45.4281338855781,34.9273826908262,173.192755241168));
#44975=CARTESIAN_POINT('Ctrl Pts',(-45.4281094090274,34.9272464152488,173.192891087362));
#44976=CARTESIAN_POINT('Ctrl Pts',(-45.4181985665645,34.8720668355002,173.247896804654));
#44977=CARTESIAN_POINT('Ctrl Pts',(-45.4070570723305,34.8096241895739,173.296989238882));
#44978=CARTESIAN_POINT('Ctrl Pts',(-45.3952940807049,34.7432514620707,173.337731815262));
#44979=CARTESIAN_POINT('Ctrl Pts',(-45.3939189104418,34.7354920583365,173.342494887554));
#44980=CARTESIAN_POINT('Ctrl Pts',(-45.3925352362935,34.7276788857477,173.347143832958));
#44981=CARTESIAN_POINT('Ctrl Pts',(-45.391144024528,34.71981722941,173.351674748709));
#44982=CARTESIAN_POINT('Ctrl Pts',(-45.391113929105,34.7196471619343,173.351772763857));
#44983=CARTESIAN_POINT('Ctrl Pts',(-45.3910838287156,34.7194770634957,173.351870728113));
#44984=CARTESIAN_POINT('Ctrl Pts',(-45.391053723366,34.7193069341307,173.351968641468));
#44985=CARTESIAN_POINT('Ctrl Pts',(-45.3853123614024,34.686861728367,173.370641602265));
#44986=CARTESIAN_POINT('Ctrl Pts',(-45.3793724983653,34.653189475525,173.387517101079));
#44987=CARTESIAN_POINT('Ctrl Pts',(-45.3732936451112,34.6186406634444,173.402457951648));
#44988=CARTESIAN_POINT('Ctrl Pts',(-45.3671493578082,34.5837199607191,173.41755962866));
#44989=CARTESIAN_POINT('Ctrl Pts',(-45.3608632446221,34.5479047591227,173.430684404547));
#44990=CARTESIAN_POINT('Ctrl Pts',(-45.3545001320436,34.5115782752305,173.44173857501));
#44991=CARTESIAN_POINT('Ctrl Pts',(-45.3525468614839,34.5004272150142,173.445131849208));
#44992=CARTESIAN_POINT('Ctrl Pts',(-45.3505863489167,34.4892280661516,173.448330371619));
#44993=CARTESIAN_POINT('Ctrl Pts',(-45.3486204928608,34.4779920738192,173.451332405848));
#44994=CARTESIAN_POINT('Ctrl Pts',(-45.3434524005459,34.4484534687685,173.459224535072));
#44995=CARTESIAN_POINT('Ctrl Pts',(-45.3382520871963,34.4186872945855,173.465756220107));
#44996=CARTESIAN_POINT('Ctrl Pts',(-45.3330182670165,34.3886927955056,173.470935497225));
#44997=CARTESIAN_POINT('Ctrl Pts',(-45.3278822554434,34.3592588277512,173.476017985026));
#44998=CARTESIAN_POINT('Ctrl Pts',(-45.3227138390104,34.3296041551761,173.479798218183));
#44999=CARTESIAN_POINT('Ctrl Pts',(-45.3175108165138,34.2997211452501,173.482235171309));
#45000=CARTESIAN_POINT('Ctrl Pts',(-45.3129287259598,34.2734043923248,173.484381296933));
#45001=CARTESIAN_POINT('Ctrl Pts',(-45.3083197232477,34.2469100985176,173.485485069079));
#45002=CARTESIAN_POINT('Ctrl Pts',(-45.3036829175493,34.2202360714903,173.485485069079));
#45003=CARTESIAN_POINT('Origin',(-51.7918181085456,40.3156359630969,172.485485069079));
#45004=CARTESIAN_POINT('Origin',(54.4964231308939,46.060372587574,172.485485069079));
#45005=CARTESIAN_POINT('Origin',(-55.2932569457149,10.3110887801052,178.485485069079));
#45006=CARTESIAN_POINT('Origin',(-55.2932569457149,10.3110887801052,177.985485069079));
#45007=CARTESIAN_POINT('Origin',(-55.2932569457149,10.3110887801052,177.185485069079));
#45008=CARTESIAN_POINT('Origin',(-51.5511046852341,5.7956973373016,177.185485069079));
#45009=CARTESIAN_POINT('',(-51.5511046852341,5.7956973373016,174.785485069079));
#45010=CARTESIAN_POINT('',(-51.5511046852341,5.7956973373016,174.785485069079));
#45011=CARTESIAN_POINT('',(-51.5511046852341,5.7956973373016,177.185485069079));
#45012=CARTESIAN_POINT('',(-51.5511046852341,5.7956973373016,177.185485069079));
#45013=CARTESIAN_POINT('',(-51.5511046852341,5.7956973373016,177.185485069079));
#45014=CARTESIAN_POINT('Origin',(-55.2165279528263,6.30034797823479,177.185485069079));
#45015=CARTESIAN_POINT('',(-57.9855837402625,3.84630436695446,177.185485069079));
#45016=CARTESIAN_POINT('',(-63.4605999891139,10.0241185510634,177.185485069079));
#45017=CARTESIAN_POINT('Origin',(-55.2165279528263,6.30034797823479,177.185485069079));
#45018=CARTESIAN_POINT('Origin',(-55.2165279528263,6.30034797823479,174.785485069079));
#45019=CARTESIAN_POINT('',(-57.9855837402625,3.84630436695446,174.785485069079));
#45020=CARTESIAN_POINT('Origin',(-55.2165279528263,6.30034797823479,174.785485069079));
#45021=CARTESIAN_POINT('',(-63.4605999891139,10.0241185510634,174.785485069079));
#45022=CARTESIAN_POINT('Origin',(-55.2165279528263,6.30034797823479,177.185485069079));
#45023=CARTESIAN_POINT('',(-57.9855837402625,3.84630436695446,177.185485069079));
#45024=CARTESIAN_POINT('Origin',(-63.4605999891139,10.0241185510634,177.185485069079));
#45025=CARTESIAN_POINT('Origin',(-43.5924087366602,55.5662189415684,171.985485069079));
#45026=CARTESIAN_POINT('',(-44.949586852714,57.3017198020218,171.985485069079));
#45027=CARTESIAN_POINT('',(-45.7483677109949,58.3231663243772,171.985485069079));
#45028=CARTESIAN_POINT('Origin',(-44.6376627105729,59.1917481581946,171.985485069079));
#45029=CARTESIAN_POINT('Origin',(-44.8222909569807,57.4012663985631,171.985485069079));
#45030=CARTESIAN_POINT('',(-45.9329959574027,56.5326845647457,171.985485069079));
#45031=CARTESIAN_POINT('Origin',(-44.9746623630668,55.6077515601656,171.985485069079));
#45032=CARTESIAN_POINT('',(-46.0853673634888,54.7391697263481,171.985485069079));
#45033=CARTESIAN_POINT('',(-45.1205026113461,55.4937031042329,171.985485069079));
#45034=CARTESIAN_POINT('Origin',(-45.0947275618286,53.8117847261202,171.985485069079));
#45035=CARTESIAN_POINT('',(-46.2054325622506,52.9432028923028,171.985485069079));
#45036=CARTESIAN_POINT('',(-45.2594247703932,53.6829899485823,171.985485069079));
#45037=CARTESIAN_POINT('Origin',(-45.182447653192,52.0139477739702,171.985485069079));
#45038=CARTESIAN_POINT('',(-46.293152653614,51.1453659401528,171.985485069079));
#45039=CARTESIAN_POINT('',(-45.3663083202907,51.8701669902924,171.985485069079));
#45040=CARTESIAN_POINT('Origin',(-45.2377942166148,50.2148231871608,171.985485069079));
#45041=CARTESIAN_POINT('',(-46.3484992170368,49.3462413533434,171.985485069079));
#45042=CARTESIAN_POINT('',(-45.4411186317038,50.0558215681434,171.985485069079));
#45043=CARTESIAN_POINT('Origin',(-45.2607493202947,48.4149938663196,171.985485069079));
#45044=CARTESIAN_POINT('',(-46.3714543207166,47.5464120325021,171.985485069079));
#45045=CARTESIAN_POINT('',(-45.4838314667458,48.2405415141803,171.985485069079));
#45046=CARTESIAN_POINT('Origin',(-44.2154953463819,44.7894646496933,171.985485069079));
#45047=CARTESIAN_POINT('Origin',(-44.1925402427021,46.5892939705346,171.985485069079));
#45048=CARTESIAN_POINT('Origin',(-44.1371936792793,48.388418557344,171.985485069079));
#45049=CARTESIAN_POINT('Origin',(-44.0494735879158,50.186255509494,171.985485069079));
#45050=CARTESIAN_POINT('Origin',(-43.9294083891541,51.9822223435394,171.985485069079));
#45051=CARTESIAN_POINT('Origin',(-43.777036983068,53.7757371819369,171.985485069079));
#45052=CARTESIAN_POINT('Origin',(-45.2094658963734,44.8155535777614,171.985485069079));
#45053=CARTESIAN_POINT('',(-46.3201708967954,43.9469717439439,171.985485069079));
#45054=CARTESIAN_POINT('Origin',(-44.1642119224607,41.1900243611352,171.985485069079));
#45055=CARTESIAN_POINT('Origin',(-44.206051553066,42.9895137237755,171.985485069079));
#45056=CARTESIAN_POINT('',(-46.3620105274007,45.7464611065843,171.985485069079));
#45057=CARTESIAN_POINT('Origin',(-45.2513055269787,46.6150429404017,171.985485069079));
#45058=CARTESIAN_POINT('Origin',(-37.6267629804773,17.3035841126903,173.985485069079));
#45059=CARTESIAN_POINT('Origin',(-39.8623336503921,1.96564996953346,173.985485069079));
#45060=CARTESIAN_POINT('Origin',(-52.0389027942237,11.5991800255814,173.985485069079));
#45061=CARTESIAN_POINT('Origin',(-55.2932569457149,10.3110887801052,173.985485069079));
#45062=CARTESIAN_POINT('Origin',(-56.6916004724222,13.5196142017461,173.985485069079));
#45063=CARTESIAN_POINT('Origin',(-67.58190263219,8.77338921431569,173.985485069079));
#45064=CARTESIAN_POINT('Origin',(-94.0351308638859,47.8471884530858,173.985485069079));
#45065=CARTESIAN_POINT('Origin',(-58.9792278552929,42.2495403530246,173.985485069079));
#45066=CARTESIAN_POINT('Origin',(-31.8232466514532,37.9133340783293,173.985485069079));
#45067=CARTESIAN_POINT('Origin',(-51.2438457370578,57.3835762739523,173.985485069079));
#45068=CARTESIAN_POINT('Ctrl Pts',(-49.676843289894,59.3614282330636,172.857169043842));
#45069=CARTESIAN_POINT('Ctrl Pts',(-49.6580501443528,59.498785825288,172.940667815898));
#45070=CARTESIAN_POINT('Ctrl Pts',(-49.5614006736427,59.5779430613272,173.043611870202));
#45071=CARTESIAN_POINT('Ctrl Pts',(-49.8129218697063,59.2066852860614,173.020976119607));
#45072=CARTESIAN_POINT('Ctrl Pts',(-49.8268191099127,59.3595810228937,173.140746393147));
#45073=CARTESIAN_POINT('Ctrl Pts',(-49.7298982507317,59.4401605537898,173.288593641521));
#45074=CARTESIAN_POINT('Ctrl Pts',(-49.9751587473744,59.0175746776917,173.132009583873));
#45075=CARTESIAN_POINT('Ctrl Pts',(-50.0283787246662,59.1891576068682,173.26617245629));
#45076=CARTESIAN_POINT('Ctrl Pts',(-49.9342084666479,59.2692635558937,173.455528336301));
#45077=CARTESIAN_POINT('Ctrl Pts',(-50.2670349607775,58.6648561595715,173.282713630629));
#45078=CARTESIAN_POINT('Ctrl Pts',(-50.3867087288933,58.8763902547733,173.422336146559));
#45079=CARTESIAN_POINT('Ctrl Pts',(-50.3068160600608,58.946637106271,173.681583012477));
#45080=CARTESIAN_POINT('Ctrl Pts',(-50.3913565197452,58.5110970032596,173.331875725947));
#45081=CARTESIAN_POINT('Ctrl Pts',(-50.5416645611132,58.7381013798362,173.467425863685));
#45082=CARTESIAN_POINT('Ctrl Pts',(-50.4671147462085,58.8047920444951,173.755313568593));
#45083=CARTESIAN_POINT('Ctrl Pts',(-50.8097833774366,57.9804901848007,173.46326053759));
#45084=CARTESIAN_POINT('Ctrl Pts',(-51.0806778350923,58.2463716358246,173.571501704738));
#45085=CARTESIAN_POINT('Ctrl Pts',(-51.0122898852652,58.3106471527106,173.952327305448));
#45086=CARTESIAN_POINT('Ctrl Pts',(-51.1047582211487,57.5839691659291,173.498876066328));
#45087=CARTESIAN_POINT('Ctrl Pts',(-51.4575793662449,57.881015208655,173.541235698465));
#45088=CARTESIAN_POINT('Ctrl Pts',(-51.4062439592343,57.9336438396564,174.005637220798));
#45089=CARTESIAN_POINT('Ctrl Pts',(-51.3846028209176,57.183358971478,173.481037601188));
#45090=CARTESIAN_POINT('Ctrl Pts',(-51.7691525391572,57.5641765559212,173.436036324449));
#45091=CARTESIAN_POINT('Ctrl Pts',(-51.7892845019502,57.5437998061236,173.978750519954));
#45092=CARTESIAN_POINT('Origin',(-49.394587641375,59.0674820360207,173.235485069079));
#45093=CARTESIAN_POINT('Ctrl Pts',(-49.7140665684645,59.4521029079787,173.235485069079));
#45094=CARTESIAN_POINT('Ctrl Pts',(-49.8076683737025,59.3743541260188,173.092919514947));
#45095=CARTESIAN_POINT('Ctrl Pts',(-49.7994785223376,59.2209856988867,172.985485069079));
#45096=CARTESIAN_POINT('Ctrl Pts',(-49.3244877069872,59.7757001065599,172.810949602497));
#45097=CARTESIAN_POINT('Ctrl Pts',(-49.4175936181462,59.7012196303848,172.669550113054));
#45098=CARTESIAN_POINT('Ctrl Pts',(-49.4120033989242,59.551605021816,172.560949601135));
#45099=CARTESIAN_POINT('Ctrl Pts',(-48.9215898703068,60.0925595649752,172.396514721378));
#45100=CARTESIAN_POINT('Ctrl Pts',(-49.0132975775448,60.0219725953743,172.255650553252));
#45101=CARTESIAN_POINT('Ctrl Pts',(-49.0106022401066,59.8760222809677,172.146514351631));
#45102=CARTESIAN_POINT('Ctrl Pts',(-48.5031673671099,60.4028926537974,171.994932980254));
#45103=CARTESIAN_POINT('Ctrl Pts',(-48.5921091241355,60.3369268656953,171.853849669263));
#45104=CARTESIAN_POINT('Ctrl Pts',(-48.5928620772033,60.1944375331114,171.744932980254));
#45105=CARTESIAN_POINT('Origin',(-37.6267629804773,17.3035841126903,177.985485069079));
#45106=CARTESIAN_POINT('Origin',(-39.8623336503921,1.96564996953346,177.985485069079));
#45107=CARTESIAN_POINT('Origin',(-52.0389027942237,11.5991800255814,177.985485069079));
#45108=CARTESIAN_POINT('Origin',(-55.2932569457149,10.3110887801052,177.985485069079));
#45109=CARTESIAN_POINT('Origin',(-56.6916004724222,13.5196142017461,177.985485069079));
#45110=CARTESIAN_POINT('Origin',(-67.58190263219,8.77338921431569,177.985485069079));
#45111=CARTESIAN_POINT('Origin',(-94.0351308638859,47.8471884530858,177.985485069079));
#45112=CARTESIAN_POINT('Origin',(-58.9792278552929,42.2495403530246,177.985485069079));
#45113=CARTESIAN_POINT('Origin',(-31.8232466514532,37.9133340783293,177.985485069079));
#45114=CARTESIAN_POINT('Origin',(-51.243845737057,57.3835762739531,177.985485069079));
#45115=CARTESIAN_POINT('Ctrl Pts',(-51.3851747440281,57.1830027074348,178.489845032705));
#45116=CARTESIAN_POINT('Ctrl Pts',(-51.7698287477023,57.5635493714596,178.53459520218));
#45117=CARTESIAN_POINT('Ctrl Pts',(-51.789795174837,57.5433312673965,177.992059147256));
#45118=CARTESIAN_POINT('Ctrl Pts',(-51.1036551824481,57.5857370375821,178.47242911223));
#45119=CARTESIAN_POINT('Ctrl Pts',(-51.4556422663022,57.882802074248,178.429816451876));
#45120=CARTESIAN_POINT('Ctrl Pts',(-51.4046161396593,57.9351319791878,177.965865526389));
#45121=CARTESIAN_POINT('Ctrl Pts',(-50.812871026537,57.9768655506053,178.506778396529));
#45122=CARTESIAN_POINT('Ctrl Pts',(-51.0847171506893,58.2426715965213,178.398610314328));
#45123=CARTESIAN_POINT('Ctrl Pts',(-51.0161416619809,58.3071396903623,178.017328502921));
#45124=CARTESIAN_POINT('Ctrl Pts',(-50.39072672801,58.5121320105389,178.639222923132));
#45125=CARTESIAN_POINT('Ctrl Pts',(-50.5408096374063,58.7388868900845,178.503564579484));
#45126=CARTESIAN_POINT('Ctrl Pts',(-50.4661837565912,58.8056426366741,178.215960736115));
#45127=CARTESIAN_POINT('Ctrl Pts',(-50.2654292154088,58.6670064325193,178.688993669122));
#45128=CARTESIAN_POINT('Ctrl Pts',(-50.384555500579,58.8782789036964,178.549394330658));
#45129=CARTESIAN_POINT('Ctrl Pts',(-50.3046760179673,58.9484994170746,178.29061015284));
#45130=CARTESIAN_POINT('Ctrl Pts',(-49.9761487934086,59.0165015159078,178.838454681089));
#45131=CARTESIAN_POINT('Ctrl Pts',(-50.0294357633358,59.1882221141344,178.704350540701));
#45132=CARTESIAN_POINT('Ctrl Pts',(-49.9354391713799,59.2681848187678,178.514801007031));
#45133=CARTESIAN_POINT('Ctrl Pts',(-49.8137887158582,59.2058315816185,178.948821207635));
#45134=CARTESIAN_POINT('Ctrl Pts',(-49.8279315490083,59.358683921035,178.828773746461));
#45135=CARTESIAN_POINT('Ctrl Pts',(-49.7309210947959,59.4393519811699,178.680758434674));
#45136=CARTESIAN_POINT('Ctrl Pts',(-49.6753781533107,59.3631653373938,179.115257436673));
#45137=CARTESIAN_POINT('Ctrl Pts',(-49.6562522395083,59.5002721847792,179.032027213671));
#45138=CARTESIAN_POINT('Ctrl Pts',(-49.5596295986081,59.5793903823432,178.92957895201));
#45139=CARTESIAN_POINT('Origin',(-49.3945876413725,59.0674820360227,178.735485069082));
#45140=CARTESIAN_POINT('Ctrl Pts',(-49.7994785223352,59.2209856988888,178.985485069082));
#45141=CARTESIAN_POINT('Ctrl Pts',(-49.8076683737,59.3743541260209,178.878050623215));
#45142=CARTESIAN_POINT('Ctrl Pts',(-49.714066568462,59.4521029079807,178.735485069082));
#45143=CARTESIAN_POINT('Ctrl Pts',(-49.412003398922,59.5516050218084,179.410020537031));
#45144=CARTESIAN_POINT('Ctrl Pts',(-49.4175936181378,59.7012196303778,179.301420025102));
#45145=CARTESIAN_POINT('Ctrl Pts',(-49.3244877069919,59.775700106556,179.16002053567));
#45146=CARTESIAN_POINT('Ctrl Pts',(-49.0106022401058,59.8760222809537,179.824455786539));
#45147=CARTESIAN_POINT('Ctrl Pts',(-49.0132975775679,60.0219725953311,179.715319584971));
#45148=CARTESIAN_POINT('Ctrl Pts',(-48.9215898703156,60.0925595649687,179.5744554168));
#45149=CARTESIAN_POINT('Ctrl Pts',(-48.5928620772034,60.1944375331114,180.226037157904));
#45150=CARTESIAN_POINT('Ctrl Pts',(-48.5921091241356,60.3369268656953,180.117120468896));
#45151=CARTESIAN_POINT('Ctrl Pts',(-48.5031673671099,60.4028926537974,179.976037157904));
#45152=CARTESIAN_POINT('Ctrl Pts',(-45.4569991048231,35.0869155900178,172.985485069079));
#45153=CARTESIAN_POINT('Ctrl Pts',(-44.9016339249302,35.0941792779979,172.955802932359));
#45154=CARTESIAN_POINT('Ctrl Pts',(-44.9520576904499,35.5723002038223,173.235485069079));
#45155=CARTESIAN_POINT('Ctrl Pts',(-45.4850941496413,35.3295082190528,172.566233948071));
#45156=CARTESIAN_POINT('Ctrl Pts',(-44.9281468509024,35.3344337427825,172.534956661662));
#45157=CARTESIAN_POINT('Ctrl Pts',(-44.9775100896269,35.8136412566676,172.81623419061));
#45158=CARTESIAN_POINT('Ctrl Pts',(-45.5125916761024,35.5723252360281,172.14705466709));
#45159=CARTESIAN_POINT('Ctrl Pts',(-44.9537495963942,35.5744329169919,172.114352981929));
#45160=CARTESIAN_POINT('Ctrl Pts',(-45.0020952646643,36.0551804790105,172.397054925059));
#45161=CARTESIAN_POINT('Ctrl Pts',(-45.5396570323393,35.815459379751,171.727986820601));
#45162=CARTESIAN_POINT('Ctrl Pts',(-44.9783867312583,35.8135096162751,171.694926243495));
#45163=CARTESIAN_POINT('Ctrl Pts',(-45.0258168897239,36.2969847903722,171.977986820601));
#45164=CARTESIAN_POINT('Origin',(-45.4493000945566,35.5198598419035,173.235485069079));
#45165=CARTESIAN_POINT('Ctrl Pts',(-45.3036829175493,34.2202360714903,173.485485069079));
#45166=CARTESIAN_POINT('Ctrl Pts',(-44.8071649770098,34.2791422233116,173.485485069079));
#45167=CARTESIAN_POINT('Ctrl Pts',(-44.8071649770098,34.2791422233116,173.985485069079));
#45168=CARTESIAN_POINT('Ctrl Pts',(-45.3338963953346,34.3940443299001,173.485485069079));
#45169=CARTESIAN_POINT('Ctrl Pts',(-44.8279831491234,34.4546178863727,173.475857632828));
#45170=CARTESIAN_POINT('Ctrl Pts',(-44.8379572766539,34.538689464662,173.985485049617));
#45171=CARTESIAN_POINT('Ctrl Pts',(-45.3644831092931,34.5691582546223,173.438504175172));
#45172=CARTESIAN_POINT('Ctrl Pts',(-44.84765733035,34.6236472660135,173.417377867645));
#45173=CARTESIAN_POINT('Ctrl Pts',(-44.8678394640859,34.800067602205,173.915013729195));
#45174=CARTESIAN_POINT('Ctrl Pts',(-45.4044745628099,34.7951467101956,173.308260039551));
#45175=CARTESIAN_POINT('Ctrl Pts',(-44.8718806226984,34.8337506678808,173.278188236865));
#45176=CARTESIAN_POINT('Ctrl Pts',(-44.9052767643286,35.1372390952084,173.719647524298));
#45177=CARTESIAN_POINT('Ctrl Pts',(-45.417105936473,34.8659857778945,173.254031151206));
#45178=CARTESIAN_POINT('Ctrl Pts',(-44.8792949307336,34.898439442477,173.2217377076));
#45179=CARTESIAN_POINT('Ctrl Pts',(-44.9168097068416,35.2429009650579,173.638304190863));
#45180=CARTESIAN_POINT('Ctrl Pts',(-45.4392598534242,34.9893244322491,173.130935739704));
#45181=CARTESIAN_POINT('Ctrl Pts',(-44.8919644948922,35.0092694227254,173.097445835965));
#45182=CARTESIAN_POINT('Ctrl Pts',(-44.9366510910588,35.4268263152626,173.453661076422));
#45183=CARTESIAN_POINT('Ctrl Pts',(-45.4489103970047,35.042562611079,173.062045438043));
#45184=CARTESIAN_POINT('Ctrl Pts',(-44.8972783322719,35.0559155097348,173.029495931902));
#45185=CARTESIAN_POINT('Ctrl Pts',(-44.9450858967755,35.5061932716661,173.35032414664));
#45186=CARTESIAN_POINT('Ctrl Pts',(-45.4569991048231,35.0869155900178,172.985485069079));
#45187=CARTESIAN_POINT('Ctrl Pts',(-44.9016339249302,35.0941792779979,172.955802932359));
#45188=CARTESIAN_POINT('Ctrl Pts',(-44.9520576904499,35.5723002038223,173.235485069079));
#45189=CARTESIAN_POINT('Origin',(-45.3036829175493,34.2202360714903,173.985485069079));
#45190=CARTESIAN_POINT('Origin',(54.4964231308939,46.060372587574,173.985485069079));
#45191=CARTESIAN_POINT('Origin',(-43.2773451499467,22.8108513846653,173.985485069079));
#45192=CARTESIAN_POINT('Origin',(-31.1164286971058,25.7025828775644,173.985485069079));
#45193=CARTESIAN_POINT('Origin',(-36.2883138077383,14.3227057076466,173.985485069079));
#45194=CARTESIAN_POINT('Origin',(-38.9776940652673,8.40516957928931,173.985485069079));
#45195=CARTESIAN_POINT('Origin',(-39.8623336503921,1.96564996953346,173.985485069079));
#45196=CARTESIAN_POINT('Origin',(-39.8623336503921,1.96564996953345,173.985485069079));
#45197=CARTESIAN_POINT('Origin',(-39.8623336503921,1.96564996953346,173.985485069079));
#45198=CARTESIAN_POINT('Origin',(-39.8623336503921,1.96564996953346,178.485485069079));
#45199=CARTESIAN_POINT('Origin',(-39.8623336503921,1.96564996953346,177.985485069079));
#45200=CARTESIAN_POINT('Origin',(-39.8623336503921,1.96564996953345,177.985485069079));
#45201=CARTESIAN_POINT('Origin',(-39.8623336503921,1.96564996953346,177.985485069079));
#45202=CARTESIAN_POINT('Origin',(-38.9776940652673,8.40516957928931,177.985485069079));
#45203=CARTESIAN_POINT('Origin',(-36.2883138077383,14.3227057076466,177.985485069079));
#45204=CARTESIAN_POINT('Origin',(-31.1164286971058,25.7025828775644,177.985485069079));
#45205=CARTESIAN_POINT('Origin',(-43.2773451499467,22.8108513846653,177.985485069079));
#45206=CARTESIAN_POINT('Origin',(54.4964231308939,46.060372587574,177.985485069079));
#45207=CARTESIAN_POINT('Origin',(-45.3036829175493,34.2202360714903,177.985485069079));
#45208=CARTESIAN_POINT('Ctrl Pts',(-45.4569991048231,35.0869155900178,178.985485069079));
#45209=CARTESIAN_POINT('Ctrl Pts',(-44.9016339249302,35.0941792779979,179.0151672058));
#45210=CARTESIAN_POINT('Ctrl Pts',(-44.9520576904499,35.5723002038223,178.735485069079));
#45211=CARTESIAN_POINT('Ctrl Pts',(-45.4410006746859,34.9991910657925,178.83405844334));
#45212=CARTESIAN_POINT('Ctrl Pts',(-44.8930599489135,35.0188571214058,178.870102671035));
#45213=CARTESIAN_POINT('Ctrl Pts',(-44.9382677607559,35.4415433298683,178.508337952365));
#45214=CARTESIAN_POINT('Ctrl Pts',(-45.4177353589643,34.8700866935674,178.705789670185));
#45215=CARTESIAN_POINT('Ctrl Pts',(-44.8800761442588,34.9048322093886,178.739759632446));
#45216=CARTESIAN_POINT('Ctrl Pts',(-44.9176930036587,35.2490486968859,178.315941970112));
#45217=CARTESIAN_POINT('Ctrl Pts',(-45.3777210193303,34.6439624480249,178.575633526873));
#45218=CARTESIAN_POINT('Ctrl Pts',(-44.8555949763002,34.6924969087779,178.599259564719));
#45219=CARTESIAN_POINT('Ctrl Pts',(-44.8802307081201,34.9116742540591,178.120707756082));
#45220=CARTESIAN_POINT('Ctrl Pts',(-45.3632480720711,34.5616383925205,178.541657619885));
#45221=CARTESIAN_POINT('Ctrl Pts',(-44.8465284950399,34.6142452624173,178.560861887554));
#45222=CARTESIAN_POINT('Ctrl Pts',(-44.8663865052777,34.7888188171875,178.069743897378));
#45223=CARTESIAN_POINT('Ctrl Pts',(-45.3339158795757,34.3939812335556,178.496912907544));
#45224=CARTESIAN_POINT('Ctrl Pts',(-44.8275659262796,34.4518581195231,178.506832300477));
#45225=CARTESIAN_POINT('Ctrl Pts',(-44.8376784522628,34.5385617116783,178.002626824687));
#45226=CARTESIAN_POINT('Ctrl Pts',(-45.3189633638158,34.3081394824255,178.485485069079));
#45227=CARTESIAN_POINT('Ctrl Pts',(-44.8176339640159,34.3673849580269,178.490326489291));
#45228=CARTESIAN_POINT('Ctrl Pts',(-44.8227374568447,34.4104021236386,177.985485079905));
#45229=CARTESIAN_POINT('Ctrl Pts',(-45.3036829175493,34.2202360714903,178.485485069079));
#45230=CARTESIAN_POINT('Ctrl Pts',(-44.8071649770098,34.2791422233116,178.485485069079));
#45231=CARTESIAN_POINT('Ctrl Pts',(-44.8071649770098,34.2791422233116,177.985485069079));
#45232=CARTESIAN_POINT('Origin',(-45.4493000945566,35.5198598419035,178.735485069079));
#45233=CARTESIAN_POINT('Ctrl Pts',(-44.9520576904499,35.5723002038223,178.735485069079));
#45234=CARTESIAN_POINT('Ctrl Pts',(-44.9016339249302,35.0941792779979,179.0151672058));
#45235=CARTESIAN_POINT('Ctrl Pts',(-45.4569991048231,35.0869155900178,178.985485069079));
#45236=CARTESIAN_POINT('Ctrl Pts',(-44.9775100896269,35.8136412566674,179.154735947548));
#45237=CARTESIAN_POINT('Ctrl Pts',(-44.928146850906,35.334433742785,179.436013476495));
#45238=CARTESIAN_POINT('Ctrl Pts',(-45.4850941496413,35.3295082190525,179.404736190087));
#45239=CARTESIAN_POINT('Ctrl Pts',(-45.0020952646649,36.0551804790164,179.573915213096));
#45240=CARTESIAN_POINT('Ctrl Pts',(-44.9537495963754,35.5744329169963,179.856617156227));
#45241=CARTESIAN_POINT('Ctrl Pts',(-45.5125916761142,35.572325236028,179.823915471068));
#45242=CARTESIAN_POINT('Ctrl Pts',(-45.0258168897239,36.296984790372,179.992983317557));
#45243=CARTESIAN_POINT('Ctrl Pts',(-44.9783867312583,35.8135096162749,180.276043894663));
#45244=CARTESIAN_POINT('Ctrl Pts',(-45.5396570323393,35.8154593797507,180.242983317557));
#45245=CARTESIAN_POINT('',(0.,0.,0.));
#45246=CARTESIAN_POINT('Origin',(-31.229031910667,-116.780702189177,178.985485069079));
#45247=CARTESIAN_POINT('',(-81.9809794708757,-61.5607798889249,178.985485069079));
#45248=CARTESIAN_POINT('',(-104.027257502361,-98.7413465825904,178.985485069079));
#45249=CARTESIAN_POINT('Origin',(-31.229031910667,-116.780702189177,178.985485069079));
#45250=CARTESIAN_POINT('',(-83.2437717586763,-60.6850977397733,180.485485069079));
#45251=CARTESIAN_POINT('Ctrl Pts',(-83.2437717586763,-60.6850977397733,
180.485485069079));
#45252=CARTESIAN_POINT('Ctrl Pts',(-83.2422325967899,-60.6861625729165,
180.485485069079));
#45253=CARTESIAN_POINT('Ctrl Pts',(-83.2406934401744,-60.6872274114438,
180.485481729905));
#45254=CARTESIAN_POINT('Ctrl Pts',(-83.070898721105,-60.8046979074495,180.484744993636));
#45255=CARTESIAN_POINT('Ctrl Pts',(-82.9042059840165,-60.9201343030104,
180.444117117279));
#45256=CARTESIAN_POINT('Ctrl Pts',(-82.5956424548927,-61.1339972589321,
180.288086830727));
#45257=CARTESIAN_POINT('Ctrl Pts',(-82.4561538201594,-61.2307685378217,
180.174971263388));
#45258=CARTESIAN_POINT('Ctrl Pts',(-82.2247684030825,-61.3913855449473,
179.892696719416));
#45259=CARTESIAN_POINT('Ctrl Pts',(-82.1339882775335,-61.4544507205017,
179.72770850648));
#45260=CARTESIAN_POINT('Ctrl Pts',(-82.0121144592395,-61.5391347772565,
179.368058467365));
#45261=CARTESIAN_POINT('Ctrl Pts',(-81.9809990073737,-61.5607663092965,
179.17792947018));
#45262=CARTESIAN_POINT('Ctrl Pts',(-81.9809794739406,-61.5607798867945,
178.985605775658));
#45263=CARTESIAN_POINT('Ctrl Pts',(-81.9809794708757,-61.5607798889249,
178.985545422265));
#45264=CARTESIAN_POINT('Ctrl Pts',(-81.9809794708757,-61.5607798889249,
178.985485069079));
#45265=CARTESIAN_POINT('',(-106.601824441649,-103.696660532197,180.485485069079));
#45266=CARTESIAN_POINT('Origin',(-31.229031910667,-116.780702189177,180.485485069079));
#45267=CARTESIAN_POINT('',(-105.613710699518,-102.630519079741,180.265888107377));
#45268=CARTESIAN_POINT('Ctrl Pts',(-105.613710699518,-102.630519079741,
180.265888107377));
#45269=CARTESIAN_POINT('Ctrl Pts',(-105.658052765278,-102.739223164379,
180.280074653183));
#45270=CARTESIAN_POINT('Ctrl Pts',(-105.708972522035,-102.837432096684,
180.298606216492));
#45271=CARTESIAN_POINT('Ctrl Pts',(-105.889297996009,-103.133428559691,
180.362418620409));
#45272=CARTESIAN_POINT('Ctrl Pts',(-106.053691035723,-103.31971416131,180.41853554034));
#45273=CARTESIAN_POINT('Ctrl Pts',(-106.358503600507,-103.559189420194,
180.472850239938));
#45274=CARTESIAN_POINT('Ctrl Pts',(-106.47665098808,-103.634137304981,180.485485069079));
#45275=CARTESIAN_POINT('Ctrl Pts',(-106.601824441649,-103.696660532197,
180.485485069079));
#45276=CARTESIAN_POINT('Ctrl Pts',(-104.027257502361,-98.7413465825906,
178.985485069079));
#45277=CARTESIAN_POINT('Ctrl Pts',(-104.027257502361,-98.7413465825906,
179.026424101808));
#45278=CARTESIAN_POINT('Ctrl Pts',(-104.032888367115,-98.7551505853665,
179.073234241807));
#45279=CARTESIAN_POINT('Ctrl Pts',(-104.053185991761,-98.8049099880857,
179.167298560279));
#45280=CARTESIAN_POINT('Ctrl Pts',(-104.075243416314,-98.858983520846,179.223244697426));
#45281=CARTESIAN_POINT('Ctrl Pts',(-104.152999108407,-99.0496007415273,
179.382318294648));
#45282=CARTESIAN_POINT('Ctrl Pts',(-104.224794456088,-99.2256062436916,
179.466142077644));
#45283=CARTESIAN_POINT('Ctrl Pts',(-104.37241425056,-99.5874945400008,179.616310592306));
#45284=CARTESIAN_POINT('Ctrl Pts',(-104.448792282881,-99.7747344429623,
179.678812502117));
#45285=CARTESIAN_POINT('Ctrl Pts',(-104.856768027367,-100.774882476199,
179.982161235303));
#45286=CARTESIAN_POINT('Ctrl Pts',(-105.232613956139,-101.696264620951,
180.143962204427));
#45287=CARTESIAN_POINT('Ctrl Pts',(-105.613710699518,-102.630519079741,
180.265888107377));
#45288=CARTESIAN_POINT('Origin',(-31.229031910667,-116.780702189177,172.985485069079));
#45289=CARTESIAN_POINT('',(-83.2437717586763,-60.6850977397733,171.485485069079));
#45290=CARTESIAN_POINT('',(-106.601824441649,-103.696660532197,171.485485069079));
#45291=CARTESIAN_POINT('Origin',(-31.229031910667,-116.780702189177,171.485485069079));
#45292=CARTESIAN_POINT('',(-81.9809794708757,-61.5607798889249,172.985485069079));
#45293=CARTESIAN_POINT('Ctrl Pts',(-81.9809794708757,-61.5607798889249,
172.985485069079));
#45294=CARTESIAN_POINT('Ctrl Pts',(-81.9809794708757,-61.5607798889249,
172.794647159443));
#45295=CARTESIAN_POINT('Ctrl Pts',(-82.0116164204235,-61.5394810565551,
172.605891278582));
#45296=CARTESIAN_POINT('Ctrl Pts',(-82.1311013468671,-61.4564564904976,
172.250286109186));
#45297=CARTESIAN_POINT('Ctrl Pts',(-82.2194216547433,-61.3950995397068,
172.08752918528));
#45298=CARTESIAN_POINT('Ctrl Pts',(-82.4445214808283,-61.2388407613391,
171.807588409535));
#45299=CARTESIAN_POINT('Ctrl Pts',(-82.5802654678823,-61.1446627802494,
171.694380155136));
#45300=CARTESIAN_POINT('Ctrl Pts',(-82.809839687611,-60.9855353654994,171.572921494192));
#45301=CARTESIAN_POINT('Ctrl Pts',(-82.8932820097023,-60.927723055843,171.540639437838));
#45302=CARTESIAN_POINT('Ctrl Pts',(-83.0643730653962,-60.8092421044008,
171.497047848165));
#45303=CARTESIAN_POINT('Ctrl Pts',(-83.1516444302605,-60.7488349303393,
171.485874790325));
#45304=CARTESIAN_POINT('Ctrl Pts',(-83.2406934401744,-60.6872274114439,
171.485488408253));
#45305=CARTESIAN_POINT('Ctrl Pts',(-83.2422325967899,-60.6861625729165,
171.485485069079));
#45306=CARTESIAN_POINT('Ctrl Pts',(-83.2437717586764,-60.6850977397733,
171.485485069079));
#45307=CARTESIAN_POINT('',(-104.027257502361,-98.7413465825904,172.985485069079));
#45308=CARTESIAN_POINT('Origin',(-31.229031910667,-116.780702189177,172.985485069079));
#45309=CARTESIAN_POINT('',(-105.613710699519,-102.630519079742,171.705082030781));
#45310=CARTESIAN_POINT('Ctrl Pts',(-105.613710699519,-102.630519079742,
171.705082030781));
#45311=CARTESIAN_POINT('Ctrl Pts',(-105.232613956139,-101.696264620952,
171.827007933732));
#45312=CARTESIAN_POINT('Ctrl Pts',(-104.856768027367,-100.7748824762,171.988808902855));
#45313=CARTESIAN_POINT('Ctrl Pts',(-104.448792282881,-99.7747344429622,
172.292157636041));
#45314=CARTESIAN_POINT('Ctrl Pts',(-104.37241425056,-99.5874945400007,172.354659545853));
#45315=CARTESIAN_POINT('Ctrl Pts',(-104.224794456088,-99.2256062436915,
172.504828060515));
#45316=CARTESIAN_POINT('Ctrl Pts',(-104.152999108407,-99.0496007415272,
172.58865184351));
#45317=CARTESIAN_POINT('Ctrl Pts',(-104.075243416314,-98.8589835208459,
172.747725440733));
#45318=CARTESIAN_POINT('Ctrl Pts',(-104.053185991761,-98.8049099880857,
172.803671577879));
#45319=CARTESIAN_POINT('Ctrl Pts',(-104.032888367115,-98.7551505853665,
172.897735896352));
#45320=CARTESIAN_POINT('Ctrl Pts',(-104.027257502361,-98.7413465825906,
172.94454603635));
#45321=CARTESIAN_POINT('Ctrl Pts',(-104.027257502361,-98.7413465825906,
172.985485069079));
#45322=CARTESIAN_POINT('Ctrl Pts',(-106.601824441649,-103.696660532197,
171.485485069079));
#45323=CARTESIAN_POINT('Ctrl Pts',(-106.53220525908,-103.66188625821,171.485485069079));
#45324=CARTESIAN_POINT('Ctrl Pts',(-106.464169344039,-103.622977573215,
171.489410638421));
#45325=CARTESIAN_POINT('Ctrl Pts',(-106.211695162338,-103.458610972797,
171.516115265147));
#45326=CARTESIAN_POINT('Ctrl Pts',(-106.046375023087,-103.308026666015,
171.559682835566));
#45327=CARTESIAN_POINT('Ctrl Pts',(-105.804368479235,-103.003327965471,
171.637167539166));
#45328=CARTESIAN_POINT('Ctrl Pts',(-105.715452773286,-102.858679667203,
171.670867024465));
#45329=CARTESIAN_POINT('Ctrl Pts',(-105.634000122074,-102.67893082039,171.698474541123));
#45330=CARTESIAN_POINT('Ctrl Pts',(-105.623629484128,-102.654834870701,
171.701908671809));
#45331=CARTESIAN_POINT('Ctrl Pts',(-105.613710699519,-102.630519079742,
171.705082030781));
#45332=CARTESIAN_POINT('Origin',(106.899307254449,-150.793932399799,177.485485069079));
#45333=CARTESIAN_POINT('',(-91.410849784583,-57.8787323612094,180.485485069079));
#45334=CARTESIAN_POINT('',(-107.009977058815,-103.84909152684,180.485485069079));
#45335=CARTESIAN_POINT('Origin',(106.899307254449,-150.793932399799,180.485485069079));
#45336=CARTESIAN_POINT('',(-94.1292986217245,-56.6052939157322,177.485485069079));
#45337=CARTESIAN_POINT('Ctrl Pts',(-94.1292986217245,-56.6052939157322,
177.485485069079));
#45338=CARTESIAN_POINT('Ctrl Pts',(-94.1292986217245,-56.6052939157322,
177.856763201439));
#45339=CARTESIAN_POINT('Ctrl Pts',(-94.0660385633859,-56.6351180251081,
178.239317280815));
#45340=CARTESIAN_POINT('Ctrl Pts',(-93.8670456578475,-56.7283483675185,
178.785738776833));
#45341=CARTESIAN_POINT('Ctrl Pts',(-93.7835242707107,-56.7674422240991,
178.963188566011));
#45342=CARTESIAN_POINT('Ctrl Pts',(-93.6330340156095,-56.8378730704672,
179.215996936763));
#45343=CARTESIAN_POINT('Ctrl Pts',(-93.5786828002802,-56.8633094959559,
179.298034924651));
#45344=CARTESIAN_POINT('Ctrl Pts',(-93.491075623674,-56.9043212188128,179.416933247598));
#45345=CARTESIAN_POINT('Ctrl Pts',(-93.4457533491126,-56.9255407794407,
179.475342645356));
#45346=CARTESIAN_POINT('Ctrl Pts',(-93.3902788233905,-56.9515217739284,
179.541489655834));
#45347=CARTESIAN_POINT('Ctrl Pts',(-93.3619004743536,-56.96481499421,179.574041689426));
#45348=CARTESIAN_POINT('Ctrl Pts',(-93.3475521299737,-56.9715368357171,
179.590184575139));
#45349=CARTESIAN_POINT('Ctrl Pts',(-93.3413688531149,-56.9744336964136,
179.597074130901));
#45350=CARTESIAN_POINT('Ctrl Pts',(-93.3372391296956,-56.9763685027338,
179.601660729943));
#45351=CARTESIAN_POINT('Ctrl Pts',(-93.3344333984817,-56.977683037912,179.604764185584));
#45352=CARTESIAN_POINT('Ctrl Pts',(-93.1621805239265,-57.0583876466175,
179.794841788008));
#45353=CARTESIAN_POINT('Ctrl Pts',(-92.9270395815964,-57.1691883844647,
180.005835194439));
#45354=CARTESIAN_POINT('Ctrl Pts',(-92.4482315155942,-57.3936123286524,
180.265019693198));
#45355=CARTESIAN_POINT('Ctrl Pts',(-92.2678586301383,-57.4780238050178,
180.341232854623));
#45356=CARTESIAN_POINT('Ctrl Pts',(-91.8674994509229,-57.6652677007972,
180.451346123991));
#45357=CARTESIAN_POINT('Ctrl Pts',(-91.6474047383563,-57.7681443459078,
180.485147996224));
#45358=CARTESIAN_POINT('Ctrl Pts',(-91.4113312145148,-57.878670006244,180.485485069079));
#45359=CARTESIAN_POINT('',(-109.534287722621,-101.392525888427,177.485485069079));
#45360=CARTESIAN_POINT('Origin',(106.899307254449,-150.793932399799,177.485485069079));
#45361=CARTESIAN_POINT('Ctrl Pts',(-107.009977058815,-103.84909152684,180.485485069079));
#45362=CARTESIAN_POINT('Ctrl Pts',(-107.137921837196,-103.881980428467,
180.485485069079));
#45363=CARTESIAN_POINT('Ctrl Pts',(-107.268759891508,-103.902517901244,
180.478513657667));
#45364=CARTESIAN_POINT('Ctrl Pts',(-107.618867465629,-103.923371702875,
180.436712848229));
#45365=CARTESIAN_POINT('Ctrl Pts',(-107.831376286747,-103.901466369003,
180.387630831655));
#45366=CARTESIAN_POINT('Ctrl Pts',(-108.256149207338,-103.793261446598,
180.232967049603));
#45367=CARTESIAN_POINT('Ctrl Pts',(-108.457219871836,-103.702395545817,
180.124910466337));
#45368=CARTESIAN_POINT('Ctrl Pts',(-108.86130608821,-103.444418866416,179.830873029469));
#45369=CARTESIAN_POINT('Ctrl Pts',(-109.044027201329,-103.26519727749,179.634119786442));
#45370=CARTESIAN_POINT('Ctrl Pts',(-109.370932552757,-102.820739354799,
179.1432271976));
#45371=CARTESIAN_POINT('Ctrl Pts',(-109.48673079434,-102.54337787575,178.835080933563));
#45372=CARTESIAN_POINT('Ctrl Pts',(-109.603841517271,-101.97541853432,178.18613896477));
#45373=CARTESIAN_POINT('Ctrl Pts',(-109.598798782044,-101.679242827835,
177.838268930735));
#45374=CARTESIAN_POINT('Ctrl Pts',(-109.535241658531,-101.396720316011,
177.490648716974));
#45375=CARTESIAN_POINT('Ctrl Pts',(-109.534766330367,-101.39462272741,177.488066892411));
#45376=CARTESIAN_POINT('Ctrl Pts',(-109.534287722621,-101.392525888427,
177.485485069079));
#45377=CARTESIAN_POINT('Origin',(106.899307254449,-150.793932399799,174.485485069079));
#45378=CARTESIAN_POINT('',(-94.1292986217245,-56.6052939157322,174.485485069079));
#45379=CARTESIAN_POINT('',(-109.534287722621,-101.392525888427,174.485485069079));
#45380=CARTESIAN_POINT('Origin',(106.899307254449,-150.793932399799,174.485485069079));
#45381=CARTESIAN_POINT('',(-91.4108060345764,-57.8786324516506,171.485485069079));
#45382=CARTESIAN_POINT('Ctrl Pts',(-91.410862632993,-57.8787562475091,171.485488161254));
#45383=CARTESIAN_POINT('Ctrl Pts',(-91.6484623587964,-57.7676500200356,
171.485988398864));
#45384=CARTESIAN_POINT('Ctrl Pts',(-91.8679492309091,-57.6650573954028,
171.519752422514));
#45385=CARTESIAN_POINT('Ctrl Pts',(-92.2677947733545,-57.4780539094026,
171.629714980247));
#45386=CARTESIAN_POINT('Ctrl Pts',(-92.4481639960319,-57.3936442958883,
171.705919699708));
#45387=CARTESIAN_POINT('Ctrl Pts',(-92.7673736667778,-57.2440265817481,
171.878699917269));
#45388=CARTESIAN_POINT('Ctrl Pts',(-92.9063177114656,-57.1787762224701,
171.975241718896));
#45389=CARTESIAN_POINT('Ctrl Pts',(-93.0863798448037,-57.0941626545074,
172.122130842798));
#45390=CARTESIAN_POINT('Ctrl Pts',(-93.1417074499794,-57.0681551828317,
172.171477751684));
#45391=CARTESIAN_POINT('Ctrl Pts',(-93.2181992503479,-57.03221925648,172.244767934548));
#45392=CARTESIAN_POINT('Ctrl Pts',(-93.2548217785949,-57.0150194895201,
172.281233967651));
#45393=CARTESIAN_POINT('Ctrl Pts',(-93.2948376449404,-56.9962442115694,
172.323214494815));
#45394=CARTESIAN_POINT('Ctrl Pts',(-93.3141848810401,-56.9871724551456,
172.344035313164));
#45395=CARTESIAN_POINT('Ctrl Pts',(-93.3236954404761,-56.9827146845638,
172.354399845872));
#45396=CARTESIAN_POINT('Ctrl Pts',(-93.3277366813326,-56.9808208558246,
172.358831588447));
#45397=CARTESIAN_POINT('Ctrl Pts',(-93.3304231532481,-56.9795619917248,
172.361783776208));
#45398=CARTESIAN_POINT('Ctrl Pts',(-93.3310258878557,-56.9792795491844,
172.362445828695));
#45399=CARTESIAN_POINT('Ctrl Pts',(-93.5983418840511,-56.8540342037519,
172.657424206742));
#45400=CARTESIAN_POINT('Ctrl Pts',(-93.8006909816924,-56.7594348190334,
173.003045307483));
#45401=CARTESIAN_POINT('Ctrl Pts',(-94.0660265072745,-56.6351229429811,
173.731602247926));
#45402=CARTESIAN_POINT('Ctrl Pts',(-94.1292986217245,-56.6052939157322,
174.114172392865));
#45403=CARTESIAN_POINT('Ctrl Pts',(-94.1292986217245,-56.6052939157322,
174.485485069079));
#45404=CARTESIAN_POINT('',(-107.009977058815,-103.84909152684,171.485485069079));
#45405=CARTESIAN_POINT('Origin',(106.899307254449,-150.793932399799,171.485485069079));
#45406=CARTESIAN_POINT('Ctrl Pts',(-109.534287722621,-101.392525888427,
174.485485069079));
#45407=CARTESIAN_POINT('Ctrl Pts',(-109.534766330367,-101.39462272741,174.482903245747));
#45408=CARTESIAN_POINT('Ctrl Pts',(-109.535241658531,-101.396720316011,
174.480321421184));
#45409=CARTESIAN_POINT('Ctrl Pts',(-109.598798782043,-101.679242827829,
174.132701207431));
#45410=CARTESIAN_POINT('Ctrl Pts',(-109.60384151727,-101.975418534307,173.784831173405));
#45411=CARTESIAN_POINT('Ctrl Pts',(-109.486730794348,-102.543377875726,
173.135889204623));
#45412=CARTESIAN_POINT('Ctrl Pts',(-109.370932552772,-102.820739354769,
172.827742940592));
#45413=CARTESIAN_POINT('Ctrl Pts',(-109.044027201355,-103.265197277462,
172.336850351747));
#45414=CARTESIAN_POINT('Ctrl Pts',(-108.861306088238,-103.444418866393,
172.140097108715));
#45415=CARTESIAN_POINT('Ctrl Pts',(-108.457219871866,-103.702395545801,
171.846059671839));
#45416=CARTESIAN_POINT('Ctrl Pts',(-108.256149207368,-103.793261446586,
171.73800308857));
#45417=CARTESIAN_POINT('Ctrl Pts',(-107.831376286778,-103.901466368998,
171.583339306512));
#45418=CARTESIAN_POINT('Ctrl Pts',(-107.618867465661,-103.923371702873,
171.534257289936));
#45419=CARTESIAN_POINT('Ctrl Pts',(-107.268759891529,-103.902517901247,
171.492456480493));
#45420=CARTESIAN_POINT('Ctrl Pts',(-107.137921837206,-103.88198042847,171.485485069079));
#45421=CARTESIAN_POINT('Ctrl Pts',(-107.009977058815,-103.84909152684,171.485485069079));
#45422=CARTESIAN_POINT('Origin',(106.899307254449,-150.793932399799,180.485485069079));
#45423=CARTESIAN_POINT('',(-92.5715804833908,-57.2874890652447,178.785485069079));
#45424=CARTESIAN_POINT('',(-108.319971216218,-103.75403258522,178.785485069079));
#45425=CARTESIAN_POINT('Origin',(106.899307254449,-150.793932399799,178.785485069079));
#45426=CARTESIAN_POINT('',(-108.319971216218,-103.75403258522,173.185485069079));
#45427=CARTESIAN_POINT('',(-108.319971216218,-103.75403258522,180.485485069079));
#45428=CARTESIAN_POINT('',(-92.5715804833908,-57.2874890652447,173.185485069079));
#45429=CARTESIAN_POINT('Origin',(106.899307254449,-150.793932399799,173.185485069079));
#45430=CARTESIAN_POINT('',(-92.5715804833908,-57.2874890652447,178.785485069079));
#45431=CARTESIAN_POINT('Origin',(-70.143810135276,-11.0431453779933,170.985485069079));
#45432=CARTESIAN_POINT('',(-71.9956660035516,-10.2877449258268,178.785485069079));
#45433=CARTESIAN_POINT('Origin',(-70.143810135276,-11.0431453779933,178.785485069079));
#45434=CARTESIAN_POINT('',(-71.9956660035516,-10.2877449258268,180.485485069079));
#45435=CARTESIAN_POINT('',(-71.9956660035516,-10.2877449258268,170.985485069079));
#45436=CARTESIAN_POINT('Origin',(-70.143810135276,-11.0431453779933,180.485485069079));
#45437=CARTESIAN_POINT('Origin',(-69.9391102914966,14.1820463536532,180.985485069079));
#45438=CARTESIAN_POINT('',(-68.087254423221,13.4266459014867,180.985485069079));
#45439=CARTESIAN_POINT('Origin',(-69.9391102914966,14.1820463536532,180.985485069079));
#45440=CARTESIAN_POINT('',(-68.087254423221,13.4266459014867,179.485485069079));
#45441=CARTESIAN_POINT('',(-68.087254423221,13.4266459014867,180.985485069079));
#45442=CARTESIAN_POINT('Origin',(-69.9391102914966,14.1820463536532,179.485485069079));
#45443=CARTESIAN_POINT('Origin',(-84.8548278771908,-59.0746191263193,180.485485069079));
#45444=CARTESIAN_POINT('',(-83.9288999430531,-59.4523193524025,180.485485069079));
#45445=CARTESIAN_POINT('Origin',(-84.8548278771908,-59.0746191263193,180.485485069079));
#45446=CARTESIAN_POINT('',(-83.9288999430531,-59.4523193524025,178.785485069079));
#45447=CARTESIAN_POINT('',(-83.9288999430531,-59.4523193524025,180.485485069079));
#45448=CARTESIAN_POINT('Origin',(-84.8548278771908,-59.0746191263193,178.785485069079));
#45449=CARTESIAN_POINT('Origin',(-31.229031910667,-116.780702189177,180.485485069079));
#45450=CARTESIAN_POINT('',(-104.027257502361,-98.7413465825904,178.785485069079));
#45451=CARTESIAN_POINT('',(-104.027257502361,-98.7413465825904,180.485485069079));
#45452=CARTESIAN_POINT('',(-81.9809794708757,-61.5607798889249,178.785485069079));
#45453=CARTESIAN_POINT('Origin',(-31.229031910667,-116.780702189177,178.785485069079));
#45454=CARTESIAN_POINT('',(-81.9809794708757,-61.5607798889249,180.485485069079));
#45455=CARTESIAN_POINT('Origin',(-70.143810135276,-11.0431453779933,170.985485069079));
#45456=CARTESIAN_POINT('',(-71.9956660035516,-10.2877449258268,171.485485069079));
#45457=CARTESIAN_POINT('Origin',(-70.143810135276,-11.0431453779933,171.485485069079));
#45458=CARTESIAN_POINT('',(-71.9956660035516,-10.2877449258268,173.185485069079));
#45459=CARTESIAN_POINT('',(-71.9956660035516,-10.2877449258268,170.985485069079));
#45460=CARTESIAN_POINT('Origin',(-70.143810135276,-11.0431453779933,173.185485069079));
#45461=CARTESIAN_POINT('Origin',(-69.9391102914966,14.1820463536532,180.985485069079));
#45462=CARTESIAN_POINT('',(-68.087254423221,13.4266459014867,172.485485069079));
#45463=CARTESIAN_POINT('Origin',(-69.9391102914966,14.1820463536532,172.485485069079));
#45464=CARTESIAN_POINT('',(-68.087254423221,13.4266459014867,170.985485069079));
#45465=CARTESIAN_POINT('',(-68.087254423221,13.4266459014867,180.985485069079));
#45466=CARTESIAN_POINT('Origin',(-69.9391102914966,14.1820463536532,170.985485069079));
#45467=CARTESIAN_POINT('Origin',(-84.8548278771908,-59.0746191263193,180.485485069079));
#45468=CARTESIAN_POINT('',(-83.9288999430531,-59.4523193524025,173.185485069079));
#45469=CARTESIAN_POINT('Origin',(-84.8548278771908,-59.0746191263193,173.185485069079));
#45470=CARTESIAN_POINT('',(-83.9288999430531,-59.4523193524025,171.485485069079));
#45471=CARTESIAN_POINT('',(-83.9288999430531,-59.4523193524025,180.485485069079));
#45472=CARTESIAN_POINT('Origin',(-84.8548278771908,-59.0746191263193,171.485485069079));
#45473=CARTESIAN_POINT('Origin',(-31.229031910667,-116.780702189177,180.485485069079));
#45474=CARTESIAN_POINT('',(-104.027257502361,-98.7413465825904,173.185485069079));
#45475=CARTESIAN_POINT('',(-81.9809794708757,-61.5607798889249,173.185485069079));
#45476=CARTESIAN_POINT('Origin',(-31.229031910667,-116.780702189177,173.185485069079));
#45477=CARTESIAN_POINT('',(-104.027257502361,-98.7413465825904,180.485485069079));
#45478=CARTESIAN_POINT('',(-81.9809794708757,-61.5607798889249,180.485485069079));
#45479=CARTESIAN_POINT('Origin',(106.899307254449,-150.793932399799,180.485485069079));
#45480=CARTESIAN_POINT('',(-94.1292986217245,-56.6052939157322,180.485485069079));
#45481=CARTESIAN_POINT('',(-109.534287722621,-101.392525888427,361.145530749938));
#45482=CARTESIAN_POINT('Origin',(-107.048859311027,-106.148770055693,180.485485069079));
#45483=CARTESIAN_POINT('',(-105.613710699519,-102.630519079742,173.185485069079));
#45484=CARTESIAN_POINT('',(-105.613710699519,-102.630519079742,361.145530749938));
#45485=CARTESIAN_POINT('',(-79.4940096800365,-38.5983604123683,173.185485069079));
#45486=CARTESIAN_POINT('Origin',(-107.048859311027,-106.148770055693,180.485485069079));
#45487=CARTESIAN_POINT('',(-105.613710699519,-102.630519079742,178.785485069079));
#45488=CARTESIAN_POINT('',(-105.613710699519,-102.630519079742,361.145530749938));
#45489=CARTESIAN_POINT('',(-79.4940096800365,-38.5983604123683,178.785485069079));
#45490=CARTESIAN_POINT('Origin',(-64.3046088901795,-18.2273525712768,180.485485069079));
#45491=CARTESIAN_POINT('',(-64.3046088901795,-18.2273525712768,172.985485069079));
#45492=CARTESIAN_POINT('',(-64.3046088901795,-18.2273525712768,172.985485069079));
#45493=CARTESIAN_POINT('',(-64.3046088901795,-18.2273525712768,173.185485069079));
#45494=CARTESIAN_POINT('',(-64.3046088901795,-18.2273525712768,180.485485069079));
#45495=CARTESIAN_POINT('',(-73.5957040846178,-41.004369859499,173.185485069079));
#45496=CARTESIAN_POINT('Origin',(-64.100606517944,3.77170156821119,180.485485069079));
#45497=CARTESIAN_POINT('',(-64.3024536808101,-17.9949407268459,172.485485069079));
#45498=CARTESIAN_POINT('',(-64.067029466095,7.39255839147599,172.485485069079));
#45499=CARTESIAN_POINT('',(-64.100606517944,3.77170156821119,172.485485069079));
#45500=CARTESIAN_POINT('',(-64.067029466095,7.39255839147599,172.685485069079));
#45501=CARTESIAN_POINT('',(-64.067029466095,7.39255839147599,180.485485069079));
#45502=CARTESIAN_POINT('',(-64.0976157548621,4.09421722445422,172.685485069079));
#45503=CARTESIAN_POINT('',(-64.100606517944,3.77170156821119,172.685485069079));
#45504=CARTESIAN_POINT('',(-64.1113219987316,2.61617362315227,173.185485069079));
#45505=CARTESIAN_POINT('',(-64.1222537350124,1.437325281122,173.584271796681));
#45506=CARTESIAN_POINT('',(-64.1303313887531,0.566253342026285,173.185485069079));
#45507=CARTESIAN_POINT('Origin',(-64.2669244479369,-14.1635660768473,172.985485069062));
#45508=CARTESIAN_POINT('Origin',(-178.096445811705,1.62308776542128,180.485485069079));
#45509=CARTESIAN_POINT('Origin',(-107.523469003812,-101.851499334574,180.485485069079));
#45510=CARTESIAN_POINT('',(-64.6577925771904,-15.1217749800781,180.485485069079));
#45511=CARTESIAN_POINT('',(-74.9845959858244,-40.4378195203742,180.485485069079));
#45512=CARTESIAN_POINT('',(-64.4948557181401,2.4488872837273,180.485485069079));
#45513=CARTESIAN_POINT('',(-64.6954770194348,-19.1855614746571,180.485485069079));
#45514=CARTESIAN_POINT('',(-73.9667318408259,6.31261103702609,180.485485069079));
#45515=CARTESIAN_POINT('',(-76.6565310829785,7.40982146175055,180.485485069079));
#45516=CARTESIAN_POINT('',(-73.9319567695917,6.14627830862634,180.485485069079));
#45517=CARTESIAN_POINT('',(-73.9667318408259,6.31261103702609,180.485485069079));
#45518=CARTESIAN_POINT('',(-75.1094485830761,3.25967012829823,180.485485069079));
#45519=CARTESIAN_POINT('',(-90.3736629061554,-34.16038275589,180.485485069079));
#45520=CARTESIAN_POINT('',(-85.7265587833611,-43.9488769757557,180.485485069079));
#45521=CARTESIAN_POINT('Origin',(-178.096445811705,1.62308776542128,180.485485069079));
#45522=CARTESIAN_POINT('',(-82.9662394330532,-37.1819845645561,180.485485069079));
#45523=CARTESIAN_POINT('Origin',(-178.096445811705,1.62308776542128,171.485485069079));
#45524=CARTESIAN_POINT('Origin',(-107.523469003812,-101.851499334574,171.485485069079));
#45525=CARTESIAN_POINT('',(-85.7265587833611,-43.9488769757557,171.485485069079));
#45526=CARTESIAN_POINT('',(-92.9256857780509,-61.5974573192564,171.485485069079));
#45527=CARTESIAN_POINT('',(-75.1094485830761,3.25967012829824,171.485485069079));
#45528=CARTESIAN_POINT('Origin',(-178.096445811705,1.62308776542128,171.485485069079));
#45529=CARTESIAN_POINT('',(-73.9319567695917,6.14627830862634,171.485485069079));
#45530=CARTESIAN_POINT('',(-73.3598858593218,7.54870382904371,171.485485069079));
#45531=CARTESIAN_POINT('',(-73.9667318408259,6.31261103702609,171.485485069079));
#45532=CARTESIAN_POINT('',(-73.9319567695917,6.14627830862634,171.485485069079));
#45533=CARTESIAN_POINT('',(-64.4948557181401,2.4488872837273,171.485485069079));
#45534=CARTESIAN_POINT('',(-76.6565310829785,7.40982146175055,171.485485069079));
#45535=CARTESIAN_POINT('',(-64.6577925771904,-15.1217749800782,171.485485069079));
#45536=CARTESIAN_POINT('',(-64.4948557181401,2.4488872837273,171.485485069079));
#45537=CARTESIAN_POINT('',(-83.3698713720824,-60.9942295498001,171.485485069079));
#45538=CARTESIAN_POINT('Origin',(-76.1376696617351,8.68180450729347,180.485485069079));
#45539=CARTESIAN_POINT('',(-75.2878441530478,10.7651423591035,177.485485069079));
#45540=CARTESIAN_POINT('',(-75.2878441530478,10.7651423591035,174.485485069079));
#45541=CARTESIAN_POINT('',(-75.2878441530478,10.7651423591035,180.985485069079));
#45542=CARTESIAN_POINT('',(-78.1205958486722,3.82068285307013,174.485485069079));
#45543=CARTESIAN_POINT('',(-76.1376696617351,8.68180450729347,174.485485069079));
#45544=CARTESIAN_POINT('',(-78.1205958486722,3.82068285307013,177.485485069079));
#45545=CARTESIAN_POINT('',(-78.1205958486722,3.82068285307013,180.485485069079));
#45546=CARTESIAN_POINT('',(-76.1376696617351,8.68180450729347,177.485485069079));
#45547=CARTESIAN_POINT('Origin',(-178.096445811705,1.62308776542128,180.485485069079));
#45548=CARTESIAN_POINT('',(-88.4637952304757,-42.7163749036655,174.485485069079));
#45549=CARTESIAN_POINT('Origin',(-178.096445811705,1.62308776542128,174.485485069079));
#45550=CARTESIAN_POINT('',(-88.4637952304757,-42.7163749036655,177.485485069079));
#45551=CARTESIAN_POINT('',(-88.4637952304757,-42.7163749036655,180.485485069079));
#45552=CARTESIAN_POINT('Origin',(-178.096445811705,1.62308776542128,177.485485069079));
#45553=CARTESIAN_POINT('Origin',(-88.4637952304757,-42.7163749036655,180.485485069079));
#45554=CARTESIAN_POINT('',(-113.298872866457,-103.599293529631,174.485485069079));
#45555=CARTESIAN_POINT('',(-88.4637952304757,-42.7163749036655,177.485485069079));
#45556=CARTESIAN_POINT('Origin',(-64.3046088901795,-18.2273525712768,180.485485069079));
#45557=CARTESIAN_POINT('',(-64.3046088901795,-18.2273525712768,178.985485069079));
#45558=CARTESIAN_POINT('',(-64.3046088901795,-18.2273525712768,178.785485069079));
#45559=CARTESIAN_POINT('',(-64.3046088901795,-18.2273525712768,180.485485069079));
#45560=CARTESIAN_POINT('',(-64.3046088901795,-18.2273525712768,178.985485069079));
#45561=CARTESIAN_POINT('',(-73.5957040846178,-41.004369859499,178.785485069079));
#45562=CARTESIAN_POINT('Origin',(-64.100606517944,3.77170156821119,180.485485069079));
#45563=CARTESIAN_POINT('',(-64.0976157548621,4.09421722445422,179.285485069079));
#45564=CARTESIAN_POINT('',(-64.067029466095,7.39255839147599,179.285485069079));
#45565=CARTESIAN_POINT('',(-64.100606517944,3.77170156821119,179.285485069079));
#45566=CARTESIAN_POINT('',(-64.067029466095,7.39255839147599,179.485485069079));
#45567=CARTESIAN_POINT('',(-64.067029466095,7.39255839147599,180.485485069079));
#45568=CARTESIAN_POINT('',(-64.3024536808101,-17.9949407268459,179.485485069079));
#45569=CARTESIAN_POINT('',(-64.100606517944,3.77170156821119,179.485485069079));
#45570=CARTESIAN_POINT('Origin',(-64.2669244479286,-14.1635660759491,178.985485069037));
#45571=CARTESIAN_POINT('',(-64.1113219987316,2.61617362315227,178.785485069079));
#45572=CARTESIAN_POINT('',(-64.1303313887531,0.566253342026285,178.785485069079));
#45573=CARTESIAN_POINT('',(-64.0969218480186,4.16904622791266,179.310798599544));
#45574=CARTESIAN_POINT('Origin',(-76.1376696617351,8.68180450729347,170.985485069079));
#45575=CARTESIAN_POINT('',(-73.0571341974619,7.42520677607053,170.985485069079));
#45576=CARTESIAN_POINT('',(-65.5950181087078,4.38129500943137,170.985485069079));
#45577=CARTESIAN_POINT('',(-76.1376696617351,8.68180450729347,170.985485069079));
#45578=CARTESIAN_POINT('Origin',(-65.6361368403207,-0.0528357944954805,
172.485485069087));
#45579=CARTESIAN_POINT('Origin',(-72.0398282687001,2.55932829637862,172.485485069078));
#45580=CARTESIAN_POINT('Origin',(-69.9391102914966,14.1820463536532,180.985485069079));
#45581=CARTESIAN_POINT('',(-73.0571341974619,7.42520677607053,180.985485069079));
#45582=CARTESIAN_POINT('',(-65.5950181087078,4.38129500943137,180.985485069079));
#45583=CARTESIAN_POINT('',(-76.1376696617351,8.68180450729347,180.985485069079));
#45584=CARTESIAN_POINT('',(-65.5045147937286,14.14092331283,180.985485069079));
#45585=CARTESIAN_POINT('',(-65.5045147937286,14.14092331283,180.985485069079));
#45586=CARTESIAN_POINT('',(-74.2800401190792,13.2744910851909,180.985485069079));
#45587=CARTESIAN_POINT('Origin',(-69.9391102914966,14.1820463536532,180.985485069079));
#45588=CARTESIAN_POINT('',(-73.2641860378138,8.41555694081837,180.985485069079));
#45589=CARTESIAN_POINT('Origin',(-69.9391102914966,14.1820463536532,170.985485069079));
#45590=CARTESIAN_POINT('',(-74.2800401190792,13.2744910851909,170.985485069079));
#45591=CARTESIAN_POINT('',(-65.5045147937286,14.14092331283,170.985485069079));
#45592=CARTESIAN_POINT('Origin',(-69.9391102914966,14.1820463536532,170.985485069079));
#45593=CARTESIAN_POINT('',(-65.5045147937286,14.14092331283,170.985485069079));
#45594=CARTESIAN_POINT('',(-74.2800401190792,13.2744910851909,170.985485069079));
#45595=CARTESIAN_POINT('Origin',(-76.1376696617351,8.68180450729347,180.985485069079));
#45596=CARTESIAN_POINT('Origin',(-65.6361368403178,-0.0528357944828661,
179.485485069077));
#45597=CARTESIAN_POINT('Origin',(-72.0398282686983,2.55932829637348,179.485485069079));
#45598=CARTESIAN_POINT('Origin',(-75.7482946184945,12.9675241082264,180.985485069079));
#45599=CARTESIAN_POINT('',(-75.0082722890301,9.42792149152613,179.485485069079));
#45600=CARTESIAN_POINT('',(-75.5631600798882,12.0820066431433,179.485485069079));
#45601=CARTESIAN_POINT('',(-75.7482946184945,12.9675241082264,179.485485069079));
#45602=CARTESIAN_POINT('',(-75.5631600798882,12.0820066431433,172.485485069079));
#45603=CARTESIAN_POINT('',(-75.5631600798882,12.0820066431433,180.985485069079));
#45604=CARTESIAN_POINT('',(-75.0082722890301,9.42792149152613,172.485485069079));
#45605=CARTESIAN_POINT('',(-75.7482946184945,12.9675241082264,172.485485069079));
#45606=CARTESIAN_POINT('Origin',(-74.1899511896153,5.51380783648853,174.485485069067));
#45607=CARTESIAN_POINT('Origin',(-74.1899511896128,5.51380783647723,177.485485069089));
#45608=CARTESIAN_POINT('Origin',(-178.096445811705,1.62308776542128,178.785485069079));
#45609=CARTESIAN_POINT('Origin',(-107.523469003812,-101.851499334574,178.785485069079));
#45610=CARTESIAN_POINT('',(-86.9127681729002,-43.414973163782,178.785485069079));
#45611=CARTESIAN_POINT('',(-84.1699457474323,-36.6909742706479,178.785485069079));
#45612=CARTESIAN_POINT('',(-76.4138381126899,3.50385663167992,178.785485069079));
#45613=CARTESIAN_POINT('Origin',(-178.096445811705,1.62308776542128,178.785485069079));
#45614=CARTESIAN_POINT('',(-74.9692357361314,7.04528340827526,178.785485069079));
#45615=CARTESIAN_POINT('',(-91.5773692205345,-33.6693724619818,178.785485069079));
#45616=CARTESIAN_POINT('',(-76.5433132241656,7.68737379261679,178.785485069079));
#45617=CARTESIAN_POINT('Origin',(-178.096445811705,1.62308776542128,173.185485069079));
#45618=CARTESIAN_POINT('Origin',(-107.523469003812,-101.851499334574,173.185485069079));
#45619=CARTESIAN_POINT('',(-74.9692357361314,7.04528340827526,173.185485069079));
#45620=CARTESIAN_POINT('',(-76.5433132241656,7.68737379261679,173.185485069079));
#45621=CARTESIAN_POINT('',(-76.4138381126899,3.50385663167992,173.185485069079));
#45622=CARTESIAN_POINT('',(-91.5773692205345,-33.6693724619818,173.185485069079));
#45623=CARTESIAN_POINT('',(-86.9127681729002,-43.414973163782,173.185485069079));
#45624=CARTESIAN_POINT('Origin',(-178.096445811705,1.62308776542128,173.185485069079));
#45625=CARTESIAN_POINT('',(-84.1699457474323,-36.6909742706479,173.185485069079));
#45626=CARTESIAN_POINT('Origin',(-74.5635921737009,8.03971412295194,180.485485069079));
#45627=CARTESIAN_POINT('',(-74.4503743148881,8.31726645381818,172.685485069079));
#45628=CARTESIAN_POINT('',(-74.3439843284204,8.57808033101511,172.582962524415));
#45629=CARTESIAN_POINT('',(-73.5174599342508,10.6042957578474,172.685485069079));
#45630=CARTESIAN_POINT('',(-74.5635921737009,8.03971412295194,172.685485069079));
#45631=CARTESIAN_POINT('',(-73.5174599342508,10.6042957578474,179.285485069079));
#45632=CARTESIAN_POINT('',(-73.5174599342508,10.6042957578474,180.985485069079));
#45633=CARTESIAN_POINT('',(-74.4503743148881,8.31726645381818,179.285485069079));
#45634=CARTESIAN_POINT('',(-74.5635921737009,8.03971412295194,179.285485069079));
#45635=CARTESIAN_POINT('',(-74.3439843284204,8.57808033101511,179.388007613743));
#45636=CARTESIAN_POINT('',(-76.4138381126899,3.50385663167992,178.785485069079));
#45637=CARTESIAN_POINT('Origin',(-178.096445811705,1.62308776542128,180.485485069079));
#45638=CARTESIAN_POINT('',(-86.9127681729002,-43.414973163782,178.785485069079));
#45639=CARTESIAN_POINT('Origin',(-86.8897177424414,-43.358465288007,180.485485069079));
#45640=CARTESIAN_POINT('Origin',(-75.9180618164546,9.22017071535663,172.582962524415));
#45641=CARTESIAN_POINT('',(-76.0244518029223,8.95935683815971,172.685485069079));
#45642=CARTESIAN_POINT('Origin',(-69.9391102914966,14.1820463536532,179.285485069079));
#45643=CARTESIAN_POINT('',(-73.6644795614854,11.3075056969888,179.285485069079));
#45644=CARTESIAN_POINT('',(-74.0842728524905,13.3154200154528,179.285485069079));
#45645=CARTESIAN_POINT('',(-71.4758555404412,10.4147323427326,179.285485069079));
#45646=CARTESIAN_POINT('',(-76.0244518029223,8.95935683815971,179.285485069079));
#45647=CARTESIAN_POINT('Origin',(-69.9391102914966,14.1820463536532,172.685485069079));
#45648=CARTESIAN_POINT('',(-73.6644795614854,11.3075056969888,172.685485069079));
#45649=CARTESIAN_POINT('',(-71.4758555404412,10.4147323427326,172.685485069079));
#45650=CARTESIAN_POINT('',(-74.0842728524905,13.3154200154528,172.685485069079));
#45651=CARTESIAN_POINT('Origin',(-75.9180618164546,9.22017071535663,179.388007613743));
#45652=CARTESIAN_POINT('Origin',(-74.0842728524905,13.3154200154528,180.985485069079));
#45653=CARTESIAN_POINT('',(-73.6644795614854,11.3075056969888,180.985485069079));
#45654=CARTESIAN_POINT('Origin',(-178.096445811705,1.62308776542128,174.485485069079));
#45655=CARTESIAN_POINT('Ctrl Pts',(-85.7265587833611,-43.9488769757557,
171.485485069079));
#45656=CARTESIAN_POINT('Ctrl Pts',(-85.803250652307,-43.914368625268,171.485485069079));
#45657=CARTESIAN_POINT('Ctrl Pts',(-85.8800425344643,-43.8798139862072,
171.489021188661));
#45658=CARTESIAN_POINT('Ctrl Pts',(-85.9565889693217,-43.8453679850229,
171.496095119029));
#45659=CARTESIAN_POINT('Ctrl Pts',(-86.033153479375,-43.8109138499754,171.503170719791));
#45660=CARTESIAN_POINT('Ctrl Pts',(-86.1094719448409,-43.7765686004695,
171.513785775505));
#45661=CARTESIAN_POINT('Ctrl Pts',(-86.1852015595645,-43.7424860901274,
171.527889918968));
#45662=CARTESIAN_POINT('Ctrl Pts',(-86.2609375075804,-43.708400729454,171.541995241965));
#45663=CARTESIAN_POINT('Ctrl Pts',(-86.3360840355133,-43.674578343957,171.559590124626));
#45664=CARTESIAN_POINT('Ctrl Pts',(-86.4103083068289,-43.6411687240148,
171.580573167936));
#45665=CARTESIAN_POINT('Ctrl Pts',(-86.484621793816,-43.6077189465657,171.601581432327));
#45666=CARTESIAN_POINT('Ctrl Pts',(-86.5580103545068,-43.5746831116226,
171.625985823891));
#45667=CARTESIAN_POINT('Ctrl Pts',(-86.6301569692901,-43.5422046082181,
171.653635642269));
#45668=CARTESIAN_POINT('Ctrl Pts',(-86.6794632456137,-43.5200082228679,
171.672532018619));
#45669=CARTESIAN_POINT('Ctrl Pts',(-86.7281898183943,-43.498071998044,171.692943178902));
#45670=CARTESIAN_POINT('Ctrl Pts',(-86.7762416508316,-43.4764391924131,
171.714808688551));
#45671=CARTESIAN_POINT('Ctrl Pts',(-86.844202757917,-43.4458432849216,171.745733716116));
#45672=CARTESIAN_POINT('Ctrl Pts',(-86.9112560532974,-43.4156547293774,
171.779771728895));
#45673=CARTESIAN_POINT('Ctrl Pts',(-86.9770837908681,-43.3860162755525,
171.816822321779));
#45674=CARTESIAN_POINT('Ctrl Pts',(-87.0428464088205,-43.3564071413559,
171.85383626263));
#45675=CARTESIAN_POINT('Ctrl Pts',(-87.1073854308492,-43.3273472093682,
171.89385665786));
#45676=CARTESIAN_POINT('Ctrl Pts',(-87.1703999907691,-43.2989723048369,
171.936734325967));
#45677=CARTESIAN_POINT('Ctrl Pts',(-87.1969931361074,-43.2869976443596,
171.954829383065));
#45678=CARTESIAN_POINT('Ctrl Pts',(-87.2233150134355,-43.2751448897427,
171.973432729157));
#45679=CARTESIAN_POINT('Ctrl Pts',(-87.2493441620514,-43.263423779529,171.992530657435));
#45680=CARTESIAN_POINT('Ctrl Pts',(-87.3074800086726,-43.2372447955113,
172.035185691818));
#45681=CARTESIAN_POINT('Ctrl Pts',(-87.3638206194771,-43.2118725332094,
172.080056350151));
#45682=CARTESIAN_POINT('Ctrl Pts',(-87.4184018693449,-43.1872918753659,
172.127088854887));
#45683=CARTESIAN_POINT('Ctrl Pts',(-87.4733030268523,-43.162567147164,172.174397023108));
#45684=CARTESIAN_POINT('Ctrl Pts',(-87.5264247429931,-43.1386430837505,
172.223892902332));
#45685=CARTESIAN_POINT('Ctrl Pts',(-87.5777782826842,-43.1155145981015,
172.275566687581));
#45686=CARTESIAN_POINT('Ctrl Pts',(-87.6066127988569,-43.1025281769607,
172.304581018539));
#45687=CARTESIAN_POINT('Ctrl Pts',(-87.6348893538779,-43.0897927850127,
172.334282751313));
#45688=CARTESIAN_POINT('Ctrl Pts',(-87.6626054251485,-43.0773093641887,
172.364675456255));
#45689=CARTESIAN_POINT('Ctrl Pts',(-87.7022875141167,-43.0594364048168,
172.408189777231));
#45690=CARTESIAN_POINT('Ctrl Pts',(-87.7409436157031,-43.0420261537913,
172.453262073559));
#45691=CARTESIAN_POINT('Ctrl Pts',(-87.7783597289956,-43.0251734587016,
172.4997017108));
#45692=CARTESIAN_POINT('Ctrl Pts',(-87.815731883462,-43.0083405632284,172.546086787806));
#45693=CARTESIAN_POINT('Ctrl Pts',(-87.8518666337329,-42.9920640480807,
172.593835653644));
#45694=CARTESIAN_POINT('Ctrl Pts',(-87.8865850093306,-42.9764244448045,
172.642721841606));
#45695=CARTESIAN_POINT('Ctrl Pts',(-87.9213372796397,-42.9607695729615,
172.691655755973));
#45696=CARTESIAN_POINT('Ctrl Pts',(-87.9546701380456,-42.9457529674742,
172.741728816459));
#45697=CARTESIAN_POINT('Ctrl Pts',(-87.9864429746324,-42.9314395340925,
172.792682837345));
#45698=CARTESIAN_POINT('Ctrl Pts',(-87.9921769878195,-42.9288564025695,
172.80187846037));
#45699=CARTESIAN_POINT('Ctrl Pts',(-87.9978603003912,-42.9262961287167,
172.811102703421));
#45700=CARTESIAN_POINT('Ctrl Pts',(-88.0034922301876,-42.9237590351675,
172.820353957677));
#45701=CARTESIAN_POINT('Ctrl Pts',(-88.0423527552536,-42.9062529953147,
172.88418795613));
#45702=CARTESIAN_POINT('Ctrl Pts',(-88.0788588190602,-42.8898062504737,
172.949452352716));
#45703=CARTESIAN_POINT('Ctrl Pts',(-88.1130345979563,-42.8744094619404,
173.016132724375));
#45704=CARTESIAN_POINT('Ctrl Pts',(-88.1471669345133,-42.8590322449437,
173.082728335673));
#45705=CARTESIAN_POINT('Ctrl Pts',(-88.1789752565884,-42.8447021739146,
173.150737019641));
#45706=CARTESIAN_POINT('Ctrl Pts',(-88.2084421665376,-42.8314268668266,
173.220170227426));
#45707=CARTESIAN_POINT('Ctrl Pts',(-88.2248095428287,-42.8240531059923,
173.258736858297));
#45708=CARTESIAN_POINT('Ctrl Pts',(-88.2404537681471,-42.8170050788906,
173.29774338966));
#45709=CARTESIAN_POINT('Ctrl Pts',(-88.2553657482793,-42.8102865845098,
173.337194006733));
#45710=CARTESIAN_POINT('Ctrl Pts',(-88.2785508339243,-42.7998406969589,
173.398531664609));
#45711=CARTESIAN_POINT('Ctrl Pts',(-88.2999340259369,-42.7902077310875,
173.460870943718));
#45712=CARTESIAN_POINT('Ctrl Pts',(-88.3194011434631,-42.7814372835972,
173.523931455552));
#45713=CARTESIAN_POINT('Ctrl Pts',(-88.3388862024838,-42.7726587529926,
173.587050085894));
#45714=CARTESIAN_POINT('Ctrl Pts',(-88.3564514902963,-42.7647443979481,
173.650890795394));
#45715=CARTESIAN_POINT('Ctrl Pts',(-88.3720283006514,-42.7577252737347,
173.715155412108));
#45716=CARTESIAN_POINT('Ctrl Pts',(-88.386961771976,-42.7509960469049,173.776765830993));
#45717=CARTESIAN_POINT('Ctrl Pts',(-88.4000678620873,-42.7450895338618,
173.838765365943));
#45718=CARTESIAN_POINT('Ctrl Pts',(-88.4113270034268,-42.7400163854414,
173.900882979141));
#45719=CARTESIAN_POINT('Ctrl Pts',(-88.4248392494687,-42.7339280322006,
173.975431157173));
#45720=CARTESIAN_POINT('Ctrl Pts',(-88.4357556434908,-42.7290082994433,
174.050459862041));
#45721=CARTESIAN_POINT('Ctrl Pts',(-88.4440715753402,-42.7252609302257,
174.125976729112));
#45722=CARTESIAN_POINT('Ctrl Pts',(-88.4523200024512,-42.7215439803506,
174.200880586548));
#45723=CARTESIAN_POINT('Ctrl Pts',(-88.4580100367288,-42.7189804288886,
174.276265478641));
#45724=CARTESIAN_POINT('Ctrl Pts',(-88.4610900430369,-42.7175931561194,
174.352140154751));
#45725=CARTESIAN_POINT('Ctrl Pts',(-88.4628875726858,-42.7167835266303,
174.396421551042));
#45726=CARTESIAN_POINT('Ctrl Pts',(-88.4637952304757,-42.7163749036655,
174.440869736792));
#45727=CARTESIAN_POINT('Ctrl Pts',(-88.4637952304757,-42.7163749036655,
174.485485069079));
#45728=CARTESIAN_POINT('Ctrl Pts',(-75.1094485830761,3.25967012829815,171.485485069079));
#45729=CARTESIAN_POINT('Ctrl Pts',(-75.1120445846317,3.2601578535513,171.485485069079));
#45730=CARTESIAN_POINT('Ctrl Pts',(-75.1146405871344,3.26064556863604,171.485488417755));
#45731=CARTESIAN_POINT('Ctrl Pts',(-75.5167168146379,3.33618265944911,171.486525721311));
#45732=CARTESIAN_POINT('Ctrl Pts',(-75.9126646258982,3.41031403917456,171.566843725105));
#45733=CARTESIAN_POINT('Ctrl Pts',(-76.6469980011459,3.54738856602921,171.876254905816));
#45734=CARTESIAN_POINT('Ctrl Pts',(-76.9795047377048,3.60924302566342,172.10107561908));
#45735=CARTESIAN_POINT('Ctrl Pts',(-77.5328013082622,3.71195743403252,172.66315582424));
#45736=CARTESIAN_POINT('Ctrl Pts',(-77.7505284531588,3.75226045795544,172.992534367449));
#45737=CARTESIAN_POINT('Ctrl Pts',(-78.0441240514199,3.80656466012662,173.711715425967));
#45738=CARTESIAN_POINT('Ctrl Pts',(-78.1196409565064,3.82050645968902,174.092743833336));
#45739=CARTESIAN_POINT('Ctrl Pts',(-78.1205928503534,3.82068229920291,174.480597840799));
#45740=CARTESIAN_POINT('Ctrl Pts',(-78.1205958486722,3.82068285307013,174.483041537554));
#45741=CARTESIAN_POINT('Ctrl Pts',(-78.1205958486722,3.82068285307013,174.485485069079));
#45742=CARTESIAN_POINT('Origin',(-73.3598858593218,7.54870382904371,174.485485069079));
#45743=CARTESIAN_POINT('Ctrl Pts',(-75.0082722890301,9.42792149152613,172.485485069079));
#45744=CARTESIAN_POINT('Ctrl Pts',(-74.9739694602182,9.26384754701334,172.380688709692));
#45745=CARTESIAN_POINT('Ctrl Pts',(-74.9285618899177,9.10219402976686,172.281030806539));
#45746=CARTESIAN_POINT('Ctrl Pts',(-74.7471063051629,8.54399815677015,171.960847918504));
#45747=CARTESIAN_POINT('Ctrl Pts',(-74.5448580111294,8.09335437334894,171.758213612547));
#45748=CARTESIAN_POINT('Ctrl Pts',(-74.1813523460724,7.1343272986673,171.523884315342));
#45749=CARTESIAN_POINT('Ctrl Pts',(-74.0316751243507,6.62324141552802,171.485485069079));
#45750=CARTESIAN_POINT('Ctrl Pts',(-73.9319567695917,6.14627830862634,171.485485069079));
#45751=CARTESIAN_POINT('Origin',(-178.096445811705,1.62308776542128,177.485485069079));
#45752=CARTESIAN_POINT('Ctrl Pts',(-88.4637952304757,-42.7163749036655,
177.485485069079));
#45753=CARTESIAN_POINT('Ctrl Pts',(-88.4637952304757,-42.7163749036655,
177.561790921156));
#45754=CARTESIAN_POINT('Ctrl Pts',(-88.4611428086215,-42.7175691207664,
177.63760722595));
#45755=CARTESIAN_POINT('Ctrl Pts',(-88.4559170665894,-42.7199234808925,
177.712938143183));
#45756=CARTESIAN_POINT('Ctrl Pts',(-88.4506407020019,-42.7223006480621,
177.788998802434));
#45757=CARTESIAN_POINT('Ctrl Pts',(-88.4427409408535,-42.725860535365,177.86456540467));
#45758=CARTESIAN_POINT('Ctrl Pts',(-88.4322503736512,-42.7305879883129,
177.939647769675));
#45759=CARTESIAN_POINT('Ctrl Pts',(-88.4261504565341,-42.7333368455101,
177.983305676312));
#45760=CARTESIAN_POINT('Ctrl Pts',(-88.4191736653467,-42.7364808333816,
178.026799902097));
#45761=CARTESIAN_POINT('Ctrl Pts',(-88.4113189409649,-42.7400200182287,
178.070131638527));
#45762=CARTESIAN_POINT('Ctrl Pts',(-88.3995732954023,-42.7453123758946,
178.134928211008));
#45763=CARTESIAN_POINT('Ctrl Pts',(-88.3858176127608,-42.751511672146,178.199596284079));
#45764=CARTESIAN_POINT('Ctrl Pts',(-88.3700751037746,-42.7586054082518,
178.263828290739));
#45765=CARTESIAN_POINT('Ctrl Pts',(-88.3543457755428,-42.7656932049744,
178.32800651777));
#45766=CARTESIAN_POINT('Ctrl Pts',(-88.3366330233926,-42.7736739130754,
178.391748902742));
#45767=CARTESIAN_POINT('Ctrl Pts',(-88.3170073313624,-42.7825157579229,
178.45475847167));
#45768=CARTESIAN_POINT('Ctrl Pts',(-88.2981763416785,-42.7909995703079,
178.515216596696));
#45769=CARTESIAN_POINT('Ctrl Pts',(-88.2775846114719,-42.8002760222853,
178.574999737149));
#45770=CARTESIAN_POINT('Ctrl Pts',(-88.255333885622,-42.8103009400199,178.633860422541));
#45771=CARTESIAN_POINT('Ctrl Pts',(-88.2285124211434,-42.8223851738887,
178.704812255441));
#45772=CARTESIAN_POINT('Ctrl Pts',(-88.1993250780218,-42.8355342384889,
178.774328445248));
#45773=CARTESIAN_POINT('Ctrl Pts',(-88.1678143700804,-42.8497302730071,
178.842430176088));
#45774=CARTESIAN_POINT('Ctrl Pts',(-88.1362149276743,-42.8639662836987,
178.910723682074));
#45775=CARTESIAN_POINT('Ctrl Pts',(-88.1022787041779,-42.8792552966842,
178.977595470867));
#45776=CARTESIAN_POINT('Ctrl Pts',(-88.0660039857381,-42.8955974879037,
179.043046798095));
#45777=CARTESIAN_POINT('Ctrl Pts',(-88.045866981765,-42.9046694472095,179.079380467745));
#45778=CARTESIAN_POINT('Ctrl Pts',(-88.0250085722305,-42.9140662704144,
179.115275982884));
#45779=CARTESIAN_POINT('Ctrl Pts',(-88.0034231363848,-42.9237901608107,
179.150729671394));
#45780=CARTESIAN_POINT('Ctrl Pts',(-87.9722169216766,-42.937848056777,179.201985315421));
#45781=CARTESIAN_POINT('Ctrl Pts',(-87.9394301197629,-42.9526188574974,
179.252409455835));
#45782=CARTESIAN_POINT('Ctrl Pts',(-87.9051958767024,-42.9680407049136,
179.301739114946));
#45783=CARTESIAN_POINT('Ctrl Pts',(-87.870989601021,-42.9834499535803,179.351028474603));
#45784=CARTESIAN_POINT('Ctrl Pts',(-87.8353385026604,-42.9995090818352,
179.399224732454));
#45785=CARTESIAN_POINT('Ctrl Pts',(-87.7984148583883,-43.016140288081,179.446095415752));
#45786=CARTESIAN_POINT('Ctrl Pts',(-87.7614367362052,-43.0327960323536,
179.493035253029));
#45787=CARTESIAN_POINT('Ctrl Pts',(-87.7231826255935,-43.0500254153442,
179.538645243775));
#45788=CARTESIAN_POINT('Ctrl Pts',(-87.6838608886981,-43.0677358823089,
179.582727629355));
#45789=CARTESIAN_POINT('Ctrl Pts',(-87.6767708756422,-43.0709292163761,
179.590676024161));
#45790=CARTESIAN_POINT('Ctrl Pts',(-87.6696462380143,-43.0741381562752,
179.598574856602));
#45791=CARTESIAN_POINT('Ctrl Pts',(-87.6624883060175,-43.077362115076,179.606423103847));
#45792=CARTESIAN_POINT('Ctrl Pts',(-87.6131318343259,-43.0995924507871,
179.660539543226));
#45793=CARTESIAN_POINT('Ctrl Pts',(-87.5620001392908,-43.1226209376601,
179.712467127506));
#45794=CARTESIAN_POINT('Ctrl Pts',(-87.5090998705986,-43.1464453560287,
179.762217973346));
#45795=CARTESIAN_POINT('Ctrl Pts',(-87.4564279354805,-43.1701669409953,
179.811754079474));
#45796=CARTESIAN_POINT('Ctrl Pts',(-87.4020020892567,-43.1946778346095,
179.859132678972));
#45797=CARTESIAN_POINT('Ctrl Pts',(-87.3457992427768,-43.2199879417789,
179.904325581094));
#45798=CARTESIAN_POINT('Ctrl Pts',(-87.3141559279581,-43.2342380330006,
179.929770079353));
#45799=CARTESIAN_POINT('Ctrl Pts',(-87.2819488300374,-43.2487416676317,
179.954520963863));
#45800=CARTESIAN_POINT('Ctrl Pts',(-87.2491707291509,-43.2635018775903,
179.978566720226));
#45801=CARTESIAN_POINT('Ctrl Pts',(-87.1874231391168,-43.2913072527857,
180.023864265409));
#45802=CARTESIAN_POINT('Ctrl Pts',(-87.1240278699442,-43.3198535458025,
180.066374884163));
#45803=CARTESIAN_POINT('Ctrl Pts',(-87.0592774397836,-43.3490083205518,
180.10592960246));
#45804=CARTESIAN_POINT('Ctrl Pts',(-86.994455720103,-43.3781951943912,180.145527870073));
#45805=CARTESIAN_POINT('Ctrl Pts',(-86.9282763051401,-43.4079917064379,
180.182163520666));
#45806=CARTESIAN_POINT('Ctrl Pts',(-86.8610515278968,-43.4382572944597,
180.215715122154));
#45807=CARTESIAN_POINT('Ctrl Pts',(-86.8328807003895,-43.450940217253,180.229775062802));
#45808=CARTESIAN_POINT('Ctrl Pts',(-86.8045264883465,-43.463705436197,180.243294021659));
#45809=CARTESIAN_POINT('Ctrl Pts',(-86.7760125604202,-43.4765423282938,
180.256265681589));
#45810=CARTESIAN_POINT('Ctrl Pts',(-86.6840444637611,-43.517946113006,180.298104143037));
#45811=CARTESIAN_POINT('Ctrl Pts',(-86.5897272059914,-43.5604047951258,
180.334559206954));
#45812=CARTESIAN_POINT('Ctrl Pts',(-86.4935381712521,-43.6037025304365,
180.365327483151));
#45813=CARTESIAN_POINT('Ctrl Pts',(-86.4176500184837,-43.6378621949002,
180.389602055099));
#45814=CARTESIAN_POINT('Ctrl Pts',(-86.3405974644073,-43.6725438472567,
180.410337515834));
#45815=CARTESIAN_POINT('Ctrl Pts',(-86.2626305571894,-43.7076351215567,
180.427400457632));
#45816=CARTESIAN_POINT('Ctrl Pts',(-86.2032719335862,-43.7343511965846,
180.44039100421));
#45817=CARTESIAN_POINT('Ctrl Pts',(-86.1434246486064,-43.7612859572302,
180.451240234448));
#45818=CARTESIAN_POINT('Ctrl Pts',(-86.0833635482303,-43.7883156486128,
180.459893197225));
#45819=CARTESIAN_POINT('Ctrl Pts',(-86.0231931259934,-43.8153945388302,
180.46856190993));
#45820=CARTESIAN_POINT('Ctrl Pts',(-85.9628085830272,-43.8425685124351,
180.475026292058));
#45821=CARTESIAN_POINT('Ctrl Pts',(-85.9024912617655,-43.8697111008618,
180.479283238523));
#45822=CARTESIAN_POINT('Ctrl Pts',(-85.8436965864612,-43.8961685038115,
180.48343272295));
#45823=CARTESIAN_POINT('Ctrl Pts',(-85.7849662058798,-43.9225959131722,
180.485485069079));
#45824=CARTESIAN_POINT('Ctrl Pts',(-85.7265587833611,-43.9488769757557,
180.485485069079));
#45825=CARTESIAN_POINT('Ctrl Pts',(-78.1205958486722,3.82068285307014,177.485485069079));
#45826=CARTESIAN_POINT('Ctrl Pts',(-78.1205958486722,3.82068285307014,177.487928596335));
#45827=CARTESIAN_POINT('Ctrl Pts',(-78.1205928503639,3.82068229920484,177.490372288819));
#45828=CARTESIAN_POINT('Ctrl Pts',(-78.1196409581911,3.82050646000022,177.878226291952));
#45829=CARTESIAN_POINT('Ctrl Pts',(-78.044124054763,3.80656466074426,178.259254699594));
#45830=CARTESIAN_POINT('Ctrl Pts',(-77.7505284596663,3.75226045915992,178.978435759267));
#45831=CARTESIAN_POINT('Ctrl Pts',(-77.532801316253,3.71195743551325,179.307814303359));
#45832=CARTESIAN_POINT('Ctrl Pts',(-76.9795047482519,3.60924302762411,179.86989451086));
#45833=CARTESIAN_POINT('Ctrl Pts',(-76.6469980127308,3.54738856818747,180.094715225556));
#45834=CARTESIAN_POINT('Ctrl Pts',(-75.9126646351845,3.41031404091361,180.404126411066));
#45835=CARTESIAN_POINT('Ctrl Pts',(-75.5167168218597,3.33618265904544,180.484444416827));
#45836=CARTESIAN_POINT('Ctrl Pts',(-75.1146405870959,3.2606455686755,180.485481720403));
#45837=CARTESIAN_POINT('Ctrl Pts',(-75.1120445846825,3.26015785356084,180.485485069079));
#45838=CARTESIAN_POINT('Ctrl Pts',(-75.1094485830761,3.25967012829816,180.485485069079));
#45839=CARTESIAN_POINT('Origin',(-90.3736629061554,-34.16038275589,177.485485069079));
#45840=CARTESIAN_POINT('Ctrl Pts',(-73.9319567695917,6.14627830862636,180.485485069079));
#45841=CARTESIAN_POINT('Ctrl Pts',(-74.0316751243507,6.62324141552803,180.485485069079));
#45842=CARTESIAN_POINT('Ctrl Pts',(-74.1813523460724,7.1343272986673,180.447085822817));
#45843=CARTESIAN_POINT('Ctrl Pts',(-74.5448580111294,8.09335437334895,180.212756525611));
#45844=CARTESIAN_POINT('Ctrl Pts',(-74.7471063051629,8.54399815677015,180.010122219654));
#45845=CARTESIAN_POINT('Ctrl Pts',(-74.9285618899177,9.10219402976687,179.68993933162));
#45846=CARTESIAN_POINT('Ctrl Pts',(-74.9739694602182,9.26384754701335,179.590281428466));
#45847=CARTESIAN_POINT('Ctrl Pts',(-75.0082722890301,9.42792149152614,179.485485069079));
#45848=CARTESIAN_POINT('Origin',(-85.6860114280623,-43.8494755819152,174.485485069079));
#45849=CARTESIAN_POINT('Origin',(-82.9662394330532,-37.1819845645561,177.485485069079));
#45850=CARTESIAN_POINT('Origin',(-74.2800401190792,13.2744910851909,172.485485069079));
#45851=CARTESIAN_POINT('',(-75.7482946184945,12.9675241082264,172.485485069079));
#45852=CARTESIAN_POINT('',(-75.7482946184945,12.9675241082264,172.485485069079));
#45853=CARTESIAN_POINT('Origin',(-74.2800401190792,13.2744910851909,172.485485069079));
#45854=CARTESIAN_POINT('Origin',(-65.6935007913861,-17.6608022321519,172.985485069079));
#45855=CARTESIAN_POINT('Ctrl Pts',(-64.30245368081,-17.9949407268459,172.485485069079));
#45856=CARTESIAN_POINT('Ctrl Pts',(-64.3021058587946,-17.95743255836,172.446326101961));
#45857=CARTESIAN_POINT('Ctrl Pts',(-64.3033770800788,-17.9191055129556,
172.407568629705));
#45858=CARTESIAN_POINT('Ctrl Pts',(-64.3167498663848,-17.7106704190456,
172.203844459849));
#45859=CARTESIAN_POINT('Ctrl Pts',(-64.3568840214925,-17.5200526030795,
172.048524450343));
#45860=CARTESIAN_POINT('Ctrl Pts',(-64.4530685529843,-17.0982909105767,
171.800345132073));
#45861=CARTESIAN_POINT('Ctrl Pts',(-64.5071684893368,-16.8667300414478,
171.707442565609));
#45862=CARTESIAN_POINT('Ctrl Pts',(-64.6326468132148,-16.1395439177394,
171.512810422578));
#45863=CARTESIAN_POINT('Ctrl Pts',(-64.6622884122446,-15.6065934538952,
171.485485069079));
#45864=CARTESIAN_POINT('Ctrl Pts',(-64.6577925771903,-15.1217749800779,
171.485485069079));
#45865=CARTESIAN_POINT('Origin',(-69.9391102914966,14.1820463536532,172.485485069079));
#45866=CARTESIAN_POINT('',(-64.0045792842181,14.1270140601776,172.485485069079));
#45867=CARTESIAN_POINT('Origin',(-69.9391102914966,14.1820463536532,172.485485069079));
#45868=CARTESIAN_POINT('Origin',(-65.5045147937286,14.14092331283,172.485485069079));
#45869=CARTESIAN_POINT('Origin',(-65.6005420274545,3.78561082086359,172.485485069079));
#45870=CARTESIAN_POINT('',(-64.100606517944,3.77170156821119,172.485485069079));
#45871=CARTESIAN_POINT('Origin',(-74.2800401190792,13.2744910851909,179.485485069079));
#45872=CARTESIAN_POINT('',(-75.7482946184945,12.9675241082264,179.485485069079));
#45873=CARTESIAN_POINT('Origin',(-74.2800401190792,13.2744910851909,179.485485069079));
#45874=CARTESIAN_POINT('',(-75.7482946184945,12.9675241082265,179.485485069079));
#45875=CARTESIAN_POINT('Origin',(-74.9845959858244,-40.4378195203742,178.985485069079));
#45876=CARTESIAN_POINT('Ctrl Pts',(-64.6577925771903,-15.121774980078,180.485485069079));
#45877=CARTESIAN_POINT('Ctrl Pts',(-64.6622884122446,-15.6065934538952,
180.485485069079));
#45878=CARTESIAN_POINT('Ctrl Pts',(-64.6326468132148,-16.1395439177395,
180.45815971558));
#45879=CARTESIAN_POINT('Ctrl Pts',(-64.5071684893368,-16.8667300414478,
180.26352757255));
#45880=CARTESIAN_POINT('Ctrl Pts',(-64.4530685529843,-17.0982909105767,
180.170625006086));
#45881=CARTESIAN_POINT('Ctrl Pts',(-64.3568840214925,-17.5200526030795,
179.922445687816));
#45882=CARTESIAN_POINT('Ctrl Pts',(-64.3167498663848,-17.7106704190457,
179.767125678309));
#45883=CARTESIAN_POINT('Ctrl Pts',(-64.3033770800788,-17.9191055129557,
179.563401508453));
#45884=CARTESIAN_POINT('Ctrl Pts',(-64.3021058587946,-17.95743255836,179.524644036198));
#45885=CARTESIAN_POINT('Ctrl Pts',(-64.30245368081,-17.9949407268459,179.485485069079));
#45886=CARTESIAN_POINT('Origin',(-69.9391102914966,14.1820463536532,179.485485069079));
#45887=CARTESIAN_POINT('',(-64.0045792842181,14.1270140601776,179.485485069079));
#45888=CARTESIAN_POINT('Origin',(-65.5045147937286,14.14092331283,179.485485069079));
#45889=CARTESIAN_POINT('Origin',(-69.9391102914966,14.1820463536532,179.485485069079));
#45890=CARTESIAN_POINT('Origin',(-65.5045147937286,14.14092331283,179.485485069079));
#45891=CARTESIAN_POINT('',(-64.100606517944,3.77170156821119,179.485485069079));
#45892=CARTESIAN_POINT('Origin',(-107.523469003812,-101.851499334574,361.145530749938));
#45893=CARTESIAN_POINT('Origin',(-76.9710398341703,12.6563024191807,172.485485069079));
#45894=CARTESIAN_POINT('',(-76.9710398341703,12.6563024191807,179.485485069079));
#45895=CARTESIAN_POINT('',(-76.9710398341703,12.6563024191807,172.485485069079));
#45896=CARTESIAN_POINT('Origin',(-73.1927245087776,21.9188007238304,172.485485069079));
#45897=CARTESIAN_POINT('Origin',(-73.1927245087776,21.9188007238304,179.485485069079));
#45898=CARTESIAN_POINT('',(0.,0.,0.));
#45899=CARTESIAN_POINT('Origin',(-84.8548278771908,-59.0746191263193,171.485485069079));
#45900=CARTESIAN_POINT('',(-86.0548278771908,-59.0746191263193,171.485485069079));
#45901=CARTESIAN_POINT('Origin',(-84.8548278771908,-59.0746191263193,171.485485069079));
#45902=CARTESIAN_POINT('',(-84.8548278771908,-59.0746191263193,170.285485069079));
#45903=CARTESIAN_POINT('Origin',(-84.8548278771908,-59.0746191263193,171.485485069079));
#45904=CARTESIAN_POINT('Origin',(-84.8548278771908,-59.0746191263193,180.485485069079));
#45905=CARTESIAN_POINT('',(-86.0548278771908,-59.0746191263193,180.485485069079));
#45906=CARTESIAN_POINT('Origin',(-84.8548278771908,-59.0746191263193,180.485485069079));
#45907=CARTESIAN_POINT('',(-84.8548278771908,-59.0746191263193,181.685485069079));
#45908=CARTESIAN_POINT('Origin',(-84.8548278771908,-59.0746191263193,180.485485069079));
#45909=CARTESIAN_POINT('Origin',(-84.8548278771908,-59.0746191263193,180.485485069079));
#45910=CARTESIAN_POINT('',(-83.8548278771908,-59.0746191263193,171.485485069079));
#45911=CARTESIAN_POINT('Origin',(-84.8548278771908,-59.0746191263193,171.485485069079));
#45912=CARTESIAN_POINT('',(-83.8548278771908,-59.0746191263193,180.485485069079));
#45913=CARTESIAN_POINT('',(-83.8548278771908,-59.0746191263193,180.485485069079));
#45914=CARTESIAN_POINT('Origin',(-84.8548278771908,-59.0746191263193,180.485485069079));
#45915=CARTESIAN_POINT('Origin',(-84.8548278771908,-59.0746191263193,180.485485069079));
#45916=CARTESIAN_POINT('Origin',(-84.8548278771908,-59.0746191263193,171.485485069079));
#45917=CARTESIAN_POINT('',(0.,0.,0.));
#45918=CARTESIAN_POINT('Origin',(-70.1438101352769,-11.0431453779948,178.735485069079));
#45919=CARTESIAN_POINT('',(-73.4509606331853,-11.0591323784537,180.985485069079));
#45920=CARTESIAN_POINT('Origin',(-70.1438101352769,-11.0431453779948,180.985485069079));
#45921=CARTESIAN_POINT('Origin',(-70.1438101352769,-11.0431453779948,175.985485069079));
#45922=CARTESIAN_POINT('',(-70.1534781644024,-9.04316874582809,180.985485069079));
#45923=CARTESIAN_POINT('Origin',(-70.1438101352769,-11.0431453779948,180.985485069079));
#45924=CARTESIAN_POINT('',(-70.1534781644024,-9.04316874582809,170.985485069079));
#45925=CARTESIAN_POINT('',(-70.1534781644024,-9.04316874582809,175.985485069079));
#45926=CARTESIAN_POINT('Origin',(-70.1438101352769,-11.0431453779948,170.985485069079));
#45927=CARTESIAN_POINT('Origin',(-70.1438101352769,-11.0431453779948,173.235485069079));
#45928=CARTESIAN_POINT('',(-73.4509606331853,-11.0591323784537,170.985485069079));
#45929=CARTESIAN_POINT('Origin',(-70.1438101352769,-11.0431453779948,170.985485069079));
#45930=CARTESIAN_POINT('Origin',(-68.1438335031102,-11.0334773488692,170.985485069079));
#45931=CARTESIAN_POINT('Origin',(-68.1438335031102,-11.0334773488692,180.985485069079));
#45932=CARTESIAN_POINT('',(0.,0.,0.));
#45933=CARTESIAN_POINT('Origin',(-84.8548278771908,-59.0746191263193,178.585485069079));
#45934=CARTESIAN_POINT('',(-84.5058642500481,-58.1374828571826,178.585485069079));
#45935=CARTESIAN_POINT('Origin',(-84.8548278771908,-59.0746191263193,178.585485069079));
#45936=CARTESIAN_POINT('',(-84.5058642500481,-58.1374828571826,177.685485069079));
#45937=CARTESIAN_POINT('',(-84.5058642500481,-58.1374828571826,178.585485069079));
#45938=CARTESIAN_POINT('',(-85.5577653075767,-59.7858708180308,177.685485069079));
#45939=CARTESIAN_POINT('Origin',(-84.8548278771908,-59.0746191263193,177.685485069079));
#45940=CARTESIAN_POINT('',(-84.9035795890701,-58.0758081979705,177.685485069079));
#45941=CARTESIAN_POINT('Origin',(-84.8548278771908,-59.0746191263193,177.685485069079));
#45942=CARTESIAN_POINT('Origin',(-84.8548278771908,-59.0746191263193,177.685485069079));
#45943=CARTESIAN_POINT('Origin',(-77.596384432622,-39.5821847282766,178.585485069079));
#45944=CARTESIAN_POINT('',(-77.03410267114,-39.7915629045623,178.585485069079));
#45945=CARTESIAN_POINT('',(-77.4650015118991,-40.1676234767637,178.585484926558));
#45946=CARTESIAN_POINT('Origin',(-77.596384432622,-39.5821847282766,178.585485069079));
#45947=CARTESIAN_POINT('',(-77.2498704957138,-39.7773398653825,177.055074234203));
#45948=CARTESIAN_POINT('',(-77.03410267114,-39.7915629045623,178.585485069079));
#45949=CARTESIAN_POINT('',(-77.2498571612849,-39.7773460826798,174.915920053832));
#45950=CARTESIAN_POINT('',(-77.3304501603129,-39.7397688129298,177.185345426401));
#45951=CARTESIAN_POINT('',(-77.03410267114,-39.7915629045623,173.385485069079));
#45952=CARTESIAN_POINT('',(-77.03410267114,-39.7915629045623,178.585485069079));
#45953=CARTESIAN_POINT('',(-77.4650015118991,-40.1676234767637,173.3854852116));
#45954=CARTESIAN_POINT('Origin',(-77.596384432622,-39.5821847282766,173.385485069079));
#45955=CARTESIAN_POINT('',(-77.8056987826698,-40.1445035064164,173.433770774959));
#45956=CARTESIAN_POINT('Ctrl Pts',(-77.4650015118379,-40.167623476675,173.385485354513));
#45957=CARTESIAN_POINT('Ctrl Pts',(-77.5222920678253,-40.1804805015978,
173.385517889895));
#45958=CARTESIAN_POINT('Ctrl Pts',(-77.580890468835,-40.1848056038886,173.38835249126));
#45959=CARTESIAN_POINT('Ctrl Pts',(-77.6971422272215,-40.1765308873483,
173.403655693534));
#45960=CARTESIAN_POINT('Ctrl Pts',(-77.7531232269699,-40.1640606597343,
173.415935467735));
#45961=CARTESIAN_POINT('Ctrl Pts',(-77.8056942667798,-40.1444919337478,
173.433771387659));
#45962=CARTESIAN_POINT('',(-78.1586259806643,-39.3728300600142,174.385485069105));
#45963=CARTESIAN_POINT('Ctrl Pts',(-77.8056987826698,-40.1445035064164,
173.433770774959));
#45964=CARTESIAN_POINT('Ctrl Pts',(-77.8316025753951,-40.1348599999348,
173.442559365324));
#45965=CARTESIAN_POINT('Ctrl Pts',(-77.8563162910818,-40.1235859591036,
173.452576825659));
#45966=CARTESIAN_POINT('Ctrl Pts',(-77.8797393924345,-40.110999573227,173.463759860592));
#45967=CARTESIAN_POINT('Ctrl Pts',(-77.9021524569635,-40.0989559298771,
173.474460667449));
#45968=CARTESIAN_POINT('Ctrl Pts',(-77.9233830575993,-40.0857111079833,
173.486228127983));
#45969=CARTESIAN_POINT('Ctrl Pts',(-77.9433549726383,-40.071538020758,173.498955663141));
#45970=CARTESIAN_POINT('Ctrl Pts',(-77.9633241715251,-40.0573668610525,
173.511681467373));
#45971=CARTESIAN_POINT('Ctrl Pts',(-77.982034331596,-40.0422680834381,173.525366622401));
#45972=CARTESIAN_POINT('Ctrl Pts',(-77.9994322577124,-40.0265023515187,
173.539859446119));
#45973=CARTESIAN_POINT('Ctrl Pts',(-78.0169241204228,-40.0106514957089,
173.554430520915));
#45974=CARTESIAN_POINT('Ctrl Pts',(-78.0330889895565,-39.9941267838722,
173.569817339963));
#45975=CARTESIAN_POINT('Ctrl Pts',(-78.047905558146,-39.9771754028481,173.585828643786));
#45976=CARTESIAN_POINT('Ctrl Pts',(-78.049822621609,-39.9749821235464,173.58790028982));
#45977=CARTESIAN_POINT('Ctrl Pts',(-78.0517171641965,-39.9727816736662,
173.589982348299));
#45978=CARTESIAN_POINT('Ctrl Pts',(-78.0535891860334,-39.9705745632887,
173.592074369728));
#45979=CARTESIAN_POINT('Ctrl Pts',(-78.0728330194838,-39.9478861182751,
173.613579734231));
#45980=CARTESIAN_POINT('Ctrl Pts',(-78.089853382054,-39.924453320363,173.636258615212));
#45981=CARTESIAN_POINT('Ctrl Pts',(-78.1047842555492,-39.9005911821429,
173.659865265467));
#45982=CARTESIAN_POINT('Ctrl Pts',(-78.1206592741246,-39.875220135525,173.684964668486));
#45983=CARTESIAN_POINT('Ctrl Pts',(-78.1341726700168,-39.8493634840486,
173.711112013678));
#45984=CARTESIAN_POINT('Ctrl Pts',(-78.1455328604065,-39.8233751616464,
173.738044096303));
#45985=CARTESIAN_POINT('Ctrl Pts',(-78.1568930507962,-39.7973868392441,
173.764976178928));
#45986=CARTESIAN_POINT('Ctrl Pts',(-78.1661010214841,-39.7712663408389,
173.792692834852));
#45987=CARTESIAN_POINT('Ctrl Pts',(-78.1733990074322,-39.7453499152769,
173.820969559096));
#45988=CARTESIAN_POINT('Ctrl Pts',(-78.18109670286,-39.7180140513866,173.850794994835));
#45989=CARTESIAN_POINT('Ctrl Pts',(-78.1866425628593,-39.6907966187179,
173.881282707479));
#45990=CARTESIAN_POINT('Ctrl Pts',(-78.1902997744162,-39.6639645935433,
173.912302936584));
#45991=CARTESIAN_POINT('Ctrl Pts',(-78.1942435916019,-39.6350298162232,
173.945754135879));
#45992=CARTESIAN_POINT('Ctrl Pts',(-78.1959924060582,-39.6065425527247,
173.979825829551));
#45993=CARTESIAN_POINT('Ctrl Pts',(-78.1958486262586,-39.5788540211706,
174.014408581675));
#45994=CARTESIAN_POINT('Ctrl Pts',(-78.1957540319387,-39.5606374301254,
174.037160956659));
#45995=CARTESIAN_POINT('Ctrl Pts',(-78.194839549217,-39.5427669704748,174.060135624983));
#45996=CARTESIAN_POINT('Ctrl Pts',(-78.1931823226566,-39.5253477403486,
174.083307866194));
#45997=CARTESIAN_POINT('Ctrl Pts',(-78.1917910998975,-39.5107244957194,
174.102760697886));
#45998=CARTESIAN_POINT('Ctrl Pts',(-78.1898418665052,-39.4963423543713,
174.122368986697));
#45999=CARTESIAN_POINT('Ctrl Pts',(-78.1874866612736,-39.4823936898877,
174.142301808365));
#46000=CARTESIAN_POINT('Ctrl Pts',(-78.1851541826915,-39.4685796236137,
174.162042287453));
#46001=CARTESIAN_POINT('Ctrl Pts',(-78.1824234178568,-39.4551907750551,
174.182101870072));
#46002=CARTESIAN_POINT('Ctrl Pts',(-78.1793987895934,-39.4424389285065,
174.202635548891));
#46003=CARTESIAN_POINT('Ctrl Pts',(-78.1783297262753,-39.4379317526833,
174.209893235091));
#46004=CARTESIAN_POINT('Ctrl Pts',(-78.1772235617853,-39.4335043809312,
174.21721000765));
#46005=CARTESIAN_POINT('Ctrl Pts',(-78.1760836397663,-39.4291668947634,
174.224592137249));
#46006=CARTESIAN_POINT('Ctrl Pts',(-78.1730777137475,-39.4177291276969,
174.244058499917));
#46007=CARTESIAN_POINT('Ctrl Pts',(-78.1696683952291,-39.4065841791719,
174.264097692483));
#46008=CARTESIAN_POINT('Ctrl Pts',(-78.1666558229229,-39.397272372026,174.284826885168));
#46009=CARTESIAN_POINT('Ctrl Pts',(-78.1637494748364,-39.3882889020444,
174.304825160187));
#46010=CARTESIAN_POINT('Ctrl Pts',(-78.1612120338452,-39.3810116904671,
174.325466196324));
#46011=CARTESIAN_POINT('Ctrl Pts',(-78.1597309734151,-39.3768406404591,
174.346822553575));
#46012=CARTESIAN_POINT('Ctrl Pts',(-78.1588547323164,-39.3743729184355,
174.359457634198));
#46013=CARTESIAN_POINT('Ctrl Pts',(-78.1583476777879,-39.3729927506605,
174.372342435271));
#46014=CARTESIAN_POINT('Ctrl Pts',(-78.1583476777881,-39.3729927506605,
174.385485069047));
#46015=CARTESIAN_POINT('',(-78.1586244653881,-39.3728309458164,177.585485069077));
#46016=CARTESIAN_POINT('',(-78.158666194104,-39.372806551991,178.585485069079));
#46017=CARTESIAN_POINT('',(-77.8056988610362,-40.1445034772439,178.537199336601));
#46018=CARTESIAN_POINT('Ctrl Pts',(-78.1583476777881,-39.3729927506604,
177.585485069082));
#46019=CARTESIAN_POINT('Ctrl Pts',(-78.1583476777881,-39.3729927506605,
177.606543111377));
#46020=CARTESIAN_POINT('Ctrl Pts',(-78.1596294469341,-39.3764978870272,
177.626857265634));
#46021=CARTESIAN_POINT('Ctrl Pts',(-78.1616381613638,-39.3823135423054,
177.646497387667));
#46022=CARTESIAN_POINT('Ctrl Pts',(-78.1637229995436,-39.3883495920224,
177.666881806511));
#46023=CARTESIAN_POINT('Ctrl Pts',(-78.1665913487967,-39.3968744879276,
177.686540737803));
#46024=CARTESIAN_POINT('Ctrl Pts',(-78.1695883704607,-39.4065726866962,
177.705593053786));
#46025=CARTESIAN_POINT('Ctrl Pts',(-78.1717716424418,-39.4136376358397,
177.719472295355));
#46026=CARTESIAN_POINT('Ctrl Pts',(-78.174022450919,-39.4213256630031,177.733030512162));
#46027=CARTESIAN_POINT('Ctrl Pts',(-78.1760752475433,-39.4291349653113,
177.746323654485));
#46028=CARTESIAN_POINT('Ctrl Pts',(-78.1796664380935,-39.4427966658032,
177.769578859858));
#46029=CARTESIAN_POINT('Ctrl Pts',(-78.1829591937475,-39.4574596072776,
177.792348582069));
#46030=CARTESIAN_POINT('Ctrl Pts',(-78.1857889481807,-39.4727725746961,
177.814748829435));
#46031=CARTESIAN_POINT('Ctrl Pts',(-78.1886413594616,-39.4882081476548,
177.837328427697));
#46032=CARTESIAN_POINT('Ctrl Pts',(-78.1910235140542,-39.5043040816822,
177.859533548057));
#46033=CARTESIAN_POINT('Ctrl Pts',(-78.1927230572288,-39.520725590416,177.881497529369));
#46034=CARTESIAN_POINT('Ctrl Pts',(-78.1928989309815,-39.5224249366932,
177.883770427096));
#46035=CARTESIAN_POINT('Ctrl Pts',(-78.1930674551391,-39.5241277921344,
177.886040747814));
#46036=CARTESIAN_POINT('Ctrl Pts',(-78.1932283667941,-39.5258338015101,
177.888308641737));
#46037=CARTESIAN_POINT('Ctrl Pts',(-78.1951412252173,-39.5461142119357,
177.915268528484));
#46038=CARTESIAN_POINT('Ctrl Pts',(-78.1960338984988,-39.5668410266997,
177.941748603447));
#46039=CARTESIAN_POINT('Ctrl Pts',(-78.1958302050792,-39.5879108654907,
177.967815585286));
#46040=CARTESIAN_POINT('Ctrl Pts',(-78.1956284950027,-39.6087755493006,
177.993628755446));
#46041=CARTESIAN_POINT('Ctrl Pts',(-78.1943515214607,-39.6299766883225,
178.0190380862));
#46042=CARTESIAN_POINT('Ctrl Pts',(-78.1918820718927,-39.6514390060816,
178.044100477535));
#46043=CARTESIAN_POINT('Ctrl Pts',(-78.1894808174157,-39.6723086311488,
178.068470758337));
#46044=CARTESIAN_POINT('Ctrl Pts',(-78.1859515928356,-39.6934254635894,
178.092514045181));
#46045=CARTESIAN_POINT('Ctrl Pts',(-78.181150111863,-39.7147415708539,178.116258460794));
#46046=CARTESIAN_POINT('Ctrl Pts',(-78.1788875895975,-39.7247860066383,
178.127447148058));
#46047=CARTESIAN_POINT('Ctrl Pts',(-78.176342078521,-39.7348749783378,178.138569023899));
#46048=CARTESIAN_POINT('Ctrl Pts',(-78.1734960538477,-39.7450048916319,
178.149624088881));
#46049=CARTESIAN_POINT('Ctrl Pts',(-78.1664823260289,-39.7699689951893,
178.176868131256));
#46050=CARTESIAN_POINT('Ctrl Pts',(-78.1577095484763,-39.7951364254273,
178.203590494714));
#46051=CARTESIAN_POINT('Ctrl Pts',(-78.1469244962564,-39.8202256160684,
178.229632583319));
#46052=CARTESIAN_POINT('Ctrl Pts',(-78.1365609419034,-39.8443342792052,
178.254656903574));
#46053=CARTESIAN_POINT('Ctrl Pts',(-78.1243384322505,-39.8683711781007,
178.279053143627));
#46054=CARTESIAN_POINT('Ctrl Pts',(-78.1100449468631,-39.8920804832296,
178.302635096528));
#46055=CARTESIAN_POINT('Ctrl Pts',(-78.0964140060138,-39.9146907932435,
178.325123957459));
#46056=CARTESIAN_POINT('Ctrl Pts',(-78.0808988659364,-39.9370035953691,
178.346871943661));
#46057=CARTESIAN_POINT('Ctrl Pts',(-78.0633391929321,-39.9587850372975,
178.367677462424));
#46058=CARTESIAN_POINT('Ctrl Pts',(-78.0600909570606,-39.962814227419,178.371526123636));
#46059=CARTESIAN_POINT('Ctrl Pts',(-78.0567728460438,-39.9668251906836,
178.375342428917));
#46060=CARTESIAN_POINT('Ctrl Pts',(-78.0533839713637,-39.9708163811803,
178.37912496045));
#46061=CARTESIAN_POINT('Ctrl Pts',(-78.0381562345498,-39.9887505936238,
178.3961215744));
#46062=CARTESIAN_POINT('Ctrl Pts',(-78.0214792509514,-40.0061786390317,
178.412402159754));
#46063=CARTESIAN_POINT('Ctrl Pts',(-78.0034060666603,-40.0228415926461,
178.427758408585));
#46064=CARTESIAN_POINT('Ctrl Pts',(-77.9862521315262,-40.0386570251032,
178.442333598662));
#46065=CARTESIAN_POINT('Ctrl Pts',(-77.9678413089092,-40.0537827074521,
178.45607577319));
#46066=CARTESIAN_POINT('Ctrl Pts',(-77.9482495099567,-40.0679806950435,
178.468847266813));
#46067=CARTESIAN_POINT('Ctrl Pts',(-77.928632010329,-40.0821973076662,178.481635514181));
#46068=CARTESIAN_POINT('Ctrl Pts',(-77.9078311666701,-40.0954833749289,
178.493450152086));
#46069=CARTESIAN_POINT('Ctrl Pts',(-77.8859429696398,-40.1075895985258,
178.504200235491));
#46070=CARTESIAN_POINT('Ctrl Pts',(-77.8638991823429,-40.1197818781168,
178.51502673489));
#46071=CARTESIAN_POINT('Ctrl Pts',(-77.8407533339131,-40.130777031073,178.524773356882));
#46072=CARTESIAN_POINT('Ctrl Pts',(-77.8166118463901,-40.1403164142105,
178.533399105501));
#46073=CARTESIAN_POINT('Ctrl Pts',(-77.8129963943436,-40.1417450412681,
178.534690905787));
#46074=CARTESIAN_POINT('Ctrl Pts',(-77.8093586138701,-40.1431410178554,
178.535957662038));
#46075=CARTESIAN_POINT('Ctrl Pts',(-77.8056988610362,-40.1445034772439,
178.537199336601));
#46076=CARTESIAN_POINT('Ctrl Pts',(-77.8056943451453,-40.1444919045775,
178.537198723902));
#46077=CARTESIAN_POINT('Ctrl Pts',(-77.7534354935633,-40.1639444317979,
178.554928733475));
#46078=CARTESIAN_POINT('Ctrl Pts',(-77.6978009243969,-40.1763845824508,
178.567170792542));
#46079=CARTESIAN_POINT('Ctrl Pts',(-77.5815770850698,-40.1848554744716,
178.582583818994));
#46080=CARTESIAN_POINT('Ctrl Pts',(-77.5226296507783,-40.1805562612473,
178.585452056548));
#46081=CARTESIAN_POINT('Ctrl Pts',(-77.4650015118378,-40.167623476675,178.585484783646));
#46082=CARTESIAN_POINT('Origin',(-84.8548278771908,-59.0746191263193,178.585485069079));
#46083=CARTESIAN_POINT('',(-85.5577653075812,-59.7858708180264,174.285485069079));
#46084=CARTESIAN_POINT('',(-84.5058642500481,-58.1374828571826,174.285485069079));
#46085=CARTESIAN_POINT('Origin',(-84.8548278771908,-59.0746191263193,174.285485069079));
#46086=CARTESIAN_POINT('',(-84.5058642500481,-58.1374828571826,173.385485069079));
#46087=CARTESIAN_POINT('',(-84.5058642500481,-58.1374828571826,178.585485069079));
#46088=CARTESIAN_POINT('Origin',(-84.8548278771908,-59.0746191263193,173.385485069079));
#46089=CARTESIAN_POINT('',(-84.9035795890703,-58.0758081979706,174.285485069079));
#46090=CARTESIAN_POINT('Origin',(-84.8548278771908,-59.0746191263193,174.285485069079));
#46091=CARTESIAN_POINT('Origin',(-84.8548278771908,-59.0746191263193,174.285485069079));
#46092=CARTESIAN_POINT('Origin',(-99.6210548294771,-101.594714864612,178.585485069079));
#46093=CARTESIAN_POINT('',(-99.6210548299422,-101.594714864439,177.585485069079));
#46094=CARTESIAN_POINT('',(-99.6210548299422,-101.594714864439,174.385485069079));
#46095=CARTESIAN_POINT('',(-99.6210548294771,-101.594714864612,178.585485069079));
#46096=CARTESIAN_POINT('',(-99.1880632280731,-101.755948961215,174.385485069079));
#46097=CARTESIAN_POINT('',(-98.2153504257721,-102.118160305326,174.385485069079));
#46098=CARTESIAN_POINT('',(-99.1880632280731,-101.755948961215,177.585485069079));
#46099=CARTESIAN_POINT('',(-99.1880632280731,-101.755948961215,178.585485069079));
#46100=CARTESIAN_POINT('',(-99.6210548294771,-101.594714864612,177.585485069079));
#46101=CARTESIAN_POINT('Ctrl Pts',(-97.8838106736817,-101.114486609555,
174.371590892235));
#46102=CARTESIAN_POINT('Ctrl Pts',(-97.8838106736817,-101.114486609555,
173.188263904448));
#46103=CARTESIAN_POINT('Ctrl Pts',(-96.3541371085078,-96.1722845480714,
174.371590892235));
#46104=CARTESIAN_POINT('Ctrl Pts',(-96.3541371085078,-96.1722845480714,
173.188263904448));
#46105=CARTESIAN_POINT('Ctrl Pts',(-91.1365269123698,-76.1991465747503,
174.371590892235));
#46106=CARTESIAN_POINT('Ctrl Pts',(-91.1365269123698,-76.1991465747503,
173.188263904448));
#46107=CARTESIAN_POINT('Ctrl Pts',(-87.1439910232441,-64.4286763559758,
174.371590892235));
#46108=CARTESIAN_POINT('Ctrl Pts',(-87.1439910232441,-64.4286763559758,
173.188263904448));
#46109=CARTESIAN_POINT('Ctrl Pts',(-83.9950826197058,-63.9298573380069,
174.371590892235));
#46110=CARTESIAN_POINT('Ctrl Pts',(-83.9950826197058,-63.9298573380069,
173.188263904448));
#46111=CARTESIAN_POINT('Ctrl Pts',(-81.9013008568494,-58.3070397231869,
174.371590892235));
#46112=CARTESIAN_POINT('Ctrl Pts',(-81.9013008568494,-58.3070397231869,
173.188263904448));
#46113=CARTESIAN_POINT('',(-94.2301013700656,-88.1262479603296,174.285485110655));
#46114=CARTESIAN_POINT('',(-81.9013008568494,-58.3070397231869,174.285485069079));
#46115=CARTESIAN_POINT('Ctrl Pts',(-94.2301013700775,-88.1262479603088,
174.285485069079));
#46116=CARTESIAN_POINT('Ctrl Pts',(-92.4302378087403,-81.6315356194262,
174.285485069079));
#46117=CARTESIAN_POINT('Ctrl Pts',(-89.7937145858027,-72.240376274824,174.285485069079));
#46118=CARTESIAN_POINT('Ctrl Pts',(-87.1439910232441,-64.4286763559758,
174.285485069079));
#46119=CARTESIAN_POINT('Ctrl Pts',(-83.9950826197058,-63.9298573380069,
174.285485069079));
#46120=CARTESIAN_POINT('Ctrl Pts',(-81.9013008568494,-58.3070397231869,
174.285485069079));
#46121=CARTESIAN_POINT('',(-97.8838106717876,-101.114486603435,174.36571584827));
#46122=CARTESIAN_POINT('Ctrl Pts',(-94.2301013700819,-88.1262479603247,
174.285485152574));
#46123=CARTESIAN_POINT('Ctrl Pts',(-94.8572392714732,-90.3892418644711,
174.285505819717));
#46124=CARTESIAN_POINT('Ctrl Pts',(-95.4293953813936,-92.4665577589316,
174.289138567121));
#46125=CARTESIAN_POINT('Ctrl Pts',(-96.9354756174802,-97.8900543030279,
174.323115739585));
#46126=CARTESIAN_POINT('Ctrl Pts',(-97.5030442713843,-99.8842734829934,
174.356479113651));
#46127=CARTESIAN_POINT('Ctrl Pts',(-97.8838106717875,-101.114486603435,
174.36571584829));
#46128=CARTESIAN_POINT('',(-97.8838106723181,-101.11448660515,173.385485069079));
#46129=CARTESIAN_POINT('',(-97.8838106722024,-101.114486604776,174.285485069079));
#46130=CARTESIAN_POINT('',(-81.9013008568494,-58.3070397231869,173.385485069079));
#46131=CARTESIAN_POINT('Ctrl Pts',(-97.8838106722024,-101.114486604776,
173.385485069079));
#46132=CARTESIAN_POINT('Ctrl Pts',(-96.3541371055762,-96.1722845368492,
173.385485069079));
#46133=CARTESIAN_POINT('Ctrl Pts',(-91.1365269114412,-76.1991465720129,
173.385485069079));
#46134=CARTESIAN_POINT('Ctrl Pts',(-87.1439910232441,-64.4286763559758,
173.385485069079));
#46135=CARTESIAN_POINT('Ctrl Pts',(-83.9950826197058,-63.9298573380069,
173.385485069079));
#46136=CARTESIAN_POINT('Ctrl Pts',(-81.9013008568494,-58.3070397231869,
173.385485069079));
#46137=CARTESIAN_POINT('',(-81.9013008568494,-58.3070397231869,178.585485069079));
#46138=CARTESIAN_POINT('Origin',(-48.2819354919502,-57.24716229829,178.585485069079));
#46139=CARTESIAN_POINT('',(-80.6956086449654,-48.2616817644572,174.285485069079));
#46140=CARTESIAN_POINT('Origin',(-48.2819354919502,-57.24716229829,174.285485069079));
#46141=CARTESIAN_POINT('Origin',(-48.2819354919502,-57.24716229829,173.385485069079));
#46142=CARTESIAN_POINT('Ctrl Pts',(-77.0748911463595,-39.8589256890876,
174.590829198952));
#46143=CARTESIAN_POINT('Ctrl Pts',(-77.1258588534607,-39.9433224547489,
174.592143873877));
#46144=CARTESIAN_POINT('Ctrl Pts',(-77.1764462985522,-40.0279274916938,
174.593076422781));
#46145=CARTESIAN_POINT('Ctrl Pts',(-77.3118277495375,-40.2566253387939,
174.59465858183));
#46146=CARTESIAN_POINT('Ctrl Pts',(-77.3957878287932,-40.400899198962,174.594658945545));
#46147=CARTESIAN_POINT('Ctrl Pts',(-77.6960535448169,-40.9258180381849,
174.591863571298));
#46148=CARTESIAN_POINT('Ctrl Pts',(-77.9051062567381,-41.3082355654289,
174.584711888553));
#46149=CARTESIAN_POINT('Ctrl Pts',(-78.474706173954,-42.4011423337224,174.550066413528));
#46150=CARTESIAN_POINT('Ctrl Pts',(-78.8133875775858,-43.1109905067965,
174.512103266793));
#46151=CARTESIAN_POINT('Ctrl Pts',(-79.7866388893984,-45.3484841750064,
174.382338566305));
#46152=CARTESIAN_POINT('Ctrl Pts',(-80.3006668857753,-46.836993007004,174.28548333118));
#46153=CARTESIAN_POINT('Ctrl Pts',(-80.6956086449654,-48.261681764457,174.285485069103));
#46154=CARTESIAN_POINT('Origin',(-93.2994946198038,-77.3496518591637,178.585485069079));
#46155=CARTESIAN_POINT('',(-98.376517057274,-100.991065637145,178.585485066968));
#46156=CARTESIAN_POINT('',(-97.9019633317937,-101.167776319221,178.585485069079));
#46157=CARTESIAN_POINT('',(-101.649120271255,-99.7724387145074,178.585485069079));
#46158=CARTESIAN_POINT('',(-97.883810672318,-101.114486605149,178.585485069079));
#46159=CARTESIAN_POINT('Origin',(-98.8390996009304,-100.818812692078,178.585485069079));
#46160=CARTESIAN_POINT('',(-81.9013008568494,-58.3070397231869,178.585485069079));
#46161=CARTESIAN_POINT('Ctrl Pts',(-97.8838106722022,-101.114486604775,
178.585485069079));
#46162=CARTESIAN_POINT('Ctrl Pts',(-96.3541371055757,-96.1722845368475,
178.585485069079));
#46163=CARTESIAN_POINT('Ctrl Pts',(-91.1365269114411,-76.1991465720125,
178.585485069079));
#46164=CARTESIAN_POINT('Ctrl Pts',(-87.1439910232441,-64.4286763559758,
178.585485069079));
#46165=CARTESIAN_POINT('Ctrl Pts',(-83.9950826197058,-63.9298573380069,
178.585485069079));
#46166=CARTESIAN_POINT('Ctrl Pts',(-81.9013008568494,-58.3070397231869,
178.585485069079));
#46167=CARTESIAN_POINT('Origin',(-48.2819354919502,-57.24716229829,178.585485069079));
#46168=CARTESIAN_POINT('Ctrl Pts',(-77.4650015118695,-40.1676234768323,
178.585484783646));
#46169=CARTESIAN_POINT('Ctrl Pts',(-77.6905814020153,-40.555127005694,178.58548463742));
#46170=CARTESIAN_POINT('Ctrl Pts',(-77.9138848638019,-40.9434090043415,
178.585484508233));
#46171=CARTESIAN_POINT('Ctrl Pts',(-78.1332843656806,-41.3333760529069,
178.585484451998));
#46172=CARTESIAN_POINT('Ctrl Pts',(-78.4717618076451,-41.9349956915966,
178.585484365242));
#46173=CARTESIAN_POINT('Ctrl Pts',(-78.8029288442396,-42.5395302271617,
178.585484447149));
#46174=CARTESIAN_POINT('Ctrl Pts',(-79.1274796035695,-43.1466863215047,
178.585484576633));
#46175=CARTESIAN_POINT('Ctrl Pts',(-79.6250115124666,-44.07744837315,178.585484775131));
#46176=CARTESIAN_POINT('Ctrl Pts',(-80.1070311508828,-45.0143523211482,
178.585484994787));
#46177=CARTESIAN_POINT('Ctrl Pts',(-80.5756237742355,-45.9565750778124,
178.585485043419));
#46178=CARTESIAN_POINT('Ctrl Pts',(-80.719647585736,-46.2461709995885,178.585485058367));
#46179=CARTESIAN_POINT('Ctrl Pts',(-80.8624028290514,-46.5362697111046,
178.585485063812));
#46180=CARTESIAN_POINT('Ctrl Pts',(-81.0039496069982,-46.8268481729705,
178.58548506622));
#46181=CARTESIAN_POINT('Ctrl Pts',(-81.0837898722371,-46.9907506072371,
178.585485067579));
#46182=CARTESIAN_POINT('Ctrl Pts',(-81.1632479651378,-47.1548045771697,
178.585485068005));
#46183=CARTESIAN_POINT('Ctrl Pts',(-81.2423319510288,-47.3190072870547,
178.585485068133));
#46184=CARTESIAN_POINT('Ctrl Pts',(-81.8218342303691,-48.5222324859381,
178.585485069074));
#46185=CARTESIAN_POINT('Ctrl Pts',(-82.38085463941,-49.7335938646736,178.585485068901));
#46186=CARTESIAN_POINT('Ctrl Pts',(-82.9219084178718,-50.9520888272408,
178.58548506889));
#46187=CARTESIAN_POINT('Ctrl Pts',(-83.4244472543089,-52.0838451610268,
178.585485068881));
#46188=CARTESIAN_POINT('Ctrl Pts',(-83.9114855009559,-53.2217559573636,
178.585485068821));
#46189=CARTESIAN_POINT('Ctrl Pts',(-84.3850017277789,-54.3650338933268,
178.585485068922));
#46190=CARTESIAN_POINT('Ctrl Pts',(-84.4273715190481,-54.467333338975,178.585485068931));
#46191=CARTESIAN_POINT('Ctrl Pts',(-84.469632549005,-54.5696759937385,178.585485068941));
#46192=CARTESIAN_POINT('Ctrl Pts',(-84.5117857638681,-54.6720615186019,
178.585485068951));
#46193=CARTESIAN_POINT('Ctrl Pts',(-85.1131994842138,-56.1328293299712,
178.585485069102));
#46194=CARTESIAN_POINT('Ctrl Pts',(-85.6926892826506,-57.6023030610518,
178.585485069069));
#46195=CARTESIAN_POINT('Ctrl Pts',(-86.2529554615349,-59.0794092453283,
178.585485069072));
#46196=CARTESIAN_POINT('Ctrl Pts',(-86.6328377473246,-60.0809447561002,
178.585485069073));
#46197=CARTESIAN_POINT('Ctrl Pts',(-87.0038811370241,-61.0859896879636,
178.585485069073));
#46198=CARTESIAN_POINT('Ctrl Pts',(-87.3669151039208,-62.0942150904523,
178.585485069076));
#46199=CARTESIAN_POINT('Ctrl Pts',(-87.3769344349696,-62.1220409827942,
178.585485069076));
#46200=CARTESIAN_POINT('Ctrl Pts',(-87.3869476469901,-62.1498693064267,
178.585485069076));
#46201=CARTESIAN_POINT('Ctrl Pts',(-87.3969547526199,-62.1777000567301,
178.585485069076));
#46202=CARTESIAN_POINT('Ctrl Pts',(-88.0123319305732,-63.8891248398365,
178.585485069081));
#46203=CARTESIAN_POINT('Ctrl Pts',(-88.6046242589736,-65.6097164187148,
178.585485069081));
#46204=CARTESIAN_POINT('Ctrl Pts',(-89.1767249350884,-67.3383248097952,
178.585485069077));
#46205=CARTESIAN_POINT('Ctrl Pts',(-89.4481762250666,-68.1585178233966,
178.585485069076));
#46206=CARTESIAN_POINT('Ctrl Pts',(-89.7150809981247,-68.9805160269103,
178.585485069073));
#46207=CARTESIAN_POINT('Ctrl Pts',(-89.9777446627557,-69.8041983278515,
178.585485069061));
#46208=CARTESIAN_POINT('Ctrl Pts',(-89.9958921332768,-69.861106656973,178.58548506906));
#46209=CARTESIAN_POINT('Ctrl Pts',(-90.0140193906421,-69.91802307165,178.585485069059));
#46210=CARTESIAN_POINT('Ctrl Pts',(-90.0321265334954,-69.974947529394,178.585485069058));
#46211=CARTESIAN_POINT('Ctrl Pts',(-90.6556985380883,-71.9353064061813,
178.585485069019));
#46212=CARTESIAN_POINT('Ctrl Pts',(-91.2553870982626,-73.9057023814814,
178.585485068557));
#46213=CARTESIAN_POINT('Ctrl Pts',(-91.8342083922678,-75.8835284381501,
178.585485066831));
#46214=CARTESIAN_POINT('Ctrl Pts',(-92.4366613560735,-77.9421036531137,
178.585485065034));
#46215=CARTESIAN_POINT('Ctrl Pts',(-93.0165082496544,-80.0087281231012,
178.585485062237));
#46216=CARTESIAN_POINT('Ctrl Pts',(-93.5771032551113,-82.0804951687553,
178.585485063212));
#46217=CARTESIAN_POINT('Ctrl Pts',(-93.8691776689443,-83.1599021195265,
178.585485063719));
#46218=CARTESIAN_POINT('Ctrl Pts',(-94.1560254278893,-84.2407055417337,
178.585485065367));
#46219=CARTESIAN_POINT('Ctrl Pts',(-94.4381163838179,-85.3224975248452,
178.585485067051));
#46220=CARTESIAN_POINT('Ctrl Pts',(-94.5030528267729,-85.5715226067351,
178.585485067439));
#46221=CARTESIAN_POINT('Ctrl Pts',(-94.5677452759793,-85.8206032934907,
178.585485067419));
#46222=CARTESIAN_POINT('Ctrl Pts',(-94.6321980467042,-86.06973522053,178.585485067102));
#46223=CARTESIAN_POINT('Ctrl Pts',(-95.1418708908417,-88.039794480843,178.585485064593));
#46224=CARTESIAN_POINT('Ctrl Pts',(-95.6360250446987,-90.0141207468549,
178.585484976939));
#46225=CARTESIAN_POINT('Ctrl Pts',(-96.1219981705027,-91.9904905111795,
178.5854850137));
#46226=CARTESIAN_POINT('Ctrl Pts',(-96.2175637821243,-92.3791395439954,
178.585485020929));
#46227=CARTESIAN_POINT('Ctrl Pts',(-96.3128128668425,-92.7678675558309,
178.58548503405));
#46228=CARTESIAN_POINT('Ctrl Pts',(-96.4078010227875,-93.1566576401014,
178.585485047111));
#46229=CARTESIAN_POINT('Ctrl Pts',(-96.49385330348,-93.5088728518749,178.585485058943));
#46230=CARTESIAN_POINT('Ctrl Pts',(-96.5797668758499,-93.8611155073599,
178.585485057239));
#46231=CARTESIAN_POINT('Ctrl Pts',(-96.6655567819583,-94.2133925591645,
178.585485051882));
#46232=CARTESIAN_POINT('Ctrl Pts',(-96.8983471324597,-95.1692940408562,
178.585485037346));
#46233=CARTESIAN_POINT('Ctrl Pts',(-97.1298683277641,-96.1255675264222,
178.585484955934));
#46234=CARTESIAN_POINT('Ctrl Pts',(-97.3642924294251,-97.0810624897178,
178.585485025112));
#46235=CARTESIAN_POINT('Ctrl Pts',(-97.4633229695275,-97.4847035044845,
178.585485054336));
#46236=CARTESIAN_POINT('Ctrl Pts',(-97.5629746719815,-97.8881695057605,
178.585485062002));
#46237=CARTESIAN_POINT('Ctrl Pts',(-97.6636749002389,-98.2913808726464,
178.585485062489));
#46238=CARTESIAN_POINT('Ctrl Pts',(-97.7260872514047,-98.5412846698832,
178.585485062791));
#46239=CARTESIAN_POINT('Ctrl Pts',(-97.7888472641501,-98.7911089883279,
178.585485061828));
#46240=CARTESIAN_POINT('Ctrl Pts',(-97.8524422630192,-99.0407060185016,
178.585485047837));
#46241=CARTESIAN_POINT('Ctrl Pts',(-97.9614492780947,-99.4685356861605,
178.585485023857));
#46242=CARTESIAN_POINT('Ctrl Pts',(-98.072667959701,-99.8957209843174,178.585485018479));
#46243=CARTESIAN_POINT('Ctrl Pts',(-98.1886188504326,-100.321776749252,
178.585485035129));
#46244=CARTESIAN_POINT('Ctrl Pts',(-98.2494587013773,-100.545329747157,
178.585485043865));
#46245=CARTESIAN_POINT('Ctrl Pts',(-98.3115349193939,-100.768593902497,
178.585485055673));
#46246=CARTESIAN_POINT('Ctrl Pts',(-98.3765170572738,-100.991065637145,
178.585485062744));
#46247=CARTESIAN_POINT('Origin',(-93.2994946198038,-77.3496518591637,173.385485069079));
#46248=CARTESIAN_POINT('',(-97.9019633317937,-101.167776319221,173.385485069079));
#46249=CARTESIAN_POINT('Origin',(-98.8390996009304,-100.818812692078,173.385485069079));
#46250=CARTESIAN_POINT('',(-98.376517057274,-100.991065637145,173.385485071191));
#46251=CARTESIAN_POINT('',(-99.2720912023343,-100.657578595475,173.385485069079));
#46252=CARTESIAN_POINT('Ctrl Pts',(-98.3765170572737,-100.991065637145,
173.385485075415));
#46253=CARTESIAN_POINT('Ctrl Pts',(-98.311534919394,-100.768593902497,173.385485082486));
#46254=CARTESIAN_POINT('Ctrl Pts',(-98.2494587013798,-100.545329747159,
173.385485094294));
#46255=CARTESIAN_POINT('Ctrl Pts',(-98.1886188504344,-100.321776749251,
173.38548510303));
#46256=CARTESIAN_POINT('Ctrl Pts',(-98.0726679597014,-99.8957209843114,
173.38548511968));
#46257=CARTESIAN_POINT('Ctrl Pts',(-97.9614492780947,-99.4685356861606,
173.385485114302));
#46258=CARTESIAN_POINT('Ctrl Pts',(-97.8524422630192,-99.0407060185016,
173.385485090321));
#46259=CARTESIAN_POINT('Ctrl Pts',(-97.7888472641501,-98.7911089883279,
173.385485076331));
#46260=CARTESIAN_POINT('Ctrl Pts',(-97.7260872514046,-98.5412846698841,
173.385485075368));
#46261=CARTESIAN_POINT('Ctrl Pts',(-97.6636749002385,-98.2913808726465,
173.38548507567));
#46262=CARTESIAN_POINT('Ctrl Pts',(-97.5629746719806,-97.8881695057594,
173.385485076157));
#46263=CARTESIAN_POINT('Ctrl Pts',(-97.4633229695275,-97.4847035044845,
173.385485083822));
#46264=CARTESIAN_POINT('Ctrl Pts',(-97.3642924294252,-97.0810624897179,
173.385485113046));
#46265=CARTESIAN_POINT('Ctrl Pts',(-97.129868327764,-96.1255675264219,173.385485182225));
#46266=CARTESIAN_POINT('Ctrl Pts',(-96.8983471324719,-95.1692940408548,
173.385485100813));
#46267=CARTESIAN_POINT('Ctrl Pts',(-96.6655567819617,-94.2133925591637,
173.385485086277));
#46268=CARTESIAN_POINT('Ctrl Pts',(-96.5797668758502,-93.8611155073597,
173.38548508092));
#46269=CARTESIAN_POINT('Ctrl Pts',(-96.4938533034791,-93.5088728518748,
173.385485079216));
#46270=CARTESIAN_POINT('Ctrl Pts',(-96.4078010227867,-93.1566576401016,
173.385485091048));
#46271=CARTESIAN_POINT('Ctrl Pts',(-95.9247643984986,-91.1795706233595,
173.385485157466));
#46272=CARTESIAN_POINT('Ctrl Pts',(-95.4349837366555,-89.2040886563437,
173.385485090674));
#46273=CARTESIAN_POINT('Ctrl Pts',(-94.9311314986831,-87.2324375352915,
173.385485075759));
#46274=CARTESIAN_POINT('Ctrl Pts',(-94.8320499884367,-86.844716382084,173.385485072826));
#46275=CARTESIAN_POINT('Ctrl Pts',(-94.7324241658693,-86.4571433323539,
173.38548507155));
#46276=CARTESIAN_POINT('Ctrl Pts',(-94.6321980466999,-86.0697352205311,
173.385485071057));
#46277=CARTESIAN_POINT('Ctrl Pts',(-94.567745275975,-85.8206032934928,173.38548507074));
#46278=CARTESIAN_POINT('Ctrl Pts',(-94.5030528267687,-85.5715226067371,
173.38548507072));
#46279=CARTESIAN_POINT('Ctrl Pts',(-94.4381163838136,-85.3224975248463,
173.385485071108));
#46280=CARTESIAN_POINT('Ctrl Pts',(-93.8936936520863,-83.2346881348964,
173.385485074359));
#46281=CARTESIAN_POINT('Ctrl Pts',(-93.3315556794994,-81.1505590794656,
173.385485075867));
#46282=CARTESIAN_POINT('Ctrl Pts',(-92.7483148961997,-79.0730496714838,
173.385485074267));
#46283=CARTESIAN_POINT('Ctrl Pts',(-92.1887794724172,-77.0799789873133,
173.385485072732));
#46284=CARTESIAN_POINT('Ctrl Pts',(-91.6098219083077,-75.0930006983604,
173.385485070307));
#46285=CARTESIAN_POINT('Ctrl Pts',(-91.0084120392233,-73.1147375455329,
173.385485069579));
#46286=CARTESIAN_POINT('Ctrl Pts',(-90.6894518180546,-72.0655574685308,
173.385485069193));
#46287=CARTESIAN_POINT('Ctrl Pts',(-90.3641756334622,-71.0188292236311,
173.385485069122));
#46288=CARTESIAN_POINT('Ctrl Pts',(-90.0321265335055,-69.9749475293908,
173.385485069101));
#46289=CARTESIAN_POINT('Ctrl Pts',(-90.0140193906523,-69.9180230716466,
173.3854850691));
#46290=CARTESIAN_POINT('Ctrl Pts',(-89.9958921332871,-69.8611066569696,
173.385485069099));
#46291=CARTESIAN_POINT('Ctrl Pts',(-89.9777446627662,-69.8041983278482,
173.385485069098));
#46292=CARTESIAN_POINT('Ctrl Pts',(-89.4241644259319,-68.068235937028,173.385485069073));
#46293=CARTESIAN_POINT('Ctrl Pts',(-88.8517488584057,-66.3397526068269,
173.385485069079));
#46294=CARTESIAN_POINT('Ctrl Pts',(-88.2576270599827,-64.6198876182801,
173.38548506908));
#46295=CARTESIAN_POINT('Ctrl Pts',(-87.9757272049345,-63.8038433454379,
173.38548506908));
#46296=CARTESIAN_POINT('Ctrl Pts',(-87.6889399119433,-62.9897396575733,
173.385485069081));
#46297=CARTESIAN_POINT('Ctrl Pts',(-87.3969547526246,-62.1777000567284,
173.385485069083));
#46298=CARTESIAN_POINT('Ctrl Pts',(-87.3869476469948,-62.1498693064251,
173.385485069083));
#46299=CARTESIAN_POINT('Ctrl Pts',(-87.3769344349743,-62.1220409827925,
173.385485069083));
#46300=CARTESIAN_POINT('Ctrl Pts',(-87.3669151039254,-62.0942150904507,
173.385485069083));
#46301=CARTESIAN_POINT('Ctrl Pts',(-86.8314975075075,-60.6072423251777,
173.385485069087));
#46302=CARTESIAN_POINT('Ctrl Pts',(-86.278660184972,-59.1271866439569,173.385485069082));
#46303=CARTESIAN_POINT('Ctrl Pts',(-85.7057349163769,-57.6551066868731,
173.385485069093));
#46304=CARTESIAN_POINT('Ctrl Pts',(-85.317269307623,-56.6569792381303,173.3854850691));
#46305=CARTESIAN_POINT('Ctrl Pts',(-84.9195676645059,-55.6625189265031,
173.385485069105));
#46306=CARTESIAN_POINT('Ctrl Pts',(-84.5117857638601,-54.6720615186052,
173.385485069208));
#46307=CARTESIAN_POINT('Ctrl Pts',(-84.4696325489975,-54.569675993742,173.385485069218));
#46308=CARTESIAN_POINT('Ctrl Pts',(-84.4273715190409,-54.4673333389783,
173.385485069228));
#46309=CARTESIAN_POINT('Ctrl Pts',(-84.3850017277721,-54.3650338933295,
173.385485069237));
#46310=CARTESIAN_POINT('Ctrl Pts',(-83.8751948703674,-53.1341342986271,
173.385485069345));
#46311=CARTESIAN_POINT('Ctrl Pts',(-83.3497144088603,-51.9094558257061,
173.385485069266));
#46312=CARTESIAN_POINT('Ctrl Pts',(-82.8060894939277,-50.6919817529054,
173.385485069267));
#46313=CARTESIAN_POINT('Ctrl Pts',(-82.3011625525949,-49.5611736481895,
173.385485069268));
#46314=CARTESIAN_POINT('Ctrl Pts',(-81.7805823269495,-48.4365808302589,
173.385485069152));
#46315=CARTESIAN_POINT('Ctrl Pts',(-81.2423319510283,-47.3190072870549,
173.385485070025));
#46316=CARTESIAN_POINT('Ctrl Pts',(-81.1632479651373,-47.15480457717,173.385485070154));
#46317=CARTESIAN_POINT('Ctrl Pts',(-81.0837898722368,-46.9907506072374,
173.38548507058));
#46318=CARTESIAN_POINT('Ctrl Pts',(-81.003949606998,-46.8268481729707,173.385485071939));
#46319=CARTESIAN_POINT('Ctrl Pts',(-80.5434162035343,-45.8814286448278,
173.385485079774));
#46320=CARTESIAN_POINT('Ctrl Pts',(-80.0700920299859,-44.9410842957925,
173.385485162657));
#46321=CARTESIAN_POINT('Ctrl Pts',(-79.5818989661386,-44.0066238667974,
173.385485368229));
#46322=CARTESIAN_POINT('Ctrl Pts',(-79.4318508819061,-43.7194137289541,
173.385485431413));
#46323=CARTESIAN_POINT('Ctrl Pts',(-79.2803980192546,-43.432759748701,173.385485500516));
#46324=CARTESIAN_POINT('Ctrl Pts',(-79.1274796035642,-43.1466863215074,
173.385485561525));
#46325=CARTESIAN_POINT('Ctrl Pts',(-78.8029288442143,-42.5395302271525,
173.38548569101));
#46326=CARTESIAN_POINT('Ctrl Pts',(-78.4717618076259,-41.9349956915895,
173.385485772917));
#46327=CARTESIAN_POINT('Ctrl Pts',(-78.1332843656745,-41.3333760529103,
173.385485686161));
#46328=CARTESIAN_POINT('Ctrl Pts',(-77.9138848638038,-40.9434090043507,
173.385485629926));
#46329=CARTESIAN_POINT('Ctrl Pts',(-77.6905814020163,-40.5551270056959,
173.385485500739));
#46330=CARTESIAN_POINT('Ctrl Pts',(-77.4650015118694,-40.1676234768323,
173.385485354513));
#46331=CARTESIAN_POINT('Ctrl Pts',(-78.158666194104,-39.3728065519909,177.585485069079));
#46332=CARTESIAN_POINT('Ctrl Pts',(-78.158666194104,-39.3728065519909,173.745485069079));
#46333=CARTESIAN_POINT('Ctrl Pts',(-91.6625086178529,-62.3675309666402,
177.585485069079));
#46334=CARTESIAN_POINT('Ctrl Pts',(-91.6625086178529,-62.3675309666402,
173.745485069079));
#46335=CARTESIAN_POINT('Ctrl Pts',(-97.8762366937634,-96.9090335189287,
177.585485069079));
#46336=CARTESIAN_POINT('Ctrl Pts',(-97.8762366937634,-96.9090335189287,
173.745485069079));
#46337=CARTESIAN_POINT('Ctrl Pts',(-99.6210548294771,-101.594714864612,
177.585485069079));
#46338=CARTESIAN_POINT('Ctrl Pts',(-99.6210548294771,-101.594714864612,
173.745485069079));
#46339=CARTESIAN_POINT('Ctrl Pts',(-78.158666194104,-39.372806551991,174.385485069079));
#46340=CARTESIAN_POINT('Ctrl Pts',(-79.5634562342768,-41.7649227231192,
174.385485069079));
#46341=CARTESIAN_POINT('Ctrl Pts',(-80.8467635159852,-44.2054723433059,
174.385485069079));
#46342=CARTESIAN_POINT('Ctrl Pts',(-83.2418725976757,-49.1549483814856,
174.385485069079));
#46343=CARTESIAN_POINT('Ctrl Pts',(-84.3529474705451,-51.6641646149859,
174.385485069079));
#46344=CARTESIAN_POINT('Ctrl Pts',(-86.4442463955118,-56.7347654443307,
174.385485069079));
#46345=CARTESIAN_POINT('Ctrl Pts',(-87.4241628164095,-59.2962726883618,
174.385485069079));
#46346=CARTESIAN_POINT('Ctrl Pts',(-89.2799424409765,-64.4607717151331,
174.385485069079));
#46347=CARTESIAN_POINT('Ctrl Pts',(-90.1556460538296,-67.0638271244634,
174.385485069079));
#46348=CARTESIAN_POINT('Ctrl Pts',(-92.6553603269606,-74.9237845522913,
174.385485069079));
#46349=CARTESIAN_POINT('Ctrl Pts',(-94.1520335629162,-80.2352141170513,
174.385485069079));
#46350=CARTESIAN_POINT('Ctrl Pts',(-96.2277705472134,-88.2383598976106,
174.385485069079));
#46351=CARTESIAN_POINT('Ctrl Pts',(-96.8905903551983,-90.913701399124,174.385485069079));
#46352=CARTESIAN_POINT('Ctrl Pts',(-97.8694497883241,-94.9305941684308,
174.385485069079));
#46353=CARTESIAN_POINT('Ctrl Pts',(-98.1926873948002,-96.27033732199,174.385485069079));
#46354=CARTESIAN_POINT('Ctrl Pts',(-98.6897521666471,-98.2768331740868,
174.385485069079));
#46355=CARTESIAN_POINT('Ctrl Pts',(-98.8572817108174,-98.9451947300226,
174.385485069079));
#46356=CARTESIAN_POINT('Ctrl Pts',(-99.1212462758668,-99.9445001871973,
174.385485069079));
#46357=CARTESIAN_POINT('Ctrl Pts',(-99.2113105712096,-100.277071621847,
174.385485069079));
#46358=CARTESIAN_POINT('Ctrl Pts',(-99.4021032609997,-100.939490126788,
174.385485069079));
#46359=CARTESIAN_POINT('Ctrl Pts',(-99.500148440254,-101.270022679816,174.385485069079));
#46360=CARTESIAN_POINT('Ctrl Pts',(-99.6210548294771,-101.594714864612,
174.385485069079));
#46361=CARTESIAN_POINT('Ctrl Pts',(-99.6210548294771,-101.594714864612,
177.585485069079));
#46362=CARTESIAN_POINT('Ctrl Pts',(-99.5610285400747,-101.433515219282,
177.585485069079));
#46363=CARTESIAN_POINT('Ctrl Pts',(-99.5069208217296,-101.268946229191,
177.585485069079));
#46364=CARTESIAN_POINT('Ctrl Pts',(-99.4038032743778,-100.940304890532,
177.585485069079));
#46365=CARTESIAN_POINT('Ctrl Pts',(-99.3548261927294,-100.775311081876,
177.585485069079));
#46366=CARTESIAN_POINT('Ctrl Pts',(-99.2119254375992,-100.279278763247,
177.585485069079));
#46367=CARTESIAN_POINT('Ctrl Pts',(-99.1219766295885,-99.9472038638691,
177.585485069079));
#46368=CARTESIAN_POINT('Ctrl Pts',(-98.8583492039865,-98.9493576507077,
177.585485069079));
#46369=CARTESIAN_POINT('Ctrl Pts',(-98.691030413114,-98.2819281029329,177.585485069079));
#46370=CARTESIAN_POINT('Ctrl Pts',(-98.1946027213088,-96.2781979350422,
177.585485069079));
#46371=CARTESIAN_POINT('Ctrl Pts',(-97.8717928229948,-94.9402549399502,
177.585485069079));
#46372=CARTESIAN_POINT('Ctrl Pts',(-96.8942898157684,-90.9287916912753,
177.585485069079));
#46373=CARTESIAN_POINT('Ctrl Pts',(-96.2324745724884,-88.2571284325171,
177.585485069079));
#46374=CARTESIAN_POINT('Ctrl Pts',(-94.1600380638105,-80.2648202595016,
177.585485069079));
#46375=CARTESIAN_POINT('Ctrl Pts',(-92.6665566865773,-74.9615276259966,
177.585485069079));
#46376=CARTESIAN_POINT('Ctrl Pts',(-90.1657169570279,-67.0942364364973,
177.585485069079));
#46377=CARTESIAN_POINT('Ctrl Pts',(-89.289147208604,-64.4872953405147,177.585485069079));
#46378=CARTESIAN_POINT('Ctrl Pts',(-87.4300065178477,-59.3116351672732,
177.585485069079));
#46379=CARTESIAN_POINT('Ctrl Pts',(-86.4476068577322,-56.7428543288977,
177.585485069079));
#46380=CARTESIAN_POINT('Ctrl Pts',(-84.3486009704813,-51.6536849931039,
177.585485069079));
#46381=CARTESIAN_POINT('Ctrl Pts',(-83.2324817482337,-49.1343169853156,
177.585485069079));
#46382=CARTESIAN_POINT('Ctrl Pts',(-80.8356389933579,-44.1837194009194,
177.585485069079));
#46383=CARTESIAN_POINT('Ctrl Pts',(-79.554497878766,-41.7496681822473,177.585485069079));
#46384=CARTESIAN_POINT('Ctrl Pts',(-78.158666194104,-39.372806551991,177.585485069079));
#46385=CARTESIAN_POINT('Ctrl Pts',(-97.8838106736817,-101.114486609555,
178.585485069079));
#46386=CARTESIAN_POINT('Ctrl Pts',(-97.8838106736817,-101.114486609555,
177.402158081293));
#46387=CARTESIAN_POINT('Ctrl Pts',(-96.3541371085078,-96.1722845480715,
178.585485069079));
#46388=CARTESIAN_POINT('Ctrl Pts',(-96.3541371085078,-96.1722845480715,
177.402158081293));
#46389=CARTESIAN_POINT('Ctrl Pts',(-91.1365269123698,-76.1991465747503,
178.585485069079));
#46390=CARTESIAN_POINT('Ctrl Pts',(-91.1365269123698,-76.1991465747503,
177.402158081293));
#46391=CARTESIAN_POINT('Ctrl Pts',(-87.1439910232441,-64.4286763559758,
178.585485069079));
#46392=CARTESIAN_POINT('Ctrl Pts',(-87.1439910232441,-64.4286763559758,
177.402158081293));
#46393=CARTESIAN_POINT('Ctrl Pts',(-83.9950826197058,-63.9298573380069,
178.585485069079));
#46394=CARTESIAN_POINT('Ctrl Pts',(-83.9950826197058,-63.9298573380069,
177.402158081293));
#46395=CARTESIAN_POINT('Ctrl Pts',(-81.9013008568494,-58.3070397231869,
178.585485069079));
#46396=CARTESIAN_POINT('Ctrl Pts',(-81.9013008568494,-58.3070397231869,
177.402158081293));
#46397=CARTESIAN_POINT('',(-97.8838106717876,-101.114486603436,177.605254289888));
#46398=CARTESIAN_POINT('',(-97.8838106722024,-101.114486604776,178.585485069079));
#46399=CARTESIAN_POINT('',(-94.2301013700811,-88.1262479603857,177.685485027504));
#46400=CARTESIAN_POINT('Ctrl Pts',(-97.8838106717875,-101.114486603435,
177.605254289869));
#46401=CARTESIAN_POINT('Ctrl Pts',(-97.5030442961786,-99.8842735631011,
177.614491023905));
#46402=CARTESIAN_POINT('Ctrl Pts',(-96.9354756924371,-97.8900545660898,
177.647854393757));
#46403=CARTESIAN_POINT('Ctrl Pts',(-95.4293955181978,-92.466558256121,177.681831570023));
#46404=CARTESIAN_POINT('Ctrl Pts',(-94.8572393589048,-90.3892421799639,
177.685464318439));
#46405=CARTESIAN_POINT('Ctrl Pts',(-94.2301013700974,-88.1262479603808,
177.685484985585));
#46406=CARTESIAN_POINT('',(-81.9013008568494,-58.3070397231869,177.685485069079));
#46407=CARTESIAN_POINT('Ctrl Pts',(-94.230101370093,-88.1262479603649,177.685485069079));
#46408=CARTESIAN_POINT('Ctrl Pts',(-92.4302378087522,-81.6315356194686,
177.685485069079));
#46409=CARTESIAN_POINT('Ctrl Pts',(-89.7937145858072,-72.240376274837,177.685485069079));
#46410=CARTESIAN_POINT('Ctrl Pts',(-87.1439910232441,-64.4286763559758,
177.685485069079));
#46411=CARTESIAN_POINT('Ctrl Pts',(-83.9950826197058,-63.9298573380069,
177.685485069079));
#46412=CARTESIAN_POINT('Ctrl Pts',(-81.9013008568494,-58.3070397231869,
177.685485069079));
#46413=CARTESIAN_POINT('',(-81.9013008568494,-58.3070397231869,178.585485069079));
#46414=CARTESIAN_POINT('Origin',(-48.2819354919502,-57.24716229829,178.585485069079));
#46415=CARTESIAN_POINT('',(-80.6956086449674,-48.2616817644643,177.685485069079));
#46416=CARTESIAN_POINT('Origin',(-48.2819354919502,-57.24716229829,177.685485069079));
#46417=CARTESIAN_POINT('Ctrl Pts',(-80.6956086449673,-48.2616817644641,
177.685485069056));
#46418=CARTESIAN_POINT('Ctrl Pts',(-80.3006668909431,-46.8369930256451,
177.685486806981));
#46419=CARTESIAN_POINT('Ctrl Pts',(-79.7866389024401,-45.3484842121757,
177.588631574318));
#46420=CARTESIAN_POINT('Ctrl Pts',(-78.8133875980925,-43.1109905505337,
177.458866873764));
#46421=CARTESIAN_POINT('Ctrl Pts',(-78.4747061907265,-42.4011423672079,
177.420903726026));
#46422=CARTESIAN_POINT('Ctrl Pts',(-77.9051062662601,-41.3082355829664,
177.386258249981));
#46423=CARTESIAN_POINT('Ctrl Pts',(-77.6960535523287,-40.9258180515529,
177.379106567025));
#46424=CARTESIAN_POINT('Ctrl Pts',(-77.3957878325661,-40.4008992054676,
177.376311192626));
#46425=CARTESIAN_POINT('Ctrl Pts',(-77.3118277525961,-40.2566253440053,
177.376311556297));
#46426=CARTESIAN_POINT('Ctrl Pts',(-77.1764463001175,-40.0279274943117,
177.377893715319));
#46427=CARTESIAN_POINT('Ctrl Pts',(-77.1258588542569,-39.9433224560675,
177.378826264229));
#46428=CARTESIAN_POINT('Ctrl Pts',(-77.0748911463744,-39.8589256891122,
177.380140939181));
#46429=CARTESIAN_POINT('Origin',(-93.2994946198038,-77.3496518591637,177.685485069079));
#46430=CARTESIAN_POINT('Ctrl Pts',(-94.2301013700599,-88.1262479603733,
177.685484985585));
#46431=CARTESIAN_POINT('Ctrl Pts',(-93.7609037487217,-86.2787775829358,
177.685484911581));
#46432=CARTESIAN_POINT('Ctrl Pts',(-93.2798504860541,-84.4344939240166,
177.68548504784));
#46433=CARTESIAN_POINT('Ctrl Pts',(-92.7836854151622,-82.5942786034907,
177.685485064168));
#46434=CARTESIAN_POINT('Ctrl Pts',(-92.6359385547694,-82.0463036411146,
177.68548506903));
#46435=CARTESIAN_POINT('Ctrl Pts',(-92.4868514135393,-81.4986892569901,
177.685485068967));
#46436=CARTESIAN_POINT('Ctrl Pts',(-92.3363371949808,-80.9514582278748,
177.685485069002));
#46437=CARTESIAN_POINT('Ctrl Pts',(-92.3269664573115,-80.917388633205,177.685485069004));
#46438=CARTESIAN_POINT('Ctrl Pts',(-92.317590034494,-80.883320423089,177.685485069007));
#46439=CARTESIAN_POINT('Ctrl Pts',(-92.3082079016947,-80.849253605753,177.685485069009));
#46440=CARTESIAN_POINT('Ctrl Pts',(-91.7304217636379,-78.751294085718,177.685485069135));
#46441=CARTESIAN_POINT('Ctrl Pts',(-91.1316580244191,-76.6586040978249,
177.685485069079));
#46442=CARTESIAN_POINT('Ctrl Pts',(-90.5086916305028,-74.5750064731804,
177.685485069079));
#46443=CARTESIAN_POINT('Ctrl Pts',(-90.4336469891343,-74.324009247608,177.685485069079));
#46444=CARTESIAN_POINT('Ctrl Pts',(-90.3582510931399,-74.0731440131607,
177.685485069079));
#46445=CARTESIAN_POINT('Ctrl Pts',(-90.2824982722455,-73.8224174920625,
177.685485069079));
#46446=CARTESIAN_POINT('Ctrl Pts',(-89.917539583476,-72.6144780213029,177.685485069079));
#46447=CARTESIAN_POINT('Ctrl Pts',(-89.5441964515263,-71.409423930501,177.685485069079));
#46448=CARTESIAN_POINT('Ctrl Pts',(-89.1617955303327,-70.2079449176487,
177.685485069079));
#46449=CARTESIAN_POINT('Ctrl Pts',(-88.6527415452668,-68.6085301527561,
177.685485069079));
#46450=CARTESIAN_POINT('Ctrl Pts',(-88.1276036690571,-67.0148515066794,
177.685485069079));
#46451=CARTESIAN_POINT('Ctrl Pts',(-87.5839489126203,-65.4278719429401,
177.685485069079));
#46452=CARTESIAN_POINT('Ctrl Pts',(-87.0553314119355,-63.8847875484985,
177.685485069079));
#46453=CARTESIAN_POINT('Ctrl Pts',(-86.5092073119288,-62.34803672185,177.685485069079));
#46454=CARTESIAN_POINT('Ctrl Pts',(-85.9432952559966,-60.8185262246806,
177.685485069079));
#46455=CARTESIAN_POINT('Ctrl Pts',(-85.8157986536034,-60.4739366552068,
177.685485069079));
#46456=CARTESIAN_POINT('Ctrl Pts',(-85.6872974782193,-60.129714676371,177.685485069079));
#46457=CARTESIAN_POINT('Ctrl Pts',(-85.5577653075821,-59.7858708180288,
177.685485069079));
#46458=CARTESIAN_POINT('Ctrl Pts',(-84.9035795890701,-58.0758081979705,
177.685485069079));
#46459=CARTESIAN_POINT('Ctrl Pts',(-84.4380969044864,-56.8776880926409,
177.685485069079));
#46460=CARTESIAN_POINT('Ctrl Pts',(-83.9593907228013,-55.6843887421588,
177.685485069075));
#46461=CARTESIAN_POINT('Ctrl Pts',(-83.4654560220973,-54.4966313344464,
177.685485068972));
#46462=CARTESIAN_POINT('Ctrl Pts',(-82.9903344236191,-53.3541135130576,
177.685485068874));
#46463=CARTESIAN_POINT('Ctrl Pts',(-82.5011223788676,-52.2167234425755,
177.685485068703));
#46464=CARTESIAN_POINT('Ctrl Pts',(-81.9959927121058,-51.0851245641857,
177.685485068751));
#46465=CARTESIAN_POINT('Ctrl Pts',(-81.6680421620932,-50.3504449383769,
177.685485068781));
#46466=CARTESIAN_POINT('Ctrl Pts',(-81.3333812632274,-49.6182068120372,
177.685485068931));
#46467=CARTESIAN_POINT('Ctrl Pts',(-80.991499413137,-48.8885971288398,177.68548506903));
#46468=CARTESIAN_POINT('Ctrl Pts',(-80.8934759176747,-48.6794052941422,
177.685485069058));
#46469=CARTESIAN_POINT('Ctrl Pts',(-80.794854333503,-48.4704314543238,177.685485069079));
#46470=CARTESIAN_POINT('Ctrl Pts',(-80.6956167008178,-48.2616828347543,
177.685485069079));
#46471=CARTESIAN_POINT('Origin',(-93.2994946198038,-77.3496518591637,174.285485069079));
#46472=CARTESIAN_POINT('Ctrl Pts',(-80.695616700829,-48.261682834749,174.285485069079));
#46473=CARTESIAN_POINT('Ctrl Pts',(-80.7948543335137,-48.4704314543193,
174.285485069079));
#46474=CARTESIAN_POINT('Ctrl Pts',(-80.8934759176831,-48.6794052941381,
174.2854850691));
#46475=CARTESIAN_POINT('Ctrl Pts',(-80.9914994131414,-48.888597128836,174.285485069129));
#46476=CARTESIAN_POINT('Ctrl Pts',(-81.5156771503982,-50.007244265953,174.28548506928));
#46477=CARTESIAN_POINT('Ctrl Pts',(-82.0228825597661,-51.1320690378344,
174.285485069461));
#46478=CARTESIAN_POINT('Ctrl Pts',(-82.5149477029265,-52.2624018736989,
174.285485069392));
#46479=CARTESIAN_POINT('Ctrl Pts',(-83.0257505562677,-53.4357774842463,
174.28548506932));
#46480=CARTESIAN_POINT('Ctrl Pts',(-83.5202380124723,-54.615088703677,174.28548506915));
#46481=CARTESIAN_POINT('Ctrl Pts',(-84.0004086366806,-55.7996123684871,
174.285485069105));
#46482=CARTESIAN_POINT('Ctrl Pts',(-84.3071383529486,-56.556277997958,174.285485069076));
#46483=CARTESIAN_POINT('Ctrl Pts',(-84.6080249651107,-57.3150711201698,
174.285485069079));
#46484=CARTESIAN_POINT('Ctrl Pts',(-84.9035795890703,-58.0758081979706,
174.285485069079));
#46485=CARTESIAN_POINT('Ctrl Pts',(-85.5577653075812,-59.7858708180264,
174.285485069079));
#46486=CARTESIAN_POINT('Ctrl Pts',(-86.1320133072127,-61.3102152867964,
174.285485069079));
#46487=CARTESIAN_POINT('Ctrl Pts',(-86.6860022344115,-62.8419893984846,
174.285485069079));
#46488=CARTESIAN_POINT('Ctrl Pts',(-87.2220157058671,-64.3802846100018,
174.285485069079));
#46489=CARTESIAN_POINT('Ctrl Pts',(-87.772984453019,-65.9614996924093,174.285485069079));
#46490=CARTESIAN_POINT('Ctrl Pts',(-88.3049605725574,-67.5496048953572,
174.285485069079));
#46491=CARTESIAN_POINT('Ctrl Pts',(-88.8203747377026,-69.1436372841121,
174.285485069079));
#46492=CARTESIAN_POINT('Ctrl Pts',(-88.9349920760239,-69.4981167725554,
174.285485069079));
#46493=CARTESIAN_POINT('Ctrl Pts',(-89.0487902001326,-69.8528894638316,
174.285485069079));
#46494=CARTESIAN_POINT('Ctrl Pts',(-89.1617955303599,-70.207944917638,174.285485069079));
#46495=CARTESIAN_POINT('Ctrl Pts',(-89.5441964515462,-71.4094239304843,
174.285485069079));
#46496=CARTESIAN_POINT('Ctrl Pts',(-89.9175395834869,-72.6144780212793,
174.285485069079));
#46497=CARTESIAN_POINT('Ctrl Pts',(-90.2824982722559,-73.8224174920276,
174.285485069079));
#46498=CARTESIAN_POINT('Ctrl Pts',(-90.9113434606063,-75.9037679225675,
174.285485069079));
#46499=CARTESIAN_POINT('Ctrl Pts',(-91.5155952534419,-77.9946739428601,
174.285485069044));
#46500=CARTESIAN_POINT('Ctrl Pts',(-92.098482701032,-80.0913078783335,174.285485069115));
#46501=CARTESIAN_POINT('Ctrl Pts',(-92.1686992971666,-80.3438755033487,
174.285485069124));
#46502=CARTESIAN_POINT('Ctrl Pts',(-92.2386058266307,-80.5965262964667,
174.285485069135));
#46503=CARTESIAN_POINT('Ctrl Pts',(-92.308207901702,-80.8492536057496,174.28548506915));
#46504=CARTESIAN_POINT('Ctrl Pts',(-92.3175900344974,-80.8833204230718,
174.285485069152));
#46505=CARTESIAN_POINT('Ctrl Pts',(-92.326966457311,-80.9173886331741,174.285485069154));
#46506=CARTESIAN_POINT('Ctrl Pts',(-92.3363371949764,-80.95145822783,174.285485069157));
#46507=CARTESIAN_POINT('Ctrl Pts',(-92.8417956348715,-82.7891752547728,
174.285485069276));
#46508=CARTESIAN_POINT('Ctrl Pts',(-93.3311638475814,-84.6312179529252,
174.285485143859));
#46509=CARTESIAN_POINT('Ctrl Pts',(-93.8077114875544,-86.4767126138309,
174.285485171775));
#46510=CARTESIAN_POINT('Ctrl Pts',(-93.9496167188407,-87.0262596574556,
174.285485180087));
#46511=CARTESIAN_POINT('Ctrl Pts',(-94.0903848106434,-87.5761125951912,
174.28548517461));
#46512=CARTESIAN_POINT('Ctrl Pts',(-94.2301013700444,-88.1262479603172,
174.285485152574));
#46513=CARTESIAN_POINT('Ctrl Pts',(-77.3304501603129,-39.7397688129298,
177.705885069079));
#46514=CARTESIAN_POINT('Ctrl Pts',(-77.3304501603129,-39.7397688129298,
173.576925069079));
#46515=CARTESIAN_POINT('Ctrl Pts',(-77.4354809475772,-39.918618205007,177.705885069079));
#46516=CARTESIAN_POINT('Ctrl Pts',(-77.4354809475772,-39.918618205007,173.576925069079));
#46517=CARTESIAN_POINT('Ctrl Pts',(-77.5387174074033,-40.095017410943,177.705885069079));
#46518=CARTESIAN_POINT('Ctrl Pts',(-77.5387174074033,-40.095017410943,173.576925069079));
#46519=CARTESIAN_POINT('Ctrl Pts',(-77.7452188224523,-40.4514138749057,
177.705885069079));
#46520=CARTESIAN_POINT('Ctrl Pts',(-77.7452188224523,-40.4514138749057,
173.576925069079));
#46521=CARTESIAN_POINT('Ctrl Pts',(-78.0537048438588,-40.988104564515,177.705885069079));
#46522=CARTESIAN_POINT('Ctrl Pts',(-78.0537048438588,-40.988104564515,173.576925069079));
#46523=CARTESIAN_POINT('Ctrl Pts',(-78.7646561081799,-42.2546401779696,
177.705885069079));
#46524=CARTESIAN_POINT('Ctrl Pts',(-78.7646561081799,-42.2546401779696,
173.576925069079));
#46525=CARTESIAN_POINT('Ctrl Pts',(-79.358919965841,-43.3632613763041,177.705885069079));
#46526=CARTESIAN_POINT('Ctrl Pts',(-79.358919965841,-43.3632613763041,173.576925069079));
#46527=CARTESIAN_POINT('Ctrl Pts',(-80.5274284163852,-45.6074041562991,
177.705885069079));
#46528=CARTESIAN_POINT('Ctrl Pts',(-80.5274284163852,-45.6074041562991,
173.576925069079));
#46529=CARTESIAN_POINT('Ctrl Pts',(-81.2797370189181,-47.139365595286,177.705885069079));
#46530=CARTESIAN_POINT('Ctrl Pts',(-81.2797370189181,-47.139365595286,173.576925069079));
#46531=CARTESIAN_POINT('Ctrl Pts',(-83.4579294386781,-51.8125322088705,
177.705885069079));
#46532=CARTESIAN_POINT('Ctrl Pts',(-83.4579294386781,-51.8125322088705,
173.576925069079));
#46533=CARTESIAN_POINT('Ctrl Pts',(-84.8050389597313,-55.0309990672248,
177.705885069079));
#46534=CARTESIAN_POINT('Ctrl Pts',(-84.8050389597313,-55.0309990672248,
173.576925069079));
#46535=CARTESIAN_POINT('Ctrl Pts',(-88.5443259067898,-64.7535560405655,
177.705885069079));
#46536=CARTESIAN_POINT('Ctrl Pts',(-88.5443259067898,-64.7535560405655,
173.576925069079));
#46537=CARTESIAN_POINT('Ctrl Pts',(-90.6342709141923,-71.3245283131479,
177.705885069079));
#46538=CARTESIAN_POINT('Ctrl Pts',(-90.6342709141923,-71.3245283131479,
173.576925069079));
#46539=CARTESIAN_POINT('Ctrl Pts',(-94.0886049589878,-83.3618611533263,
177.705885069079));
#46540=CARTESIAN_POINT('Ctrl Pts',(-94.0886049589878,-83.3618611533263,
173.576925069079));
#46541=CARTESIAN_POINT('Ctrl Pts',(-95.4530208414653,-88.8276309456242,
177.705885069079));
#46542=CARTESIAN_POINT('Ctrl Pts',(-95.4530208414653,-88.8276309456242,
173.576925069079));
#46543=CARTESIAN_POINT('Ctrl Pts',(-97.0209399293013,-95.2453104772289,
177.705885069079));
#46544=CARTESIAN_POINT('Ctrl Pts',(-97.0209399293013,-95.2453104772289,
173.576925069079));
#46545=CARTESIAN_POINT('Ctrl Pts',(-97.4636939970592,-97.0873928564593,
177.705885069079));
#46546=CARTESIAN_POINT('Ctrl Pts',(-97.4636939970592,-97.0873928564593,
173.576925069079));
#46547=CARTESIAN_POINT('Ctrl Pts',(-98.0183678164048,-99.2934349167345,
177.705885069079));
#46548=CARTESIAN_POINT('Ctrl Pts',(-98.0183678164048,-99.2934349167345,
173.576925069079));
#46549=CARTESIAN_POINT('Ctrl Pts',(-98.1849688704148,-99.9358635919993,
177.705885069079));
#46550=CARTESIAN_POINT('Ctrl Pts',(-98.1849688704148,-99.9358635919993,
173.576925069079));
#46551=CARTESIAN_POINT('Ctrl Pts',(-98.485392535511,-101.02211760146,177.705885069079));
#46552=CARTESIAN_POINT('Ctrl Pts',(-98.485392535511,-101.02211760146,173.576925069079));
#46553=CARTESIAN_POINT('Ctrl Pts',(-98.6178709133345,-101.46363133471,177.705885069079));
#46554=CARTESIAN_POINT('Ctrl Pts',(-98.6178709133345,-101.46363133471,173.576925069079));
#46555=CARTESIAN_POINT('Ctrl Pts',(-98.7431461249941,-101.814198511965,
177.705885069079));
#46556=CARTESIAN_POINT('Ctrl Pts',(-98.7431461249941,-101.814198511965,
173.576925069079));
#46557=CARTESIAN_POINT('',(-85.8357031165434,-57.713668075261,176.685485069079));
#46558=CARTESIAN_POINT('Ctrl Pts',(-77.3304501603129,-39.7397688129298,
176.685485069079));
#46559=CARTESIAN_POINT('Ctrl Pts',(-77.4354809475772,-39.918618205007,176.685485069079));
#46560=CARTESIAN_POINT('Ctrl Pts',(-77.5387174074033,-40.095017410943,176.685485069079));
#46561=CARTESIAN_POINT('Ctrl Pts',(-77.7452188224523,-40.4514138749057,
176.685485069079));
#46562=CARTESIAN_POINT('Ctrl Pts',(-78.0537048438588,-40.988104564515,176.685485069079));
#46563=CARTESIAN_POINT('Ctrl Pts',(-78.7646561081799,-42.2546401779696,
176.685485069079));
#46564=CARTESIAN_POINT('Ctrl Pts',(-79.358919965841,-43.3632613763041,176.685485069079));
#46565=CARTESIAN_POINT('Ctrl Pts',(-80.5274284163852,-45.6074041562991,
176.685485069079));
#46566=CARTESIAN_POINT('Ctrl Pts',(-81.2797370189181,-47.139365595286,176.685485069079));
#46567=CARTESIAN_POINT('Ctrl Pts',(-83.3745257073509,-51.6335950639466,
176.685485069079));
#46568=CARTESIAN_POINT('Ctrl Pts',(-84.6499486695732,-54.6616303374944,
176.685485069079));
#46569=CARTESIAN_POINT('Ctrl Pts',(-85.8357028732072,-57.7136681697975,
176.685485069079));
#46570=CARTESIAN_POINT('',(-86.4935648641623,-59.4333382806591,176.685485069079));
#46571=CARTESIAN_POINT('Ctrl Pts',(-85.8357032382115,-57.7136680279929,
176.685485069079));
#46572=CARTESIAN_POINT('Ctrl Pts',(-85.8575368827931,-57.7698663129345,
176.685485072469));
#46573=CARTESIAN_POINT('Ctrl Pts',(-85.8790685227464,-57.8253736599762,
176.689988619807));
#46574=CARTESIAN_POINT('Ctrl Pts',(-85.9002716509352,-57.8801146319343,
176.698219460949));
#46575=CARTESIAN_POINT('Ctrl Pts',(-85.9074955079205,-57.8987647551209,
176.701023689587));
#46576=CARTESIAN_POINT('Ctrl Pts',(-85.9146812616168,-57.9173259872642,
176.704260100816));
#46577=CARTESIAN_POINT('Ctrl Pts',(-85.9218279524688,-57.9357955500639,
176.707896698839));
#46578=CARTESIAN_POINT('Ctrl Pts',(-85.9473631106758,-58.0017873801117,
176.720890279754));
#46579=CARTESIAN_POINT('Ctrl Pts',(-85.9724206859325,-58.066662896417,176.739132966205));
#46580=CARTESIAN_POINT('Ctrl Pts',(-85.9971566701928,-58.1308157259833,
176.760337228688));
#46581=CARTESIAN_POINT('Ctrl Pts',(-85.9995997074219,-58.1371517484087,
176.762431457166));
#46582=CARTESIAN_POINT('Ctrl Pts',(-86.002039611443,-58.1434807298304,176.764554536289));
#46583=CARTESIAN_POINT('Ctrl Pts',(-86.0044765344927,-58.1498030537245,
176.766704243004));
#46584=CARTESIAN_POINT('Ctrl Pts',(-86.0044947695771,-58.1498503626085,
176.766720328897));
#46585=CARTESIAN_POINT('Ctrl Pts',(-86.004513004512,-58.1498976711649,176.766736416296));
#46586=CARTESIAN_POINT('Ctrl Pts',(-86.0045312392975,-58.1499449793939,
176.7667525052));
#46587=CARTESIAN_POINT('Ctrl Pts',(-86.0316555436731,-58.2203161281954,
176.790684803966));
#46588=CARTESIAN_POINT('Ctrl Pts',(-86.0584159099637,-58.2898750286768,
176.818336470784));
#46589=CARTESIAN_POINT('Ctrl Pts',(-86.0855089993157,-58.3604325361075,
176.841588389785));
#46590=CARTESIAN_POINT('Ctrl Pts',(-86.0855275926271,-58.3604809579648,
176.841604346997));
#46591=CARTESIAN_POINT('Ctrl Pts',(-86.0855461860946,-58.360529380291,176.841620302136));
#46592=CARTESIAN_POINT('Ctrl Pts',(-86.0855647797187,-58.3605778030869,
176.841636255199));
#46593=CARTESIAN_POINT('Ctrl Pts',(-86.0991224819847,-58.3958857048106,
176.853268569574));
#46594=CARTESIAN_POINT('Ctrl Pts',(-86.1128236371906,-58.4316010060895,
176.863656877716));
#46595=CARTESIAN_POINT('Ctrl Pts',(-86.1265739659578,-58.4674794490787,
176.87090073909));
#46596=CARTESIAN_POINT('Ctrl Pts',(-86.1403017396453,-58.5032990395742,
176.878132718138));
#46597=CARTESIAN_POINT('Ctrl Pts',(-86.1540992591418,-58.5393351357888,
176.882147372206));
#46598=CARTESIAN_POINT('Ctrl Pts',(-86.1679922740321,-58.5756563092537,
176.881927610312));
#46599=CARTESIAN_POINT('Ctrl Pts',(-86.1680170995237,-58.575721211724,176.881927217619));
#46600=CARTESIAN_POINT('Ctrl Pts',(-86.1680419253213,-58.5757861151074,
176.881926811406));
#46601=CARTESIAN_POINT('Ctrl Pts',(-86.168066751425,-58.5758510194043,176.881926391667));
#46602=CARTESIAN_POINT('Ctrl Pts',(-86.1819856190064,-58.6122399076145,
176.881691063191));
#46603=CARTESIAN_POINT('Ctrl Pts',(-86.1961417868957,-58.6492857813369,
176.877082885163));
#46604=CARTESIAN_POINT('Ctrl Pts',(-86.209949809353,-58.6854557833995,176.86935105246));
#46605=CARTESIAN_POINT('Ctrl Pts',(-86.2237241681295,-58.721537603725,176.86163806981));
#46606=CARTESIAN_POINT('Ctrl Pts',(-86.2371818936595,-58.7568245986939,
176.851054685034));
#46607=CARTESIAN_POINT('Ctrl Pts',(-86.2505145561711,-58.7918158238361,
176.8393675931));
#46608=CARTESIAN_POINT('Ctrl Pts',(-86.2505443517163,-58.7918940214677,
176.83934147504));
#46609=CARTESIAN_POINT('Ctrl Pts',(-86.2505741466266,-58.7919722175953,
176.839315351477));
#46610=CARTESIAN_POINT('Ctrl Pts',(-86.2506039409043,-58.7920504122243,
176.839289222431));
#46611=CARTESIAN_POINT('Ctrl Pts',(-86.2772947577064,-58.8621000554093,
176.81588185555));
#46612=CARTESIAN_POINT('Ctrl Pts',(-86.3035333311623,-58.9310915384274,
176.788590780995));
#46613=CARTESIAN_POINT('Ctrl Pts',(-86.3301164702189,-59.0011188486079,
176.764983643558));
#46614=CARTESIAN_POINT('Ctrl Pts',(-86.3301422175475,-59.0011866741631,
176.764960778662));
#46615=CARTESIAN_POINT('Ctrl Pts',(-86.3301679651756,-59.0012545006274,
176.76493791724));
#46616=CARTESIAN_POINT('Ctrl Pts',(-86.3301937131039,-59.0013223280029,
176.7649150593));
#46617=CARTESIAN_POINT('Ctrl Pts',(-86.3548279743324,-59.0662159871751,
176.743045786526));
#46618=CARTESIAN_POINT('Ctrl Pts',(-86.3796895393454,-59.1318204739591,
176.72409006409));
#46619=CARTESIAN_POINT('Ctrl Pts',(-86.4048426318501,-59.1983128551758,
176.710356737887));
#46620=CARTESIAN_POINT('Ctrl Pts',(-86.406872472465,-59.2036787534625,176.709248466079));
#46621=CARTESIAN_POINT('Ctrl Pts',(-86.4089042134845,-59.209050439792,176.708174234396));
#46622=CARTESIAN_POINT('Ctrl Pts',(-86.4109378896597,-59.2144280102915,
176.707135274671));
#46623=CARTESIAN_POINT('Ctrl Pts',(-86.432177732687,-59.27059169784,176.696284313379));
#46624=CARTESIAN_POINT('Ctrl Pts',(-86.4537315983723,-59.3276705378626,
176.689177561902));
#46625=CARTESIAN_POINT('Ctrl Pts',(-86.4753675306458,-59.3850540800865,
176.686583816668));
#46626=CARTESIAN_POINT('Ctrl Pts',(-86.4814286020451,-59.4011294560936,
176.685857207116));
#46627=CARTESIAN_POINT('Ctrl Pts',(-86.4874960982682,-59.4172287082636,
176.685485070601));
#46628=CARTESIAN_POINT('Ctrl Pts',(-86.4935648641623,-59.4333382806591,
176.685485069079));
#46629=CARTESIAN_POINT('',(-98.743146025648,-101.814198524563,176.685485069079));
#46630=CARTESIAN_POINT('Ctrl Pts',(-86.4935648641623,-59.433338280659,176.685485069079));
#46631=CARTESIAN_POINT('Ctrl Pts',(-87.7856096728309,-62.8630783211318,
176.685485069079));
#46632=CARTESIAN_POINT('Ctrl Pts',(-88.9767665307843,-66.3330832476407,
176.685485069079));
#46633=CARTESIAN_POINT('Ctrl Pts',(-91.2072333103094,-73.3336959729049,
176.685485069079));
#46634=CARTESIAN_POINT('Ctrl Pts',(-92.2465762119515,-76.8666920983617,
176.68548506908));
#46635=CARTESIAN_POINT('Ctrl Pts',(-94.2061160331528,-83.9673845124857,
176.685485069079));
#46636=CARTESIAN_POINT('Ctrl Pts',(-95.1241782504859,-87.5338958106165,
176.68548506908));
#46637=CARTESIAN_POINT('Ctrl Pts',(-96.449702093816,-92.8970651812464,176.68548506908));
#46638=CARTESIAN_POINT('Ctrl Pts',(-96.8822526521753,-94.687157625756,176.685485069079));
#46639=CARTESIAN_POINT('Ctrl Pts',(-97.5376559351784,-97.3706189117761,
176.685485069079));
#46640=CARTESIAN_POINT('Ctrl Pts',(-97.7569410503841,-98.264897565372,176.685485069079));
#46641=CARTESIAN_POINT('Ctrl Pts',(-98.099506581766,-99.6028376178243,176.685485069079));
#46642=CARTESIAN_POINT('Ctrl Pts',(-98.2159080866078,-100.048253277279,
176.685485069079));
#46643=CARTESIAN_POINT('Ctrl Pts',(-98.4002244375469,-100.713899477402,
176.685485069079));
#46644=CARTESIAN_POINT('Ctrl Pts',(-98.4633004780488,-100.935364010716,
176.685485069079));
#46645=CARTESIAN_POINT('Ctrl Pts',(-98.5960691137325,-101.376605722965,
176.685485069079));
#46646=CARTESIAN_POINT('Ctrl Pts',(-98.6653474496106,-101.596488546345,
176.685485069079));
#46647=CARTESIAN_POINT('Ctrl Pts',(-98.7431461177365,-101.814198491655,
176.685485069079));
#46648=CARTESIAN_POINT('',(-98.743146025648,-101.814198524563,175.285485069079));
#46649=CARTESIAN_POINT('',(-98.7431461249941,-101.814198511965,177.685485069079));
#46650=CARTESIAN_POINT('',(-86.4935648641564,-59.4333382806435,175.285485069079));
#46651=CARTESIAN_POINT('Ctrl Pts',(-98.7431461177365,-101.814198491655,
175.285485069079));
#46652=CARTESIAN_POINT('Ctrl Pts',(-98.6654638987115,-101.596814414744,
175.285485069079));
#46653=CARTESIAN_POINT('Ctrl Pts',(-98.5962640059336,-101.377220104144,
175.285485069079));
#46654=CARTESIAN_POINT('Ctrl Pts',(-98.4636402639926,-100.936526438504,
175.285485069079));
#46655=CARTESIAN_POINT('Ctrl Pts',(-98.4006272590078,-100.715320031166,
175.285485069079));
#46656=CARTESIAN_POINT('Ctrl Pts',(-98.2164901868202,-100.050423526257,
175.285485069079));
#46657=CARTESIAN_POINT('Ctrl Pts',(-98.100194770959,-99.6054752430948,175.285485069079));
#46658=CARTESIAN_POINT('Ctrl Pts',(-97.7579408317027,-98.2689022351253,
175.285485069079));
#46659=CARTESIAN_POINT('Ctrl Pts',(-97.5388526271146,-97.3754873342376,
175.285485069079));
#46660=CARTESIAN_POINT('Ctrl Pts',(-96.8840551083993,-94.6945997888377,
175.285485069079));
#46661=CARTESIAN_POINT('Ctrl Pts',(-96.451924672254,-92.9061946080142,175.285485069079));
#46662=CARTESIAN_POINT('Ctrl Pts',(-95.1277832686895,-87.5482098153712,
175.285485069079));
#46663=CARTESIAN_POINT('Ctrl Pts',(-94.2107624601005,-83.9851469345354,
175.285485069079));
#46664=CARTESIAN_POINT('Ctrl Pts',(-92.2535686906978,-76.8911105188406,
175.285485069079));
#46665=CARTESIAN_POINT('Ctrl Pts',(-91.2147869939348,-73.3584403924464,
175.285485069079));
#46666=CARTESIAN_POINT('Ctrl Pts',(-88.9819313083959,-66.3482632730971,
175.285485069079));
#46667=CARTESIAN_POINT('Ctrl Pts',(-87.7888733385873,-62.8717417398051,
175.285485069079));
#46668=CARTESIAN_POINT('Ctrl Pts',(-86.4935648641568,-59.4333382806445,
175.285485069079));
#46669=CARTESIAN_POINT('',(-85.8357031165468,-57.7136680752698,175.285485069079));
#46670=CARTESIAN_POINT('Ctrl Pts',(-86.4935648641564,-59.4333382806436,
175.285485069079));
#46671=CARTESIAN_POINT('Ctrl Pts',(-86.4719023592219,-59.3758350423251,
175.285485063649));
#46672=CARTESIAN_POINT('Ctrl Pts',(-86.4502563673306,-59.3184641207399,
175.280747741342));
#46673=CARTESIAN_POINT('Ctrl Pts',(-86.4288596853718,-59.261837956496,175.272056283427));
#46674=CARTESIAN_POINT('Ctrl Pts',(-86.4228645085134,-59.2459717642467,
175.269621007366));
#46675=CARTESIAN_POINT('Ctrl Pts',(-86.4168888826336,-59.2301639886453,
175.266874982765));
#46676=CARTESIAN_POINT('Ctrl Pts',(-86.4109378971216,-59.2144280300232,
175.263834747309));
#46677=CARTESIAN_POINT('Ctrl Pts',(-86.3857421845665,-59.1478039911273,
175.250962778712));
#46678=CARTESIAN_POINT('Ctrl Pts',(-86.3608432187804,-59.0820822507344,
175.232681904101));
#46679=CARTESIAN_POINT('Ctrl Pts',(-86.3361765285873,-59.0170849735409,
175.211303790484));
#46680=CARTESIAN_POINT('Ctrl Pts',(-86.3341807485036,-59.0118260486385,
175.209574088889));
#46681=CARTESIAN_POINT('Ctrl Pts',(-86.3321864908343,-59.0065718720304,
175.207824086198));
#46682=CARTESIAN_POINT('Ctrl Pts',(-86.3301937223889,-59.0013223524624,
175.206054996239));
#46683=CARTESIAN_POINT('Ctrl Pts',(-86.3301651272193,-59.0012470246425,
175.206029610737));
#46684=CARTESIAN_POINT('Ctrl Pts',(-86.33013653242,-59.0011716979463,175.206004220941));
#46685=CARTESIAN_POINT('Ctrl Pts',(-86.3301079379899,-59.0010963723711,
175.20597882686));
#46686=CARTESIAN_POINT('Ctrl Pts',(-86.3035277119236,-58.9310767632205,
175.182373515954));
#46687=CARTESIAN_POINT('Ctrl Pts',(-86.2772919052129,-58.8620925690934,
175.155085719146));
#46688=CARTESIAN_POINT('Ctrl Pts',(-86.2506039439847,-58.7920504203087,
175.131680888139));
#46689=CARTESIAN_POINT('Ctrl Pts',(-86.2505698616544,-58.7919609717507,
175.131650998588));
#46690=CARTESIAN_POINT('Ctrl Pts',(-86.2505357784962,-58.7918715212319,
175.131621116213));
#46691=CARTESIAN_POINT('Ctrl Pts',(-86.2505016945069,-58.7917820687439,
175.131591241042));
#46692=CARTESIAN_POINT('Ctrl Pts',(-86.2371732362759,-58.7568018984936,
175.119908630803));
#46693=CARTESIAN_POINT('Ctrl Pts',(-86.2237197381054,-58.7215259993151,
175.109329580509));
#46694=CARTESIAN_POINT('Ctrl Pts',(-86.2099498106586,-58.6854557868193,
175.101619067419));
#46695=CARTESIAN_POINT('Ctrl Pts',(-86.1961417905151,-58.6492857908156,
175.093887224206));
#46696=CARTESIAN_POINT('Ctrl Pts',(-86.1819856251605,-58.6122399237039,
175.089279016292));
#46697=CARTESIAN_POINT('Ctrl Pts',(-86.1680667516765,-58.5758510200618,
175.089043628923));
#46698=CARTESIAN_POINT('Ctrl Pts',(-86.1680359710866,-58.5757705486126,
175.089043108381));
#46699=CARTESIAN_POINT('Ctrl Pts',(-86.1680051909672,-58.5756900785675,
175.08904260863));
#46700=CARTESIAN_POINT('Ctrl Pts',(-86.1679744113182,-58.5756096099258,
175.08904212966));
#46701=CARTESIAN_POINT('Ctrl Pts',(-86.1540868127237,-58.5393026268904,
175.088826021142));
#46702=CARTESIAN_POINT('Ctrl Pts',(-86.1402962101565,-58.5032846115629,
175.092840073551));
#46703=CARTESIAN_POINT('Ctrl Pts',(-86.1265739460565,-58.4674793971515,
175.100069105802));
#46704=CARTESIAN_POINT('Ctrl Pts',(-86.1128259344222,-58.4316070002417,
175.107311702123));
#46705=CARTESIAN_POINT('Ctrl Pts',(-86.0991257058918,-58.3958941006902,
175.117698434768));
#46706=CARTESIAN_POINT('Ctrl Pts',(-86.0855647542472,-58.3605777367531,
175.129333653249));
#46707=CARTESIAN_POINT('Ctrl Pts',(-86.0855374412273,-58.3605066063059,
175.129357087663));
#46708=CARTESIAN_POINT('Ctrl Pts',(-86.0855101285278,-58.3604354768277,
175.129380526571));
#46709=CARTESIAN_POINT('Ctrl Pts',(-86.0854828161481,-58.3603643483165,
175.129403969966));
#46710=CARTESIAN_POINT('Ctrl Pts',(-86.0584038496732,-58.2898437056168,
175.152647015424));
#46711=CARTESIAN_POINT('Ctrl Pts',(-86.0316436675509,-58.2202853167348,
175.180295334629));
#46712=CARTESIAN_POINT('Ctrl Pts',(-86.004531204833,-58.1499448899798,175.204217332711));
#46713=CARTESIAN_POINT('Ctrl Pts',(-86.0044869333326,-58.1498300322382,
175.204256394554));
#46714=CARTESIAN_POINT('Ctrl Pts',(-86.0044426609819,-58.149715172646,175.204295447499));
#46715=CARTESIAN_POINT('Ctrl Pts',(-86.0043983877799,-58.1496003112007,
175.204334491534));
#46716=CARTESIAN_POINT('Ctrl Pts',(-85.9772659820254,-58.0792085797364,
175.228262252673));
#46717=CARTESIAN_POINT('Ctrl Pts',(-85.9498440260562,-58.0081989380341,
175.248817356079));
#46718=CARTESIAN_POINT('Ctrl Pts',(-85.9218279496276,-57.9357955427215,
175.263073396718));
#46719=CARTESIAN_POINT('Ctrl Pts',(-85.8983583315347,-57.8751417948294,
175.275015962271));
#46720=CARTESIAN_POINT('Ctrl Pts',(-85.8744536632948,-57.8134637449331,
175.282654209087));
#46721=CARTESIAN_POINT('Ctrl Pts',(-85.8500832601142,-57.7506936916401,
175.284838580227));
#46722=CARTESIAN_POINT('Ctrl Pts',(-85.8453078965934,-57.7383939434387,
175.28526660623));
#46723=CARTESIAN_POINT('Ctrl Pts',(-85.8405146387439,-57.7260522388413,
175.285485068332));
#46724=CARTESIAN_POINT('Ctrl Pts',(-85.8357032382103,-57.7136680279897,
175.285485069079));
#46725=CARTESIAN_POINT('Origin',(71.2336965524492,-1004.00503493024,175.285485069079));
#46726=CARTESIAN_POINT('Ctrl Pts',(-99.7596659041602,-101.966952700553,
174.385485069079));
#46727=CARTESIAN_POINT('Ctrl Pts',(-99.7596659041602,-101.966952700553,
173.385485069079));
#46728=CARTESIAN_POINT('Ctrl Pts',(-98.8225296350236,-102.315916327695,
173.385485069079));
#46729=CARTESIAN_POINT('Ctrl Pts',(-99.7292244094599,-101.885202550819,
174.385485069079));
#46730=CARTESIAN_POINT('Ctrl Pts',(-99.7292244094596,-101.88520255082,173.385485069079));
#46731=CARTESIAN_POINT('Ctrl Pts',(-98.792088140323,-102.234166177962,173.385485069079));
#46732=CARTESIAN_POINT('Ctrl Pts',(-99.6987829147594,-101.803452401085,
174.385485069079));
#46733=CARTESIAN_POINT('Ctrl Pts',(-99.6987829147593,-101.803452401085,
173.385485069079));
#46734=CARTESIAN_POINT('Ctrl Pts',(-98.7616466456226,-102.152416028228,
173.385485069079));
#46735=CARTESIAN_POINT('Ctrl Pts',(-99.6531206727089,-101.680827176485,
174.385485069079));
#46736=CARTESIAN_POINT('Ctrl Pts',(-99.6531206727089,-101.680827176486,
173.385485069079));
#46737=CARTESIAN_POINT('Ctrl Pts',(-98.7159844035723,-102.029790803628,
173.385485069079));
#46738=CARTESIAN_POINT('Ctrl Pts',(-99.6378999253588,-101.639952101619,
174.385485069079));
#46739=CARTESIAN_POINT('Ctrl Pts',(-99.6378999253586,-101.639952101619,
173.385485069079));
#46740=CARTESIAN_POINT('Ctrl Pts',(-98.700763656222,-101.988915728762,173.385485069079));
#46741=CARTESIAN_POINT('Ctrl Pts',(-99.6150688043334,-101.578639489318,
174.385485069079));
#46742=CARTESIAN_POINT('Ctrl Pts',(-99.6150688043334,-101.578639489318,
173.385485069079));
#46743=CARTESIAN_POINT('Ctrl Pts',(-98.6779325351968,-101.927603116461,
173.385485069079));
#46744=CARTESIAN_POINT('Ctrl Pts',(-99.609407429959,-101.563252285373,174.385485069079));
#46745=CARTESIAN_POINT('Ctrl Pts',(-99.6094074304456,-101.563252285196,
173.385485069079));
#46746=CARTESIAN_POINT('Ctrl Pts',(-98.6703932517879,-101.907141939063,
173.385485069079));
#46747=CARTESIAN_POINT('Ctrl Pts',(-99.5964225120462,-101.527488620696,
174.385485069079));
#46748=CARTESIAN_POINT('Ctrl Pts',(-99.5964225115595,-101.527488620872,
173.385485069079));
#46749=CARTESIAN_POINT('Ctrl Pts',(-98.6555115664908,-101.866154114362,
173.385485069079));
#46750=CARTESIAN_POINT('Ctrl Pts',(-99.5899497481367,-101.509428783166,
174.385485069079));
#46751=CARTESIAN_POINT('Ctrl Pts',(-99.5899497485787,-101.509428783009,
173.385485069079));
#46752=CARTESIAN_POINT('Ctrl Pts',(-98.648156867377,-101.845631556315,173.385485069079));
#46753=CARTESIAN_POINT('Ctrl Pts',(-99.5318916024491,-101.345511288159,
174.385485069079));
#46754=CARTESIAN_POINT('Ctrl Pts',(-99.531891598913,-101.345511289411,173.385485069079));
#46755=CARTESIAN_POINT('Ctrl Pts',(-98.5826553075554,-101.660698841608,
173.385485069079));
#46756=CARTESIAN_POINT('Ctrl Pts',(-99.4817965056164,-101.190760589972,
174.385485069079));
#46757=CARTESIAN_POINT('Ctrl Pts',(-99.4817965071391,-101.190760589501,
173.385485069079));
#46758=CARTESIAN_POINT('Ctrl Pts',(-98.5290815182737,-101.494767980892,
173.385485069079));
#46759=CARTESIAN_POINT('Ctrl Pts',(-99.3356133931763,-100.717504207786,
174.385485069079));
#46760=CARTESIAN_POINT('Ctrl Pts',(-99.3356133901308,-100.717504208727,
173.385485069079));
#46761=CARTESIAN_POINT('Ctrl Pts',(-98.3746712206805,-100.994876750151,
173.385485069079));
#46762=CARTESIAN_POINT('Ctrl Pts',(-99.2432304743068,-100.389603655864,
174.385485069079));
#46763=CARTESIAN_POINT('Ctrl Pts',(-99.2432304751161,-100.389603655646,
173.385485069075));
#46764=CARTESIAN_POINT('Ctrl Pts',(-98.2801283097388,-100.658823541833,
173.385485069079));
#46765=CARTESIAN_POINT('Ctrl Pts',(-98.9732428581022,-99.3981138801062,
174.385485069079));
#46766=CARTESIAN_POINT('Ctrl Pts',(-98.9732428564835,-99.3981138805421,
173.385485069089));
#46767=CARTESIAN_POINT('Ctrl Pts',(-98.0048456627939,-99.6478885553121,
173.385485069079));
#46768=CARTESIAN_POINT('Ctrl Pts',(-98.8024390932428,-98.724463698621,174.385485069079));
#46769=CARTESIAN_POINT('Ctrl Pts',(-98.802439093562,-98.7244636985413,173.385485069079));
#46770=CARTESIAN_POINT('Ctrl Pts',(-97.8330538201541,-98.9700312938576,
173.385485069079));
#46771=CARTESIAN_POINT('Ctrl Pts',(-98.2964066418388,-96.6983592678497,
174.385485069079));
#46772=CARTESIAN_POINT('Ctrl Pts',(-98.2964066412002,-96.6983592680092,
173.385485069079));
#46773=CARTESIAN_POINT('Ctrl Pts',(-97.324582902825,-96.9341634882031,173.385485069079));
#46774=CARTESIAN_POINT('Ctrl Pts',(-97.9682125919038,-95.3374251041846,
174.385485069079));
#46775=CARTESIAN_POINT('Ctrl Pts',(-97.9682125920466,-95.3374251041595,
173.385485069079));
#46776=CARTESIAN_POINT('Ctrl Pts',(-96.9964329902176,-95.5733167033208,
173.385485069079));
#46777=CARTESIAN_POINT('Ctrl Pts',(-96.9745721058683,-91.2558483999456,
174.385485069079));
#46778=CARTESIAN_POINT('Ctrl Pts',(-96.9745721055826,-91.2558483999958,
173.385485069079));
#46779=CARTESIAN_POINT('Ctrl Pts',(-96.0032637830826,-91.4936758730623,
173.385485069079));
#46780=CARTESIAN_POINT('Ctrl Pts',(-96.3022773498184,-88.5330308242917,
174.385485069079));
#46781=CARTESIAN_POINT('Ctrl Pts',(-96.3022773498185,-88.5330308242917,
173.385485069079));
#46782=CARTESIAN_POINT('Ctrl Pts',(-95.3324240441395,-88.7768173262609,
173.385485069079));
#46783=CARTESIAN_POINT('Ctrl Pts',(-94.1962497890728,-80.3918582514504,
174.385485069079));
#46784=CARTESIAN_POINT('Ctrl Pts',(-94.1962497890724,-80.3918582514505,
173.385485069079));
#46785=CARTESIAN_POINT('Ctrl Pts',(-93.2315633992081,-80.6556182591984,
173.385485069079));
#46786=CARTESIAN_POINT('Ctrl Pts',(-92.6770445486041,-74.9910315479212,
174.385485069079));
#46787=CARTESIAN_POINT('Ctrl Pts',(-92.6770445486971,-74.9910315478917,
173.385485069079));
#46788=CARTESIAN_POINT('Ctrl Pts',(-91.7172498887648,-75.2726409100276,
173.385485069079));
#46789=CARTESIAN_POINT('Ctrl Pts',(-90.1390857940941,-67.0122253917376,
174.385485069079));
#46790=CARTESIAN_POINT('Ctrl Pts',(-90.1390857940475,-67.0122253917524,
173.385485069079));
#46791=CARTESIAN_POINT('Ctrl Pts',(-89.1895555183278,-67.32610380923,173.385485069079));
#46792=CARTESIAN_POINT('Ctrl Pts',(-89.2499340323246,-64.3720031405279,
174.385485069118));
#46793=CARTESIAN_POINT('Ctrl Pts',(-89.2499340324016,-64.3720031404906,
173.385485069156));
#46794=CARTESIAN_POINT('Ctrl Pts',(-88.3043449817598,-64.6976651653227,
173.385485069079));
#46795=CARTESIAN_POINT('Ctrl Pts',(-87.3656218452655,-59.1388679004802,
174.385485069041));
#46796=CARTESIAN_POINT('Ctrl Pts',(-87.3656218451886,-59.1388679005176,
173.385485069003));
#46797=CARTESIAN_POINT('Ctrl Pts',(-86.4294800240879,-59.490766888681,173.385485069079));
#46798=CARTESIAN_POINT('Ctrl Pts',(-86.3706260282542,-56.5458859385069,
174.385485069079));
#46799=CARTESIAN_POINT('Ctrl Pts',(-86.37062602833,-56.5458859384659,173.385485069079));
#46800=CARTESIAN_POINT('Ctrl Pts',(-85.4399803831464,-56.912233189929,173.385485069079));
#46801=CARTESIAN_POINT('Ctrl Pts',(-84.2471258837627,-51.4188822072724,
174.385485069079));
#46802=CARTESIAN_POINT('Ctrl Pts',(-84.2471258836868,-51.4188822073134,
173.385485069079));
#46803=CARTESIAN_POINT('Ctrl Pts',(-83.3299902505975,-51.8178481908489,
173.385485069079));
#46804=CARTESIAN_POINT('Ctrl Pts',(-83.1189413138823,-48.8847318393425,
174.385485069041));
#46805=CARTESIAN_POINT('Ctrl Pts',(-83.1189413140826,-48.8847318392535,
173.385485069003));
#46806=CARTESIAN_POINT('Ctrl Pts',(-82.209794638272,-49.3018557835574,173.385485069079));
#46807=CARTESIAN_POINT('Ctrl Pts',(-81.2948030758993,-45.1409331067813,
174.385485069099));
#46808=CARTESIAN_POINT('Ctrl Pts',(-81.2948030757991,-45.1409331068258,
173.385485069118));
#46809=CARTESIAN_POINT('Ctrl Pts',(-80.4009251217981,-45.5893940515925,
173.385485069079));
#46810=CARTESIAN_POINT('Ctrl Pts',(-80.6646391351484,-43.9026279540674,
174.385485069099));
#46811=CARTESIAN_POINT('Ctrl Pts',(-80.6646391352473,-43.9026279540145,
173.385485069118));
#46812=CARTESIAN_POINT('Ctrl Pts',(-79.7764072455219,-44.3622244628955,
173.385485069079));
#46813=CARTESIAN_POINT('Ctrl Pts',(-79.6803177277805,-42.0620394131515,
174.38548506907));
#46814=CARTESIAN_POINT('Ctrl Pts',(-79.680317727731,-42.062039413178,173.38548506906));
#46815=CARTESIAN_POINT('Ctrl Pts',(-78.8017030821551,-42.539619264928,173.385485069079));
#46816=CARTESIAN_POINT('Ctrl Pts',(-79.345681744444,-41.4513279672577,174.385485069079));
#46817=CARTESIAN_POINT('Ctrl Pts',(-79.3456817444886,-41.4513279672327,
173.385485069079));
#46818=CARTESIAN_POINT('Ctrl Pts',(-78.4704654251786,-41.9351162622582,
173.385485069079));
#46819=CARTESIAN_POINT('Ctrl Pts',(-78.6621302404233,-40.2360419657214,
174.385485069079));
#46820=CARTESIAN_POINT('Ctrl Pts',(-78.6621302403787,-40.2360419657465,
173.385485069079));
#46821=CARTESIAN_POINT('Ctrl Pts',(-77.7941667579945,-40.7327250772214,
173.385485069079));
#46822=CARTESIAN_POINT('Ctrl Pts',(-78.3097223640001,-39.6300292660079,
174.385485068993));
#46823=CARTESIAN_POINT('Ctrl Pts',(-78.3097223639766,-39.6300292660224,
173.385485068964));
#46824=CARTESIAN_POINT('Ctrl Pts',(-77.4471311115058,-40.1359310914719,
173.38548506908));
#46825=CARTESIAN_POINT('Ctrl Pts',(-77.959578073788,-39.0337936757116,174.385485069079));
#46826=CARTESIAN_POINT('Ctrl Pts',(-77.959578073788,-39.0337936757116,173.38548506908));
#46827=CARTESIAN_POINT('Ctrl Pts',(-77.0972759082386,-39.5401877666021,
173.38548506908));
#46828=CARTESIAN_POINT('Ctrl Pts',(-99.6210548294771,-101.594714864612,
174.385485069079));
#46829=CARTESIAN_POINT('Ctrl Pts',(-99.6210548294771,-101.594714864612,
174.34834857337));
#46830=CARTESIAN_POINT('Ctrl Pts',(-99.618332160695,-101.59351716655,174.311500923249));
#46831=CARTESIAN_POINT('Ctrl Pts',(-99.6131135575374,-101.591164496407,
174.275214504829));
#46832=CARTESIAN_POINT('Ctrl Pts',(-99.6078545210065,-101.58879359794,174.238646941769));
#46833=CARTESIAN_POINT('Ctrl Pts',(-99.6000608571668,-101.585250119418,
174.202649876939));
#46834=CARTESIAN_POINT('Ctrl Pts',(-99.5899798151376,-101.580618616698,
174.167471979048));
#46835=CARTESIAN_POINT('Ctrl Pts',(-99.5798490586212,-101.575964273801,
174.132120601952));
#46836=CARTESIAN_POINT('Ctrl Pts',(-99.5674084825397,-101.570211617946,
174.09759691258));
#46837=CARTESIAN_POINT('Ctrl Pts',(-99.5529219608852,-101.563481236162,
174.06411575878));
#46838=CARTESIAN_POINT('Ctrl Pts',(-99.5383060730445,-101.556690751351,
174.030335614699));
#46839=CARTESIAN_POINT('Ctrl Pts',(-99.5216077299695,-101.54890552263,173.997617041083));
#46840=CARTESIAN_POINT('Ctrl Pts',(-99.5031082972169,-101.540277215404,
173.966136832419));
#46841=CARTESIAN_POINT('Ctrl Pts',(-99.4988154010547,-101.538274968769,
173.958831675078));
#46842=CARTESIAN_POINT('Ctrl Pts',(-99.4944255530036,-101.536227420283,
173.951593007567));
#46843=CARTESIAN_POINT('Ctrl Pts',(-99.4899423300563,-101.534136629017,
173.944422680324));
#46844=CARTESIAN_POINT('Ctrl Pts',(-99.4689599025389,-101.524351285588,
173.910864038825));
#46845=CARTESIAN_POINT('Ctrl Pts',(-99.4461069453536,-101.513608878056,
173.8789021653));
#46846=CARTESIAN_POINT('Ctrl Pts',(-99.4216728421184,-101.502084985449,
173.848538290026));
#46847=CARTESIAN_POINT('Ctrl Pts',(-99.3964631122686,-101.490195282903,
173.817210555774));
#46848=CARTESIAN_POINT('Ctrl Pts',(-99.3695702812386,-101.47747374905,173.787583070185));
#46849=CARTESIAN_POINT('Ctrl Pts',(-99.3412946667283,-101.464066201814,
173.759628630428));
#46850=CARTESIAN_POINT('Ctrl Pts',(-99.3115503206794,-101.449962220996,
173.730222142041));
#46851=CARTESIAN_POINT('Ctrl Pts',(-99.2802758323409,-101.43509917539,173.702666199029));
#46852=CARTESIAN_POINT('Ctrl Pts',(-99.2478012559472,-101.419594345565,
173.676910847654));
#46853=CARTESIAN_POINT('Ctrl Pts',(-99.2256833056099,-101.409034236884,
173.659369261408));
#46854=CARTESIAN_POINT('Ctrl Pts',(-99.2030082431429,-101.398175294163,
173.642662567942));
#46855=CARTESIAN_POINT('Ctrl Pts',(-99.1798756003963,-101.387041827359,
173.626773374128));
#46856=CARTESIAN_POINT('Ctrl Pts',(-99.1494216646984,-101.372384709024,
173.605855379933));
#46857=CARTESIAN_POINT('Ctrl Pts',(-99.1183874733352,-101.357358017017,
173.586499314387));
#46858=CARTESIAN_POINT('Ctrl Pts',(-99.0868248128164,-101.342034097248,
173.568583317232));
#46859=CARTESIAN_POINT('Ctrl Pts',(-99.0545962472609,-101.326386875349,
173.550289330626));
#46860=CARTESIAN_POINT('Ctrl Pts',(-99.0218164572501,-101.310429158371,
173.533496191528));
#46861=CARTESIAN_POINT('Ctrl Pts',(-98.9885233176074,-101.294191619556,
173.518100410703));
#46862=CARTESIAN_POINT('Ctrl Pts',(-98.9544252291626,-101.277561495735,
173.502332396574));
#46863=CARTESIAN_POINT('Ctrl Pts',(-98.9197884262851,-101.260637206904,
173.48802953069));
#46864=CARTESIAN_POINT('Ctrl Pts',(-98.8846392312882,-101.243413123976,
173.475117316581));
#46865=CARTESIAN_POINT('Ctrl Pts',(-98.854532300697,-101.228659890816,173.464057400871));
#46866=CARTESIAN_POINT('Ctrl Pts',(-98.8240491005275,-101.213685789607,
173.454018251898));
#46867=CARTESIAN_POINT('Ctrl Pts',(-98.7932002122912,-101.198471277188,
173.444978177844));
#46868=CARTESIAN_POINT('Ctrl Pts',(-98.7399202961621,-101.172193897612,
173.429364831143));
#46869=CARTESIAN_POINT('Ctrl Pts',(-98.6859976032515,-101.145478653186,
173.4168867974));
#46870=CARTESIAN_POINT('Ctrl Pts',(-98.6317552693108,-101.118520958096,
173.407465229906));
#46871=CARTESIAN_POINT('Ctrl Pts',(-98.5731330334416,-101.089386511894,
173.397282899762));
#46872=CARTESIAN_POINT('Ctrl Pts',(-98.5141370068313,-101.059967683379,
173.390669338173));
#46873=CARTESIAN_POINT('Ctrl Pts',(-98.4551572085075,-101.030463121763,
173.387558540043));
#46874=CARTESIAN_POINT('Ctrl Pts',(-98.4289295637809,-101.017342779173,
173.386175203537));
#46875=CARTESIAN_POINT('Ctrl Pts',(-98.4027049473097,-101.004204997354,
173.385485069079));
#46876=CARTESIAN_POINT('Ctrl Pts',(-98.3765170572744,-100.991065637145,
173.385485069079));
#46877=CARTESIAN_POINT('Ctrl Pts',(-77.959578073788,-39.0337936757116,177.585485069079));
#46878=CARTESIAN_POINT('Ctrl Pts',(-77.959578073788,-39.0337936757116,178.585485069079));
#46879=CARTESIAN_POINT('Ctrl Pts',(-77.0972759082386,-39.5401877666022,
178.585485069079));
#46880=CARTESIAN_POINT('Ctrl Pts',(-78.3097223640055,-39.6300292660171,
177.585485069079));
#46881=CARTESIAN_POINT('Ctrl Pts',(-78.3097223640027,-39.6300292660199,
178.585485069079));
#46882=CARTESIAN_POINT('Ctrl Pts',(-77.4471311115041,-40.1359310914853,
178.585485069079));
#46883=CARTESIAN_POINT('Ctrl Pts',(-78.6621302404163,-40.2360419657091,
177.585485069108));
#46884=CARTESIAN_POINT('Ctrl Pts',(-78.6621302403905,-40.2360419657227,
178.585485069118));
#46885=CARTESIAN_POINT('Ctrl Pts',(-77.7941667579824,-40.7327250772121,
178.585485069079));
#46886=CARTESIAN_POINT('Ctrl Pts',(-79.345681744451,-41.4513279672701,177.585485069051));
#46887=CARTESIAN_POINT('Ctrl Pts',(-79.3456817444768,-41.4513279672565,
178.585485069041));
#46888=CARTESIAN_POINT('Ctrl Pts',(-78.4704654251907,-41.9351162622676,
178.585485069079));
#46889=CARTESIAN_POINT('Ctrl Pts',(-79.6803177277905,-42.0620394131701,
177.58548506907));
#46890=CARTESIAN_POINT('Ctrl Pts',(-79.6803177277355,-42.0620394131988,
178.58548506906));
#46891=CARTESIAN_POINT('Ctrl Pts',(-78.8017030821739,-42.5396192649393,
178.585485069079));
#46892=CARTESIAN_POINT('Ctrl Pts',(-80.6646391351287,-43.9026279540306,
177.585485069099));
#46893=CARTESIAN_POINT('Ctrl Pts',(-80.6646391352386,-43.9026279539731,
178.585485069118));
#46894=CARTESIAN_POINT('Ctrl Pts',(-79.7764072454845,-44.3622244628733,
178.585485069079));
#46895=CARTESIAN_POINT('Ctrl Pts',(-81.2948030758967,-45.1409331067761,
177.585485069079));
#46896=CARTESIAN_POINT('Ctrl Pts',(-81.2948030758329,-45.1409331068024,
178.585485069079));
#46897=CARTESIAN_POINT('Ctrl Pts',(-80.4009251217938,-45.5893940515883,
178.585485069079));
#46898=CARTESIAN_POINT('Ctrl Pts',(-83.1189413138873,-48.8847318393527,
177.585485069079));
#46899=CARTESIAN_POINT('Ctrl Pts',(-83.1189413140149,-48.8847318393001,
178.585485069079));
#46900=CARTESIAN_POINT('Ctrl Pts',(-82.2097946382807,-49.3018557835656,
178.585485069079));
#46901=CARTESIAN_POINT('Ctrl Pts',(-84.2471258837835,-51.4188822073225,
177.585485069079));
#46902=CARTESIAN_POINT('Ctrl Pts',(-84.2471258836941,-51.41888220735,178.585485069079));
#46903=CARTESIAN_POINT('Ctrl Pts',(-83.3299902506047,-51.8178481909141,
178.585485069079));
#46904=CARTESIAN_POINT('Ctrl Pts',(-86.3706260282335,-56.5458859384568,
177.585485069079));
#46905=CARTESIAN_POINT('Ctrl Pts',(-86.3706260283228,-56.5458859384294,
178.585485069079));
#46906=CARTESIAN_POINT('Ctrl Pts',(-85.4399803831393,-56.9122331898639,
178.585485069079));
#46907=CARTESIAN_POINT('Ctrl Pts',(-87.3656218452865,-59.1388679005385,
177.585485069041));
#46908=CARTESIAN_POINT('Ctrl Pts',(-87.3656218451422,-59.1388679005916,
178.585485069003));
#46909=CARTESIAN_POINT('Ctrl Pts',(-86.4294800241184,-59.490766888736,178.585485069079));
#46910=CARTESIAN_POINT('Ctrl Pts',(-89.2499340323036,-64.3720031404696,
177.585485069118));
#46911=CARTESIAN_POINT('Ctrl Pts',(-89.2499340324479,-64.3720031404165,
178.585485069156));
#46912=CARTESIAN_POINT('Ctrl Pts',(-88.3043449817293,-64.6976651652677,
178.585485069079));
#46913=CARTESIAN_POINT('Ctrl Pts',(-90.1390857941228,-67.0122253918278,
177.585485069079));
#46914=CARTESIAN_POINT('Ctrl Pts',(-90.1390857940778,-67.0122253918421,
178.585485069079));
#46915=CARTESIAN_POINT('Ctrl Pts',(-89.1895555183389,-67.3261038093198,
178.585485069079));
#46916=CARTESIAN_POINT('Ctrl Pts',(-92.6770445485467,-74.9910315477408,
177.585485069079));
#46917=CARTESIAN_POINT('Ctrl Pts',(-92.6770445486365,-74.9910315477122,
178.585485069079));
#46918=CARTESIAN_POINT('Ctrl Pts',(-91.7172498887427,-75.272640909848,178.585485069079));
#46919=CARTESIAN_POINT('Ctrl Pts',(-94.1962497890392,-80.3918582513208,
177.585485069079));
#46920=CARTESIAN_POINT('Ctrl Pts',(-94.1962497890132,-80.3918582513275,
178.585485069002));
#46921=CARTESIAN_POINT('Ctrl Pts',(-93.2315633991488,-80.6556182590752,
178.585485069079));
#46922=CARTESIAN_POINT('Ctrl Pts',(-96.3022773498351,-88.5330308243565,
177.585485069079));
#46923=CARTESIAN_POINT('Ctrl Pts',(-96.3022773498481,-88.5330308243531,
178.585485069118));
#46924=CARTESIAN_POINT('Ctrl Pts',(-95.3324240441691,-88.7768173263224,
178.585485069079));
#46925=CARTESIAN_POINT('Ctrl Pts',(-96.974572105871,-91.2558483999567,177.585485069079));
#46926=CARTESIAN_POINT('Ctrl Pts',(-96.9745721056358,-91.2558483999945,
178.585485069079));
#46927=CARTESIAN_POINT('Ctrl Pts',(-96.0032637831359,-91.4936758730611,
178.585485069079));
#46928=CARTESIAN_POINT('Ctrl Pts',(-97.9682125919025,-95.3374251041791,
177.585485069079));
#46929=CARTESIAN_POINT('Ctrl Pts',(-97.96821259202,-95.3374251041602,178.585485069079));
#46930=CARTESIAN_POINT('Ctrl Pts',(-96.996432990191,-95.5733167033214,178.585485069079));
#46931=CARTESIAN_POINT('Ctrl Pts',(-98.2964066418423,-96.6983592678637,
177.585485069079));
#46932=CARTESIAN_POINT('Ctrl Pts',(-98.2964066411991,-96.6983592680243,
178.585485069079));
#46933=CARTESIAN_POINT('Ctrl Pts',(-97.3245829028239,-96.9341634882086,
178.585485069079));
#46934=CARTESIAN_POINT('Ctrl Pts',(-98.802439093241,-98.724463698614,177.585485069079));
#46935=CARTESIAN_POINT('Ctrl Pts',(-98.8024390935625,-98.7244636985337,
178.585485069079));
#46936=CARTESIAN_POINT('Ctrl Pts',(-97.8330538201546,-98.9700312938548,
178.585485069079));
#46937=CARTESIAN_POINT('Ctrl Pts',(-98.9732428581051,-99.3981138801168,
177.585485069079));
#46938=CARTESIAN_POINT('Ctrl Pts',(-98.9732428564852,-99.3981138805579,
178.585485069079));
#46939=CARTESIAN_POINT('Ctrl Pts',(-98.0048456627956,-99.6478885553231,
178.585485069079));
#46940=CARTESIAN_POINT('Ctrl Pts',(-99.2432304743053,-100.389603655859,
177.585485069079));
#46941=CARTESIAN_POINT('Ctrl Pts',(-99.2432304751152,-100.389603655638,
178.585485069079));
#46942=CARTESIAN_POINT('Ctrl Pts',(-98.2801283097379,-100.658823541827,
178.585485069079));
#46943=CARTESIAN_POINT('Ctrl Pts',(-99.3356133931767,-100.717504207787,
177.585485069079));
#46944=CARTESIAN_POINT('Ctrl Pts',(-99.3356133901333,-100.717504208727,
178.585485069079));
#46945=CARTESIAN_POINT('Ctrl Pts',(-98.3746712206855,-100.994876750151,
178.585485069079));
#46946=CARTESIAN_POINT('Ctrl Pts',(-99.4817965056161,-101.190760589971,
177.585485069079));
#46947=CARTESIAN_POINT('Ctrl Pts',(-99.4817965071378,-101.190760589501,
178.585485069079));
#46948=CARTESIAN_POINT('Ctrl Pts',(-98.5290815182711,-101.494767980891,
178.585485069079));
#46949=CARTESIAN_POINT('Ctrl Pts',(-99.5318916024483,-101.345511288157,
177.585485069079));
#46950=CARTESIAN_POINT('Ctrl Pts',(-99.5318915989119,-101.345511289408,
178.585485069079));
#46951=CARTESIAN_POINT('Ctrl Pts',(-98.5826553075542,-101.660698841605,
178.585485069079));
#46952=CARTESIAN_POINT('Ctrl Pts',(-99.5899497481368,-101.509428783166,
177.585485069079));
#46953=CARTESIAN_POINT('Ctrl Pts',(-99.5899497485788,-101.50942878301,178.585485069079));
#46954=CARTESIAN_POINT('Ctrl Pts',(-98.6481568673771,-101.845631556315,
178.585485069079));
#46955=CARTESIAN_POINT('Ctrl Pts',(-99.5964225120462,-101.527488620696,
177.585485069079));
#46956=CARTESIAN_POINT('Ctrl Pts',(-99.5964225115594,-101.527488620873,
178.585485069079));
#46957=CARTESIAN_POINT('Ctrl Pts',(-98.6555115664906,-101.866154114362,
178.585485069079));
#46958=CARTESIAN_POINT('Ctrl Pts',(-99.6094074299589,-101.563252285373,
177.585485069079));
#46959=CARTESIAN_POINT('Ctrl Pts',(-99.6094074304457,-101.563252285196,
178.585485069079));
#46960=CARTESIAN_POINT('Ctrl Pts',(-98.6703932517879,-101.907141939062,
178.585485069079));
#46961=CARTESIAN_POINT('Ctrl Pts',(-99.6150688043333,-101.578639489318,
177.585485069079));
#46962=CARTESIAN_POINT('Ctrl Pts',(-99.6150688043334,-101.578639489318,
178.585485069079));
#46963=CARTESIAN_POINT('Ctrl Pts',(-98.6779325351968,-101.927603116461,
178.585485069079));
#46964=CARTESIAN_POINT('Ctrl Pts',(-99.6378999253588,-101.639952101619,
177.585485069079));
#46965=CARTESIAN_POINT('Ctrl Pts',(-99.6378999253585,-101.639952101619,
178.585485069079));
#46966=CARTESIAN_POINT('Ctrl Pts',(-98.7007636562219,-101.988915728762,
178.585485069079));
#46967=CARTESIAN_POINT('Ctrl Pts',(-99.6531206727089,-101.680827176486,
177.585485069079));
#46968=CARTESIAN_POINT('Ctrl Pts',(-99.653120672709,-101.680827176486,178.585485069079));
#46969=CARTESIAN_POINT('Ctrl Pts',(-98.7159844035723,-102.029790803628,
178.585485069079));
#46970=CARTESIAN_POINT('Ctrl Pts',(-99.6987829147594,-101.803452401085,
177.585485069079));
#46971=CARTESIAN_POINT('Ctrl Pts',(-99.6987829147592,-101.803452401085,
178.585485069079));
#46972=CARTESIAN_POINT('Ctrl Pts',(-98.7616466456226,-102.152416028228,
178.585485069079));
#46973=CARTESIAN_POINT('Ctrl Pts',(-99.7292244094599,-101.885202550819,
177.585485069079));
#46974=CARTESIAN_POINT('Ctrl Pts',(-99.7292244094612,-101.885202550819,
178.585485069079));
#46975=CARTESIAN_POINT('Ctrl Pts',(-98.7920881403248,-102.234166177961,
178.585485069079));
#46976=CARTESIAN_POINT('Ctrl Pts',(-99.7596659041602,-101.966952700553,
177.585485069079));
#46977=CARTESIAN_POINT('Ctrl Pts',(-99.7596659041602,-101.966952700553,
178.585485069079));
#46978=CARTESIAN_POINT('Ctrl Pts',(-98.8225296350236,-102.315916327695,
178.585485069079));
#46979=CARTESIAN_POINT('Ctrl Pts',(-98.3765170572744,-100.991065637145,
178.585485069079));
#46980=CARTESIAN_POINT('Ctrl Pts',(-98.4305822075695,-101.018191972391,
178.585485069079));
#46981=CARTESIAN_POINT('Ctrl Pts',(-98.4847274747232,-101.045274025794,
178.582547152259));
#46982=CARTESIAN_POINT('Ctrl Pts',(-98.5387005379516,-101.07219166779,178.576651720296));
#46983=CARTESIAN_POINT('Ctrl Pts',(-98.5902438653333,-101.097897543106,
178.571021686322));
#46984=CARTESIAN_POINT('Ctrl Pts',(-98.641630625025,-101.123454767852,178.562693776218));
#46985=CARTESIAN_POINT('Ctrl Pts',(-98.6926335233544,-101.148738472462,
178.551610199999));
#46986=CARTESIAN_POINT('Ctrl Pts',(-98.7263492605821,-101.16545239988,178.544283342985));
#46987=CARTESIAN_POINT('Ctrl Pts',(-98.7598970862398,-101.182046353722,
178.535751434339));
#46988=CARTESIAN_POINT('Ctrl Pts',(-98.7932079208523,-101.19847507901,178.525989701346));
#46989=CARTESIAN_POINT('Ctrl Pts',(-98.8292147103055,-101.216233434791,
178.51543791936));
#46990=CARTESIAN_POINT('Ctrl Pts',(-98.8647234933833,-101.233664780123,
178.503526033788));
#46991=CARTESIAN_POINT('Ctrl Pts',(-98.8997168217397,-101.250798523256,
178.490216331959));
#46992=CARTESIAN_POINT('Ctrl Pts',(-98.934244743073,-101.267704389684,178.477083647549));
#46993=CARTESIAN_POINT('Ctrl Pts',(-98.9682710919285,-101.284321222224,
178.462589629479));
#46994=CARTESIAN_POINT('Ctrl Pts',(-99.0017689542116,-101.300650006337,
178.446657516942));
#46995=CARTESIAN_POINT('Ctrl Pts',(-99.0341907378252,-101.316454247834,
178.431237204421));
#46996=CARTESIAN_POINT('Ctrl Pts',(-99.0661176319256,-101.331989156102,
178.414469133947));
#46997=CARTESIAN_POINT('Ctrl Pts',(-99.0975124519308,-101.347221299307,
178.396253114668));
#46998=CARTESIAN_POINT('Ctrl Pts',(-99.1254005310773,-101.360752041486,
178.380071789617));
#46999=CARTESIAN_POINT('Ctrl Pts',(-99.1528687077778,-101.37404373471,178.362747252573));
#47000=CARTESIAN_POINT('Ctrl Pts',(-99.1798801448296,-101.387044014541,
178.344193642566));
#47001=CARTESIAN_POINT('Ctrl Pts',(-99.2137741126018,-101.403356773642,
178.320912561354));
#47002=CARTESIAN_POINT('Ctrl Pts',(-99.2466864709949,-101.419082201428,
178.295876339252));
#47003=CARTESIAN_POINT('Ctrl Pts',(-99.2783014428484,-101.43413658413,178.26903067634));
#47004=CARTESIAN_POINT('Ctrl Pts',(-99.3088775986878,-101.448696304559,
178.24306711779));
#47005=CARTESIAN_POINT('Ctrl Pts',(-99.338240285646,-101.462628511189,178.215410332517));
#47006=CARTESIAN_POINT('Ctrl Pts',(-99.3660875946641,-101.475813840283,
178.186019035509));
#47007=CARTESIAN_POINT('Ctrl Pts',(-99.3925585906586,-101.488347503532,
178.158080360901));
#47008=CARTESIAN_POINT('Ctrl Pts',(-99.4176602614692,-101.500206193845,
178.12857375169));
#47009=CARTESIAN_POINT('Ctrl Pts',(-99.4411182957459,-101.511247128345,
178.097480701142));
#47010=CARTESIAN_POINT('Ctrl Pts',(-99.4583148829155,-101.519341003149,
178.074687045552));
#47011=CARTESIAN_POINT('Ctrl Pts',(-99.4746278674543,-101.526994593327,
178.051041097961));
#47012=CARTESIAN_POINT('Ctrl Pts',(-99.4899438535657,-101.534137339519,
178.026545021173));
#47013=CARTESIAN_POINT('Ctrl Pts',(-99.5101721875391,-101.543571002779,
177.994192235091));
#47014=CARTESIAN_POINT('Ctrl Pts',(-99.5284988040617,-101.552122304806,
177.960443704363));
#47015=CARTESIAN_POINT('Ctrl Pts',(-99.5445987150435,-101.559611735255,
177.9254913044));
#47016=CARTESIAN_POINT('Ctrl Pts',(-99.5598249635931,-101.566694751405,
177.892435598076));
#47017=CARTESIAN_POINT('Ctrl Pts',(-99.5730594840834,-101.572827664698,
177.858303807702));
#47018=CARTESIAN_POINT('Ctrl Pts',(-99.5840370353095,-101.577884571358,
177.823302561404));
#47019=CARTESIAN_POINT('Ctrl Pts',(-99.5949550980474,-101.582914074116,
177.788490990489));
#47020=CARTESIAN_POINT('Ctrl Pts',(-99.6036404116704,-101.586878730474,
177.752819756212));
#47021=CARTESIAN_POINT('Ctrl Pts',(-99.6098441942121,-101.589687356005,
177.716529959633));
#47022=CARTESIAN_POINT('Ctrl Pts',(-99.6160114909652,-101.592479463401,
177.680453591207));
#47023=CARTESIAN_POINT('Ctrl Pts',(-99.6197262175262,-101.594128716056,
177.643766413933));
#47024=CARTESIAN_POINT('Ctrl Pts',(-99.620758383797,-101.594584275658,177.606736088151));
#47025=CARTESIAN_POINT('Ctrl Pts',(-99.6209555024414,-101.594671276458,
177.599664196899));
#47026=CARTESIAN_POINT('Ctrl Pts',(-99.621054829477,-101.594714864612,177.592579867853));
#47027=CARTESIAN_POINT('Ctrl Pts',(-99.621054829477,-101.594714864612,177.585485069079));
#47028=CARTESIAN_POINT('Origin',(-99.2720912023343,-100.657578595475,174.385485069079));
#47029=CARTESIAN_POINT('Origin',(-98.8390996009298,-100.81881269208,174.385485069078));
#47030=CARTESIAN_POINT('Origin',(-101.649120271255,-99.7724387145074,177.585485069079));
#47031=CARTESIAN_POINT('Origin',(-98.839099600931,-100.818812692077,177.585485069078));
#47032=CARTESIAN_POINT('Origin',(-98.8390996009304,-100.818812692078,173.835485069079));
#47033=CARTESIAN_POINT('Ctrl Pts',(-97.8838106717875,-101.114486603435,
174.36571584829));
#47034=CARTESIAN_POINT('Ctrl Pts',(-97.8849135881754,-101.118050001404,
174.365742603133));
#47035=CARTESIAN_POINT('Ctrl Pts',(-97.8860364212679,-101.121607157985,
174.365777961194));
#47036=CARTESIAN_POINT('Ctrl Pts',(-97.8885814335997,-101.129515393127,
174.365875899567));
#47037=CARTESIAN_POINT('Ctrl Pts',(-97.8900136419527,-101.133863154473,
174.365942839133));
#47038=CARTESIAN_POINT('Ctrl Pts',(-97.895926912204,-101.151407824776,174.366266229089));
#47039=CARTESIAN_POINT('Ctrl Pts',(-97.9006535276767,-101.164519262059,
174.366630166537));
#47040=CARTESIAN_POINT('Ctrl Pts',(-97.9353481098766,-101.254802793895,
174.370007852721));
#47041=CARTESIAN_POINT('Ctrl Pts',(-97.9745478504433,-101.327964563021,
174.377064983029));
#47042=CARTESIAN_POINT('Ctrl Pts',(-98.0731118853643,-101.467848500997,
174.403591185806));
#47043=CARTESIAN_POINT('Ctrl Pts',(-98.1332873077329,-101.532286752824,
174.423968754122));
#47044=CARTESIAN_POINT('Ctrl Pts',(-98.2601167611847,-101.638089049953,
174.48329793291));
#47045=CARTESIAN_POINT('Ctrl Pts',(-98.3243130154484,-101.67900994078,174.520374455133));
#47046=CARTESIAN_POINT('Ctrl Pts',(-98.45418690728,-101.744830959462,174.61988553992));
#47047=CARTESIAN_POINT('Ctrl Pts',(-98.5164960369575,-101.766963654996,
174.681676275863));
#47048=CARTESIAN_POINT('Ctrl Pts',(-98.6272597346526,-101.797936714345,
174.83240435999));
#47049=CARTESIAN_POINT('Ctrl Pts',(-98.6719708237926,-101.805199932678,
174.920075475286));
#47050=CARTESIAN_POINT('Ctrl Pts',(-98.7291347063541,-101.813138240831,
175.101678439926));
#47051=CARTESIAN_POINT('Ctrl Pts',(-98.7431458989486,-101.814198490187,
175.193418679837));
#47052=CARTESIAN_POINT('Ctrl Pts',(-98.7431458989518,-101.814198490187,
175.285485069079));
#47053=CARTESIAN_POINT('Ctrl Pts',(-98.7431458989518,-101.814198490187,
176.685485069079));
#47054=CARTESIAN_POINT('Ctrl Pts',(-98.7431458989486,-101.814198490187,
176.776650914172));
#47055=CARTESIAN_POINT('Ctrl Pts',(-98.7294079789718,-101.813153557324,
176.867502767005));
#47056=CARTESIAN_POINT('Ctrl Pts',(-98.6730268299348,-101.805370421282,
177.048509953544));
#47057=CARTESIAN_POINT('Ctrl Pts',(-98.6285238159208,-101.798198724887,
177.136402953419));
#47058=CARTESIAN_POINT('Ctrl Pts',(-98.5180661808909,-101.767485380609,
177.287557268415));
#47059=CARTESIAN_POINT('Ctrl Pts',(-98.4558597070305,-101.745515778251,
177.349562701941));
#47060=CARTESIAN_POINT('Ctrl Pts',(-98.3258752989752,-101.67995039206,177.449617759738));
#47061=CARTESIAN_POINT('Ctrl Pts',(-98.2614711785115,-101.639064877108,
177.486951211427));
#47062=CARTESIAN_POINT('Ctrl Pts',(-98.1344522768478,-101.533418132759,
177.546546970785));
#47063=CARTESIAN_POINT('Ctrl Pts',(-98.0742734413384,-101.469197196162,
177.567003050164));
#47064=CARTESIAN_POINT('Ctrl Pts',(-97.9752073410398,-101.329171021278,
177.593784778556));
#47065=CARTESIAN_POINT('Ctrl Pts',(-97.9356541020267,-101.255545406551,
177.600926124503));
#47066=CARTESIAN_POINT('Ctrl Pts',(-97.900713297569,-101.164683712518,177.604335211391));
#47067=CARTESIAN_POINT('Ctrl Pts',(-97.8959658633087,-101.151520598178,
177.60470145546));
#47068=CARTESIAN_POINT('Ctrl Pts',(-97.8900295966086,-101.133911400201,
177.605026531602));
#47069=CARTESIAN_POINT('Ctrl Pts',(-97.8885931810068,-101.129551518366,
177.605093742951));
#47070=CARTESIAN_POINT('Ctrl Pts',(-97.8860414703018,-101.121623153065,
177.605192017933));
#47071=CARTESIAN_POINT('Ctrl Pts',(-97.8849160678685,-101.118058013011,
177.605227474873));
#47072=CARTESIAN_POINT('Ctrl Pts',(-97.8838106717876,-101.114486603435,
177.605254289869));
#47073=CARTESIAN_POINT('Ctrl Pts',(-97.8932302579351,-102.399362986829,
177.685485069079));
#47074=CARTESIAN_POINT('Ctrl Pts',(-98.8303665270718,-102.050399359687,
177.685485069079));
#47075=CARTESIAN_POINT('Ctrl Pts',(-98.8303665270718,-102.050399359687,
176.685485069079));
#47076=CARTESIAN_POINT('Ctrl Pts',(-97.8730369312331,-102.34513412923,177.685485069079));
#47077=CARTESIAN_POINT('Ctrl Pts',(-98.8109710951273,-101.998313235765,
177.685485069079));
#47078=CARTESIAN_POINT('Ctrl Pts',(-98.8109710951313,-101.998313235766,
176.685485069079));
#47079=CARTESIAN_POINT('Ctrl Pts',(-97.8527181088294,-102.290940987051,
177.685485069079));
#47080=CARTESIAN_POINT('Ctrl Pts',(-98.7883769389248,-101.937964302332,
177.685485069079));
#47081=CARTESIAN_POINT('Ctrl Pts',(-98.7883769378891,-101.937964302715,
176.685485069079));
#47082=CARTESIAN_POINT('Ctrl Pts',(-97.8126362132817,-102.182375180482,
177.685485069079));
#47083=CARTESIAN_POINT('Ctrl Pts',(-98.7531924801363,-101.842663688618,
177.685485069079));
#47084=CARTESIAN_POINT('Ctrl Pts',(-98.7531924811721,-101.842663688236,
176.685485069079));
#47085=CARTESIAN_POINT('Ctrl Pts',(-97.7931741603528,-102.127898788951,
177.685485069079));
#47086=CARTESIAN_POINT('Ctrl Pts',(-98.7358013339773,-101.794005894027,
177.685485069079));
#47087=CARTESIAN_POINT('Ctrl Pts',(-98.7358013331175,-101.794005894326,
176.685485069079));
#47088=CARTESIAN_POINT('Ctrl Pts',(-97.7361407722699,-101.964017467933,
177.685485069079));
#47089=CARTESIAN_POINT('Ctrl Pts',(-98.6842094799426,-101.645760425827,
177.685485069079));
#47090=CARTESIAN_POINT('Ctrl Pts',(-98.6842094816623,-101.645760425228,
176.685485069079));
#47091=CARTESIAN_POINT('Ctrl Pts',(-97.6999002805471,-101.854167720931,
177.685485069079));
#47092=CARTESIAN_POINT('Ctrl Pts',(-98.6505921303461,-101.54395040367,177.685485069079));
#47093=CARTESIAN_POINT('Ctrl Pts',(-98.6505921292553,-101.543950404017,
176.685485069079));
#47094=CARTESIAN_POINT('Ctrl Pts',(-97.5945716173814,-101.523484475616,
177.685485069079));
#47095=CARTESIAN_POINT('Ctrl Pts',(-98.5516872373819,-101.233434821501,
177.685485069079));
#47096=CARTESIAN_POINT('Ctrl Pts',(-98.5516872395635,-101.233434820807,
176.685485069079));
#47097=CARTESIAN_POINT('Ctrl Pts',(-97.5287765043858,-101.301550314339,
177.685485069079));
#47098=CARTESIAN_POINT('Ctrl Pts',(-98.4883057294024,-101.019857554285,
177.685485069079));
#47099=CARTESIAN_POINT('Ctrl Pts',(-98.4883057284991,-101.019857554543,
176.685485069079));
#47100=CARTESIAN_POINT('Ctrl Pts',(-97.337669387055,-100.633649414688,177.685485069079));
#47101=CARTESIAN_POINT('Ctrl Pts',(-98.3028651239191,-100.371760565047,
177.685485069079));
#47102=CARTESIAN_POINT('Ctrl Pts',(-98.3028651257257,-100.37176056453,176.685485069079));
#47103=CARTESIAN_POINT('Ctrl Pts',(-97.2185417746632,-100.185615621848,
177.685485069079));
#47104=CARTESIAN_POINT('Ctrl Pts',(-98.1852802927309,-99.9298032981305,
177.685485069079));
#47105=CARTESIAN_POINT('Ctrl Pts',(-98.1852802922409,-99.9298032982608,
176.685485069079));
#47106=CARTESIAN_POINT('Ctrl Pts',(-96.8691183172638,-98.8388539217306,
177.685485069079));
#47107=CARTESIAN_POINT('Ctrl Pts',(-97.8394941595671,-98.5970607167195,
177.685485069079));
#47108=CARTESIAN_POINT('Ctrl Pts',(-97.839494160547,-98.5970607164588,176.685485069079));
#47109=CARTESIAN_POINT('Ctrl Pts',(-96.6472483679273,-97.9373097658594,
177.685485069079));
#47110=CARTESIAN_POINT('Ctrl Pts',(-97.6181791273144,-97.6979435767543,
177.685485069079));
#47111=CARTESIAN_POINT('Ctrl Pts',(-97.6181791271038,-97.6979435768059,
176.685485069079));
#47112=CARTESIAN_POINT('Ctrl Pts',(-95.9849221665839,-95.2315797811142,
177.685485069079));
#47113=CARTESIAN_POINT('Ctrl Pts',(-96.9570275992017,-94.9970123582629,
177.685485069079));
#47114=CARTESIAN_POINT('Ctrl Pts',(-96.9570275996231,-94.9970123581598,
176.685485069079));
#47115=CARTESIAN_POINT('Ctrl Pts',(-95.5493747573727,-93.4257532338304,
177.685485069079));
#47116=CARTESIAN_POINT('Ctrl Pts',(-96.5209465833698,-93.1889913671421,
177.685485069079));
#47117=CARTESIAN_POINT('Ctrl Pts',(-96.5209465833055,-93.1889913671838,
176.685485069079));
#47118=CARTESIAN_POINT('Ctrl Pts',(-94.2152215208916,-88.0174687972257,
177.685485069079));
#47119=CARTESIAN_POINT('Ctrl Pts',(-95.18476174991,-87.7724714040589,177.685485069079));
#47120=CARTESIAN_POINT('Ctrl Pts',(-95.1847617500387,-87.7724714039756,
176.685485069079));
#47121=CARTESIAN_POINT('Ctrl Pts',(-93.2924266975675,-84.4230957726183,
177.685485069079));
#47122=CARTESIAN_POINT('Ctrl Pts',(-94.2595291227605,-84.1684584467021,
177.685485069079));
#47123=CARTESIAN_POINT('Ctrl Pts',(-94.259529122677,-84.1684584467251,176.685485069079));
#47124=CARTESIAN_POINT('Ctrl Pts',(-91.3239661578598,-77.2754177587244,
177.685485069079));
#47125=CARTESIAN_POINT('Ctrl Pts',(-92.2850778836019,-76.9990276012334,
177.685485069079));
#47126=CARTESIAN_POINT('Ctrl Pts',(-92.2850778836854,-76.9990276012104,
176.685485069079));
#47127=CARTESIAN_POINT('Ctrl Pts',(-90.2802592515923,-73.7220857400795,
177.685485069079));
#47128=CARTESIAN_POINT('Ctrl Pts',(-91.2377226352478,-73.433138928738,177.685485069079));
#47129=CARTESIAN_POINT('Ctrl Pts',(-91.2377226351847,-73.4331389287581,
176.685485069079));
#47130=CARTESIAN_POINT('Ctrl Pts',(-88.0433318090029,-66.6938040952403,
177.685485069079));
#47131=CARTESIAN_POINT('Ctrl Pts',(-88.9916685821912,-66.37618206286,177.685485069079));
#47132=CARTESIAN_POINT('Ctrl Pts',(-88.9916685822543,-66.3761820628399,
176.685485069079));
#47133=CARTESIAN_POINT('Ctrl Pts',(-86.849942999413,-63.2159635981179,177.685485069079));
#47134=CARTESIAN_POINT('Ctrl Pts',(-87.7928037540024,-62.8821750496115,
177.685485069079));
#47135=CARTESIAN_POINT('Ctrl Pts',(-87.7928037541667,-62.8821750495468,
176.685485069079));
#47136=CARTESIAN_POINT('Ctrl Pts',(-85.5577653075821,-59.7858708180287,
177.685485069079));
#47137=CARTESIAN_POINT('Ctrl Pts',(-86.4935648641577,-59.4333382806468,
177.685485069079));
#47138=CARTESIAN_POINT('Ctrl Pts',(-86.4935648641577,-59.4333382806468,
176.685485069079));
#47139=CARTESIAN_POINT('Origin',(-85.5577653075866,-59.7858708180409,176.685485069079));
#47140=CARTESIAN_POINT('Ctrl Pts',(-85.5194531411007,-59.8223115460841,
177.685438410949));
#47141=CARTESIAN_POINT('Ctrl Pts',(-86.4988068431487,-59.4471035664831,
177.735457988727));
#47142=CARTESIAN_POINT('Ctrl Pts',(-86.5441160166797,-59.5676907797451,
176.694509775823));
#47143=CARTESIAN_POINT('Ctrl Pts',(-85.5488285264639,-59.7938358236938,
177.685474105637));
#47144=CARTESIAN_POINT('Ctrl Pts',(-86.4967892966262,-59.4420366768795,
177.6973962827));
#47145=CARTESIAN_POINT('Ctrl Pts',(-86.499952014399,-59.4501665620726,176.678332308422));
#47146=CARTESIAN_POINT('Ctrl Pts',(-85.5871411152688,-59.7596096112386,
177.685523612831));
#47147=CARTESIAN_POINT('Ctrl Pts',(-86.4893362171423,-59.4220524652253,
177.646796562209));
#47148=CARTESIAN_POINT('Ctrl Pts',(-86.4548043581822,-59.3304223997585,
176.684724459335));
#47149=CARTESIAN_POINT('Ctrl Pts',(-85.6675280904232,-59.6585983136463,
177.68561487818));
#47150=CARTESIAN_POINT('Ctrl Pts',(-86.4551632269365,-59.3311831648032,
177.560550921871));
#47151=CARTESIAN_POINT('Ctrl Pts',(-86.3837085441107,-59.1424265153221,
176.72104467469));
#47152=CARTESIAN_POINT('Ctrl Pts',(-85.7032857420514,-59.609212897412,177.685652756804));
#47153=CARTESIAN_POINT('Ctrl Pts',(-86.4377267349023,-59.2848714957092,
177.527403265691));
#47154=CARTESIAN_POINT('Ctrl Pts',(-86.356803937052,-59.0714212354019,176.74128997663));
#47155=CARTESIAN_POINT('Ctrl Pts',(-85.7785946848509,-59.4648705863235,
177.685728562076));
#47156=CARTESIAN_POINT('Ctrl Pts',(-86.3883211207893,-59.1541829177556,
177.466627726095));
#47157=CARTESIAN_POINT('Ctrl Pts',(-86.3035833251825,-58.9312229886497,
176.788538683646));
#47158=CARTESIAN_POINT('Ctrl Pts',(-85.8199795319615,-59.369025485855,177.685766507573));
#47159=CARTESIAN_POINT('Ctrl Pts',(-86.3570787764338,-59.0717098514556,
177.439003405769));
#47160=CARTESIAN_POINT('Ctrl Pts',(-86.2773224730263,-58.8621727937877,
176.815857196747));
#47161=CARTESIAN_POINT('Ctrl Pts',(-85.8527453811609,-59.1638631347099,
177.685812659431));
#47162=CARTESIAN_POINT('Ctrl Pts',(-86.2952455717908,-58.9091065789535,
177.408732140999));
#47163=CARTESIAN_POINT('Ctrl Pts',(-86.237244648596,-58.7569891525569,176.851005000506));
#47164=CARTESIAN_POINT('Ctrl Pts',(-85.8580983310819,-59.0850699288534,
177.685825854228));
#47165=CARTESIAN_POINT('Ctrl Pts',(-86.2725674790216,-58.849546544774,177.400568011683));
#47166=CARTESIAN_POINT('Ctrl Pts',(-86.2237570173259,-58.7216236519169,
176.861619635495));
#47167=CARTESIAN_POINT('Ctrl Pts',(-85.8446620596993,-58.9106340093845,
177.685845148542));
#47168=CARTESIAN_POINT('Ctrl Pts',(-86.2230104183943,-58.7196046722724,
177.389314593047));
#47169=CARTESIAN_POINT('Ctrl Pts',(-86.1961425897331,-58.6492878843728,
176.87708230681));
#47170=CARTESIAN_POINT('Ctrl Pts',(-85.8247359731533,-58.8148969021221,
177.685850622447));
#47171=CARTESIAN_POINT('Ctrl Pts',(-86.1958236366334,-58.6484192889276,
177.386205525725));
#47172=CARTESIAN_POINT('Ctrl Pts',(-86.181985786926,-58.6122403466145,176.881690814559));
#47173=CARTESIAN_POINT('Ctrl Pts',(-85.757798456551,-58.6355045475111,177.685851182201));
#47174=CARTESIAN_POINT('Ctrl Pts',(-86.1425085870774,-58.5090309919607,
177.385885667039));
#47175=CARTESIAN_POINT('Ctrl Pts',(-86.1541477137945,-58.5394616866261,
176.882160986323));
#47176=CARTESIAN_POINT('Ctrl Pts',(-85.7111764310999,-58.5517673494884,
177.685846421581));
#47177=CARTESIAN_POINT('Ctrl Pts',(-86.1158285918039,-58.4393825623272,
177.388583808311));
#47178=CARTESIAN_POINT('Ctrl Pts',(-86.1403253895075,-58.5033607487595,
176.878144292243));
#47179=CARTESIAN_POINT('Ctrl Pts',(-85.6070035272959,-58.4105885808773,
177.685828410447));
#47180=CARTESIAN_POINT('Ctrl Pts',(-86.0659936678227,-58.3094686550687,
177.39904204685));
#47181=CARTESIAN_POINT('Ctrl Pts',(-86.1128226609236,-58.4315984586357,
176.86365543919));
#47182=CARTESIAN_POINT('Ctrl Pts',(-85.549953411443,-58.3529281116889,177.685815542119));
#47183=CARTESIAN_POINT('Ctrl Pts',(-86.0425829131345,-58.2485372045759,
177.406935364112));
#47184=CARTESIAN_POINT('Ctrl Pts',(-86.0991214598369,-58.3958830429589,
176.853266846028));
#47185=CARTESIAN_POINT('Ctrl Pts',(-85.3866542001269,-58.2165474304525,
177.685769931045));
#47186=CARTESIAN_POINT('Ctrl Pts',(-85.9787922610718,-58.0827294956763,
177.436623506163));
#47187=CARTESIAN_POINT('Ctrl Pts',(-86.0584515948782,-58.2899677801205,
176.818373491556));
#47188=CARTESIAN_POINT('Ctrl Pts',(-85.2896402982616,-58.1708177059058,
177.685731747951));
#47189=CARTESIAN_POINT('Ctrl Pts',(-85.9462013915549,-57.9983452958113,
177.46423345489));
#47190=CARTESIAN_POINT('Ctrl Pts',(-86.0316755766063,-58.220368101616,176.790702111615));
#47191=CARTESIAN_POINT('Ctrl Pts',(-85.1344296615373,-58.1114104723673,
177.685655451055));
#47192=CARTESIAN_POINT('Ctrl Pts',(-85.8946772447352,-57.8652228457512,
177.525111657089));
#47193=CARTESIAN_POINT('Ctrl Pts',(-85.9773869546852,-58.0795219938874,
176.74280243967));
#47194=CARTESIAN_POINT('Ctrl Pts',(-85.0738866036248,-58.0980831033533,
177.68561727497));
#47195=CARTESIAN_POINT('Ctrl Pts',(-85.8763844336074,-57.818157058371,177.558407398017));
#47196=CARTESIAN_POINT('Ctrl Pts',(-85.9499076944264,-58.0083634795133,
176.722185026019));
#47197=CARTESIAN_POINT('Ctrl Pts',(-84.9441455970151,-58.0757351762659,
177.685524740537));
#47198=CARTESIAN_POINT('Ctrl Pts',(-85.8402711553428,-57.7253572143701,
177.645672245051));
#47199=CARTESIAN_POINT('Ctrl Pts',(-85.8765913231287,-57.8188881891832,
176.684878031502));
#47200=CARTESIAN_POINT('Ctrl Pts',(-84.8918836039343,-58.0758297218312,
177.685474402246));
#47201=CARTESIAN_POINT('Ctrl Pts',(-85.8321927700424,-57.7047829333621,
177.697086633613));
#47202=CARTESIAN_POINT('Ctrl Pts',(-85.8297285808071,-57.6981502619506,
176.677860001849));
#47203=CARTESIAN_POINT('Ctrl Pts',(-84.8483096915888,-58.074185324701,177.685436168594));
#47204=CARTESIAN_POINT('Ctrl Pts',(-85.8301986118354,-57.6993383348146,
177.737896293016));
#47205=CARTESIAN_POINT('Ctrl Pts',(-85.7812152810651,-57.5735987346764,
176.695029611126));
#47206=CARTESIAN_POINT('Origin',(-84.9035795890714,-58.0758081979738,176.685485069078));
#47207=CARTESIAN_POINT('Ctrl Pts',(-84.9035795890714,-58.0758081979738,
177.685485069079));
#47208=CARTESIAN_POINT('Ctrl Pts',(-85.8357032382114,-57.7136680279926,
177.685485069079));
#47209=CARTESIAN_POINT('Ctrl Pts',(-85.8357032382114,-57.7136680279926,
176.685485069079));
#47210=CARTESIAN_POINT('Ctrl Pts',(-83.6957353880445,-54.9669011015685,
177.685485069079));
#47211=CARTESIAN_POINT('Ctrl Pts',(-84.6208766884138,-54.5867888507553,
177.685485069265));
#47212=CARTESIAN_POINT('Ctrl Pts',(-84.620876688336,-54.586788850792,176.685485069079));
#47213=CARTESIAN_POINT('Ctrl Pts',(-82.4022289102314,-51.899353553254,177.685485069079));
#47214=CARTESIAN_POINT('Ctrl Pts',(-83.3189771390602,-51.4990128922003,
177.685485069079));
#47215=CARTESIAN_POINT('Ctrl Pts',(-83.3189771388799,-51.4990128922617,
176.685485069079));
#47216=CARTESIAN_POINT('Ctrl Pts',(-80.2861211752646,-47.3832252372826,
177.685485069079));
#47217=CARTESIAN_POINT('Ctrl Pts',(-81.1860310864128,-46.9469487861368,
177.685485069079));
#47218=CARTESIAN_POINT('Ctrl Pts',(-81.1860310865029,-46.9469487861061,
176.685485069079));
#47219=CARTESIAN_POINT('Ctrl Pts',(-79.5512148812064,-45.8921459027875,
177.685485069079));
#47220=CARTESIAN_POINT('Ctrl Pts',(-80.4447931525142,-45.4429556181932,
177.68548506901));
#47221=CARTESIAN_POINT('Ctrl Pts',(-80.4447931524336,-45.4429556182301,
176.685485069033));
#47222=CARTESIAN_POINT('Ctrl Pts',(-78.3954041227117,-43.6813988570481,
177.685485069079));
#47223=CARTESIAN_POINT('Ctrl Pts',(-79.2779055104375,-43.2110215506448,
177.685485069114));
#47224=CARTESIAN_POINT('Ctrl Pts',(-79.2779055104779,-43.2110215506263,
176.685485069102));
#47225=CARTESIAN_POINT('Ctrl Pts',(-78.0011966023895,-42.9488090664747,
177.685485069079));
#47226=CARTESIAN_POINT('Ctrl Pts',(-78.8797401691368,-42.4710653373528,
177.685485069022));
#47227=CARTESIAN_POINT('Ctrl Pts',(-78.8797401690956,-42.4710653373763,
176.685485069033));
#47228=CARTESIAN_POINT('Ctrl Pts',(-77.3950072327152,-41.8571257984251,
177.685485069079));
#47229=CARTESIAN_POINT('Ctrl Pts',(-78.2671250050753,-41.3678098897351,
177.685485069108));
#47230=CARTESIAN_POINT('Ctrl Pts',(-78.267125005096,-41.3678098897234,176.685485069103));
#47231=CARTESIAN_POINT('Ctrl Pts',(-77.1904617586198,-41.4944329040509,
177.685485069079));
#47232=CARTESIAN_POINT('Ctrl Pts',(-78.0603558525197,-41.0011723956222,
177.685485069051));
#47233=CARTESIAN_POINT('Ctrl Pts',(-78.0603558525001,-41.0011723956339,
176.685485069056));
#47234=CARTESIAN_POINT('Ctrl Pts',(-76.776124475483,-40.7715864905627,177.685485069079));
#47235=CARTESIAN_POINT('Ctrl Pts',(-77.6413892786657,-40.270249793146,177.685485069108));
#47236=CARTESIAN_POINT('Ctrl Pts',(-77.6413892786852,-40.2702497931344,
176.685485069103));
#47237=CARTESIAN_POINT('Ctrl Pts',(-76.5654763654172,-40.4118964032511,
177.685485069079));
#47238=CARTESIAN_POINT('Ctrl Pts',(-77.427270789845,-39.904637716433,177.685485069079));
#47239=CARTESIAN_POINT('Ctrl Pts',(-77.4272707898366,-39.9046377164379,
176.685485069079));
#47240=CARTESIAN_POINT('Ctrl Pts',(-76.3543296174317,-40.0523497550927,
177.685485069079));
#47241=CARTESIAN_POINT('Ctrl Pts',(-77.2166317829811,-39.5459556642022,
177.685485069079));
#47242=CARTESIAN_POINT('Ctrl Pts',(-77.2166317829811,-39.5459556642022,
176.685485069079));
#47243=CARTESIAN_POINT('Ctrl Pts',(-85.5577653075812,-59.7858708180263,
174.285485069079));
#47244=CARTESIAN_POINT('Ctrl Pts',(-86.4935648641568,-59.4333382806444,
174.285485069079));
#47245=CARTESIAN_POINT('Ctrl Pts',(-86.4935648641568,-59.4333382806444,
175.285485069079));
#47246=CARTESIAN_POINT('Ctrl Pts',(-86.8499429992757,-63.2159635981751,
174.285485069079));
#47247=CARTESIAN_POINT('Ctrl Pts',(-87.7928037537602,-62.8821750497275,
174.285485068927));
#47248=CARTESIAN_POINT('Ctrl Pts',(-87.7928037541746,-62.8821750495676,
175.285485068927));
#47249=CARTESIAN_POINT('Ctrl Pts',(-88.0433318089691,-66.6938040952401,
174.285485069079));
#47250=CARTESIAN_POINT('Ctrl Pts',(-88.9916685821573,-66.3761820628341,
174.285485069079));
#47251=CARTESIAN_POINT('Ctrl Pts',(-88.9916685822437,-66.3761820628066,
175.285485069079));
#47252=CARTESIAN_POINT('Ctrl Pts',(-90.2802592516248,-73.7220857400759,
174.285485069079));
#47253=CARTESIAN_POINT('Ctrl Pts',(-91.2377226352804,-73.4331389287601,
174.285485069079));
#47254=CARTESIAN_POINT('Ctrl Pts',(-91.2377226351941,-73.4331389287876,
175.285485069079));
#47255=CARTESIAN_POINT('Ctrl Pts',(-91.3239661578861,-77.2754177587261,
174.285485069079));
#47256=CARTESIAN_POINT('Ctrl Pts',(-92.2850778836539,-76.9990276012609,
174.285485069079));
#47257=CARTESIAN_POINT('Ctrl Pts',(-92.2850778836961,-76.9990276012493,
175.285485069079));
#47258=CARTESIAN_POINT('Ctrl Pts',(-93.2924266975406,-84.423095772614,174.285485069079));
#47259=CARTESIAN_POINT('Ctrl Pts',(-94.2595291227079,-84.1684584466722,
174.285485069079));
#47260=CARTESIAN_POINT('Ctrl Pts',(-94.2595291226657,-84.1684584466838,
175.285485069079));
#47261=CARTESIAN_POINT('Ctrl Pts',(-94.2152215209114,-88.0174687973044,
174.285485069079));
#47262=CARTESIAN_POINT('Ctrl Pts',(-95.1847617499297,-87.772471404086,174.285485069079));
#47263=CARTESIAN_POINT('Ctrl Pts',(-95.1847617500581,-87.7724714040543,
175.285485069079));
#47264=CARTESIAN_POINT('Ctrl Pts',(-95.5493747573626,-93.4257532337901,
174.285485069079));
#47265=CARTESIAN_POINT('Ctrl Pts',(-96.5209465833597,-93.1889913671276,
174.285485069079));
#47266=CARTESIAN_POINT('Ctrl Pts',(-96.5209465832955,-93.1889913671434,
175.285485069079));
#47267=CARTESIAN_POINT('Ctrl Pts',(-95.9849221665606,-95.2315797810471,
174.285485069079));
#47268=CARTESIAN_POINT('Ctrl Pts',(-96.9570275991784,-94.997012358183,174.285485069079));
#47269=CARTESIAN_POINT('Ctrl Pts',(-96.9570275996033,-94.997012358079,175.285485069079));
#47270=CARTESIAN_POINT('Ctrl Pts',(-96.6472483679388,-97.9373097658926,
174.285485069079));
#47271=CARTESIAN_POINT('Ctrl Pts',(-97.618179127326,-97.6979435767939,174.285485069079));
#47272=CARTESIAN_POINT('Ctrl Pts',(-97.6181791271135,-97.6979435768459,
175.285485069079));
#47273=CARTESIAN_POINT('Ctrl Pts',(-96.8691183172565,-98.8388539217272,
174.285485069079));
#47274=CARTESIAN_POINT('Ctrl Pts',(-97.8394941595598,-98.5970607167033,
174.285485069079));
#47275=CARTESIAN_POINT('Ctrl Pts',(-97.8394941605458,-98.5970607164539,
175.285485069079));
#47276=CARTESIAN_POINT('Ctrl Pts',(-97.2185417746667,-100.185615621849,
174.285485069079));
#47277=CARTESIAN_POINT('Ctrl Pts',(-98.1852802927345,-99.9298032981384,
174.285485069079));
#47278=CARTESIAN_POINT('Ctrl Pts',(-98.1852802922415,-99.9298032982631,
175.285485069079));
#47279=CARTESIAN_POINT('Ctrl Pts',(-97.3376693870452,-100.633649414677,
174.285485069079));
#47280=CARTESIAN_POINT('Ctrl Pts',(-98.3028651239093,-100.371760565043,
174.285485069073));
#47281=CARTESIAN_POINT('Ctrl Pts',(-98.3028651257231,-100.371760564521,
175.285485069079));
#47282=CARTESIAN_POINT('Ctrl Pts',(-97.5287765043906,-101.301550314344,
174.285485069079));
#47283=CARTESIAN_POINT('Ctrl Pts',(-98.4883057294072,-101.019857554286,
174.285485069083));
#47284=CARTESIAN_POINT('Ctrl Pts',(-98.4883057285003,-101.019857554548,
175.285485069079));
#47285=CARTESIAN_POINT('Ctrl Pts',(-97.5945716173798,-101.523484475618,
174.285485069079));
#47286=CARTESIAN_POINT('Ctrl Pts',(-98.5516872373803,-101.233434821505,
174.285485069079));
#47287=CARTESIAN_POINT('Ctrl Pts',(-98.5516872395642,-101.23343482081,175.285485069079));
#47288=CARTESIAN_POINT('Ctrl Pts',(-97.6999002805479,-101.85416772093,174.285485069079));
#47289=CARTESIAN_POINT('Ctrl Pts',(-98.6505921303469,-101.543950403668,
174.285485069079));
#47290=CARTESIAN_POINT('Ctrl Pts',(-98.6505921292549,-101.543950404016,
175.285485069079));
#47291=CARTESIAN_POINT('Ctrl Pts',(-97.7361407722666,-101.964017467932,
174.285485069079));
#47292=CARTESIAN_POINT('Ctrl Pts',(-98.6842094799393,-101.645760425825,
174.285485069079));
#47293=CARTESIAN_POINT('Ctrl Pts',(-98.6842094816616,-101.645760425226,
175.285485069079));
#47294=CARTESIAN_POINT('Ctrl Pts',(-97.7931741603545,-102.127898788952,
174.285485069079));
#47295=CARTESIAN_POINT('Ctrl Pts',(-98.7358013339789,-101.794005894028,
174.285485069079));
#47296=CARTESIAN_POINT('Ctrl Pts',(-98.7358013331178,-101.794005894327,
175.285485069079));
#47297=CARTESIAN_POINT('Ctrl Pts',(-97.8126362132817,-102.182375180481,
174.285485069079));
#47298=CARTESIAN_POINT('Ctrl Pts',(-98.7531924801367,-101.842663688617,
174.285485069079));
#47299=CARTESIAN_POINT('Ctrl Pts',(-98.7531924811716,-101.842663688235,
175.285485069079));
#47300=CARTESIAN_POINT('Ctrl Pts',(-97.8527181088293,-102.290940987052,
174.285485069079));
#47301=CARTESIAN_POINT('Ctrl Pts',(-98.7883769389244,-101.937964302334,
174.285485069079));
#47302=CARTESIAN_POINT('Ctrl Pts',(-98.7883769378895,-101.937964302716,
175.285485069079));
#47303=CARTESIAN_POINT('Ctrl Pts',(-97.873036931237,-102.345134129228,174.285485069079));
#47304=CARTESIAN_POINT('Ctrl Pts',(-98.8109710951308,-101.998313235763,
174.285485069079));
#47305=CARTESIAN_POINT('Ctrl Pts',(-98.810971095131,-101.998313235765,175.285485069079));
#47306=CARTESIAN_POINT('Ctrl Pts',(-97.8932302579351,-102.399362986829,
174.285485069079));
#47307=CARTESIAN_POINT('Ctrl Pts',(-98.8303665270718,-102.050399359687,
174.285485069079));
#47308=CARTESIAN_POINT('Ctrl Pts',(-98.8303665270718,-102.050399359687,
175.285485069079));
#47309=CARTESIAN_POINT('Origin',(-85.5577653075812,-59.7858708180264,175.285485069079));
#47310=CARTESIAN_POINT('Ctrl Pts',(-86.549995003282,-59.5833376285491,175.274170498514));
#47311=CARTESIAN_POINT('Ctrl Pts',(-86.499087005688,-59.4478052525176,174.231213939548));
#47312=CARTESIAN_POINT('Ctrl Pts',(-85.5163014695733,-59.8258007915048,
174.285496900648));
#47313=CARTESIAN_POINT('Ctrl Pts',(-86.5039652636174,-59.4608115109789,
175.293174078778));
#47314=CARTESIAN_POINT('Ctrl Pts',(-86.4974436030401,-59.4437917418642,
174.269738655091));
#47315=CARTESIAN_POINT('Ctrl Pts',(-85.5461481361416,-59.7965609490947,
174.285488532754));
#47316=CARTESIAN_POINT('Ctrl Pts',(-86.4567528143649,-59.3355746263436,
175.287241072843));
#47317=CARTESIAN_POINT('Ctrl Pts',(-86.4902980810653,-59.4246102748182,
174.322388145275));
#47318=CARTESIAN_POINT('Ctrl Pts',(-85.5856213811138,-59.7621229158345,
174.28547663711));
#47319=CARTESIAN_POINT('Ctrl Pts',(-86.3837085441054,-59.1424265153082,
175.249925463467));
#47320=CARTESIAN_POINT('Ctrl Pts',(-86.4551137649122,-59.3310525045627,
174.411000335328));
#47321=CARTESIAN_POINT('Ctrl Pts',(-85.6681540564035,-59.6583380432654,
174.285454887567));
#47322=CARTESIAN_POINT('Ctrl Pts',(-86.356803937048,-59.0714212353912,175.229680161526));
#47323=CARTESIAN_POINT('Ctrl Pts',(-86.4376719251528,-59.2847269239036,
174.444099314138));
#47324=CARTESIAN_POINT('Ctrl Pts',(-85.703882282356,-59.6089493866821,174.285446138593));
#47325=CARTESIAN_POINT('Ctrl Pts',(-86.303583325178,-58.9312229886379,175.182431454508));
#47326=CARTESIAN_POINT('Ctrl Pts',(-86.3882664257975,-59.1540390056827,
174.504780092467));
#47327=CARTESIAN_POINT('Ctrl Pts',(-85.7791143736295,-59.4646057043272,
174.285428517499));
#47328=CARTESIAN_POINT('Ctrl Pts',(-86.2773224730233,-58.8621727937798,
175.155112941408));
#47329=CARTESIAN_POINT('Ctrl Pts',(-86.3570286560902,-59.0715781744698,
174.532358329031));
#47330=CARTESIAN_POINT('Ctrl Pts',(-85.8204497401368,-59.3687651284942,
174.285419843032));
#47331=CARTESIAN_POINT('Ctrl Pts',(-86.2372446485919,-58.756989152546,175.11996513765));
#47332=CARTESIAN_POINT('Ctrl Pts',(-86.2952103972096,-58.9090143275485,
174.562576229961));
#47333=CARTESIAN_POINT('Ctrl Pts',(-85.8531468169556,-59.1636319687109,
174.285409009404));
#47334=CARTESIAN_POINT('Ctrl Pts',(-86.2237570173223,-58.7216236519073,
175.109350502661));
#47335=CARTESIAN_POINT('Ctrl Pts',(-86.2725381980377,-58.849469804911,174.570725436989));
#47336=CARTESIAN_POINT('Ctrl Pts',(-85.8584784511242,-59.0848538815999,
174.285406058599));
#47337=CARTESIAN_POINT('Ctrl Pts',(-86.1961425897295,-58.6492878843634,
175.093887831347));
#47338=CARTESIAN_POINT('Ctrl Pts',(-86.2229945554986,-58.7195631569009,
174.581957969401));
#47339=CARTESIAN_POINT('Ctrl Pts',(-85.845014636378,-58.9104559691449,174.285401468371));
#47340=CARTESIAN_POINT('Ctrl Pts',(-86.1819857869222,-58.6122403466045,
175.089279323599));
#47341=CARTESIAN_POINT('Ctrl Pts',(-86.1958155063122,-58.6483980322719,
174.585061035853));
#47342=CARTESIAN_POINT('Ctrl Pts',(-85.8250834731818,-58.8147409947177,
174.285400256228));
#47343=CARTESIAN_POINT('Ctrl Pts',(-86.1541477137916,-58.5394616866186,
175.088809151837));
#47344=CARTESIAN_POINT('Ctrl Pts',(-86.142515422188,-58.5090488624724,174.585380285109));
#47345=CARTESIAN_POINT('Ctrl Pts',(-85.7581588973064,-58.6353860619252,
174.285400134323));
#47346=CARTESIAN_POINT('Ctrl Pts',(-86.1403253895043,-58.5033607487514,
175.092825845917));
#47347=CARTESIAN_POINT('Ctrl Pts',(-86.115843038762,-58.4394202933868,174.582687361069));
#47348=CARTESIAN_POINT('Ctrl Pts',(-85.7115539539042,-58.5516625188447,
174.285401185141));
#47349=CARTESIAN_POINT('Ctrl Pts',(-86.1128226609207,-58.431598458628,175.10731469897));
#47350=CARTESIAN_POINT('Ctrl Pts',(-86.0660217014019,-58.3095417665191,
174.572248593736));
#47351=CARTESIAN_POINT('Ctrl Pts',(-85.6074253887782,-58.4104956771806,
174.28540545462));
#47352=CARTESIAN_POINT('Ctrl Pts',(-86.0991214598344,-58.3958830429522,
175.117703292133));
#47353=CARTESIAN_POINT('Ctrl Pts',(-86.0426171221911,-58.2486263572438,
174.564369775238));
#47354=CARTESIAN_POINT('Ctrl Pts',(-85.5504013860293,-58.3528332272351,
174.28540834039));
#47355=CARTESIAN_POINT('Ctrl Pts',(-86.0584515948751,-58.2899677801124,
175.152596646605));
#47356=CARTESIAN_POINT('Ctrl Pts',(-85.9788421953099,-58.0828594024298,
174.534734180363));
#47357=CARTESIAN_POINT('Ctrl Pts',(-85.3871739388038,-58.2164300361061,
174.285419051878));
#47358=CARTESIAN_POINT('Ctrl Pts',(-86.0316755766042,-58.2203681016103,
175.180268026546));
#47359=CARTESIAN_POINT('Ctrl Pts',(-85.9462564441589,-57.9984882972759,
174.507170494432));
#47360=CARTESIAN_POINT('Ctrl Pts',(-85.2902011513818,-58.1706704423479,
174.285427777742));
#47361=CARTESIAN_POINT('Ctrl Pts',(-85.977386954683,-58.0795219938815,175.228167698491));
#47362=CARTESIAN_POINT('Ctrl Pts',(-85.8947331753262,-57.8653677607553,
174.446387500193));
#47363=CARTESIAN_POINT('Ctrl Pts',(-85.1350481968355,-58.11121024114,174.285445515549));
#47364=CARTESIAN_POINT('Ctrl Pts',(-85.949907694424,-58.0083634795072,175.248785112141));
#47365=CARTESIAN_POINT('Ctrl Pts',(-85.876435258962,-57.8182885447687,174.413140806164));
#47366=CARTESIAN_POINT('Ctrl Pts',(-85.0745252827981,-58.0978603796713,
174.285454331853));
#47367=CARTESIAN_POINT('Ctrl Pts',(-85.8745820102155,-57.8136954178983,
175.287114544409));
#47368=CARTESIAN_POINT('Ctrl Pts',(-85.8392537097024,-57.7227428207907,
174.32347969837));
#47369=CARTESIAN_POINT('Ctrl Pts',(-84.94126861619,-58.0748566531053,174.285476383955));
#47370=CARTESIAN_POINT('Ctrl Pts',(-85.8255622901349,-57.6874168715231,
175.29370201928));
#47371=CARTESIAN_POINT('Ctrl Pts',(-85.8314829454387,-57.702975857336,174.269971978808));
#47372=CARTESIAN_POINT('Ctrl Pts',(-84.8879909211494,-58.0755909926104,
174.285488480751));
#47373=CARTESIAN_POINT('Ctrl Pts',(-85.7747409433632,-57.5569792392174,
175.273508736808));
#47374=CARTESIAN_POINT('Ctrl Pts',(-85.8299220105362,-57.6985809329344,
174.228384991744));
#47375=CARTESIAN_POINT('Ctrl Pts',(-84.843264995634,-58.0736839758418,174.285497501802));
#47376=CARTESIAN_POINT('Origin',(-84.9035795890703,-58.0758081979709,175.285485069079));
#47377=CARTESIAN_POINT('Ctrl Pts',(-76.3543296174317,-40.0523497550927,
174.285485069079));
#47378=CARTESIAN_POINT('Ctrl Pts',(-77.2166317829811,-39.5459556642022,
174.285485069079));
#47379=CARTESIAN_POINT('Ctrl Pts',(-77.2166317829811,-39.5459556642022,
175.285485069079));
#47380=CARTESIAN_POINT('Ctrl Pts',(-76.5654763654227,-40.4118964032641,
174.285485069079));
#47381=CARTESIAN_POINT('Ctrl Pts',(-77.4272707898731,-39.9046377164337,
174.285485068964));
#47382=CARTESIAN_POINT('Ctrl Pts',(-77.4272707898438,-39.9046377164501,
175.285485068987));
#47383=CARTESIAN_POINT('Ctrl Pts',(-76.7761244754699,-40.7715864905485,
174.285485069079));
#47384=CARTESIAN_POINT('Ctrl Pts',(-77.6413892786381,-40.270249793139,174.285485069108));
#47385=CARTESIAN_POINT('Ctrl Pts',(-77.6413892786757,-40.2702497931179,
175.285485069103));
#47386=CARTESIAN_POINT('Ctrl Pts',(-77.1904617586327,-41.4944329040647,
174.285485069079));
#47387=CARTESIAN_POINT('Ctrl Pts',(-78.060355852547,-41.0011723956288,174.285485069051));
#47388=CARTESIAN_POINT('Ctrl Pts',(-78.0603558525094,-41.00117239565,175.285485069056));
#47389=CARTESIAN_POINT('Ctrl Pts',(-77.3950072327115,-41.8571257984251,
174.285485069079));
#47390=CARTESIAN_POINT('Ctrl Pts',(-78.2671250050659,-41.3678098897366,
174.285485069079));
#47391=CARTESIAN_POINT('Ctrl Pts',(-78.2671250050945,-41.3678098897207,
175.285485069079));
#47392=CARTESIAN_POINT('Ctrl Pts',(-78.0011966023962,-42.9488090664736,
174.285485069079));
#47393=CARTESIAN_POINT('Ctrl Pts',(-78.8797401691552,-42.4710653373489,
174.285485069079));
#47394=CARTESIAN_POINT('Ctrl Pts',(-78.879740169098,-42.4710653373806,175.285485069079));
#47395=CARTESIAN_POINT('Ctrl Pts',(-78.3954041226997,-43.68139885703,174.28548506908));
#47396=CARTESIAN_POINT('Ctrl Pts',(-79.277905510414,-43.2110215506354,174.28548506908));
#47397=CARTESIAN_POINT('Ctrl Pts',(-79.2779055104667,-43.2110215506049,
175.285485069079));
#47398=CARTESIAN_POINT('Ctrl Pts',(-79.5512148812292,-45.8921459028217,
174.28548506908));
#47399=CARTESIAN_POINT('Ctrl Pts',(-80.4447931525601,-45.4429556182101,
174.28548506908));
#47400=CARTESIAN_POINT('Ctrl Pts',(-80.4447931524548,-45.4429556182708,
175.285485069079));
#47401=CARTESIAN_POINT('Ctrl Pts',(-80.2861211753126,-47.3832252372925,
174.285485069079));
#47402=CARTESIAN_POINT('Ctrl Pts',(-81.1860310864378,-46.9469487861698,
174.285485069149));
#47403=CARTESIAN_POINT('Ctrl Pts',(-81.1860310865154,-46.9469487861327,
175.285485069126));
#47404=CARTESIAN_POINT('Ctrl Pts',(-82.4022289101332,-51.8993535532297,
174.285485069079));
#47405=CARTESIAN_POINT('Ctrl Pts',(-83.318977139008,-51.4990128921297,174.285485068941));
#47406=CARTESIAN_POINT('Ctrl Pts',(-83.3189771388528,-51.4990128922039,
175.285485068987));
#47407=CARTESIAN_POINT('Ctrl Pts',(-83.6957353882012,-54.9669011015501,
174.285485069079));
#47408=CARTESIAN_POINT('Ctrl Pts',(-84.6208766886056,-54.5867888507445,
174.285485068894));
#47409=CARTESIAN_POINT('Ctrl Pts',(-84.6208766883517,-54.5867888508327,
175.285485068894));
#47410=CARTESIAN_POINT('Ctrl Pts',(-84.9035795890702,-58.0758081979708,
174.285485069079));
#47411=CARTESIAN_POINT('Ctrl Pts',(-85.8357032382102,-57.7136680279897,
174.285485069079));
#47412=CARTESIAN_POINT('Ctrl Pts',(-85.8357032382102,-57.7136680279897,
175.285485069079));
#47413=CARTESIAN_POINT('',(0.,0.,0.));
#47414=CARTESIAN_POINT('Origin',(-70.1438101352762,-11.0431453779951,174.735485069079));
#47415=CARTESIAN_POINT('',(-70.7560295400602,-9.13915288840755,174.735485069079));
#47416=CARTESIAN_POINT('Origin',(-70.1438101352762,-11.0431453779951,174.735485069079));
#47417=CARTESIAN_POINT('',(-70.8325569656582,-8.9011538272091,174.485485069079));
#47418=CARTESIAN_POINT('Origin',(-70.8325569656582,-8.9011538272091,174.735485069079));
#47419=CARTESIAN_POINT('Origin',(-70.1438101352762,-11.0431453779951,174.485485069079));
#47420=CARTESIAN_POINT('Origin',(-53.6138862061095,-62.4509425968603,174.735485069079));
#47421=CARTESIAN_POINT('',(-57.8026696832023,-63.797825287385,174.735485069079));
#47422=CARTESIAN_POINT('',(-49.4251027290168,-61.1040599063356,174.735485069079));
#47423=CARTESIAN_POINT('Origin',(-53.6138862061095,-62.4509425968603,174.735485069079));
#47424=CARTESIAN_POINT('',(-57.5646706220038,-63.721297861787,174.485485069079));
#47425=CARTESIAN_POINT('Origin',(-57.5646706220038,-63.721297861787,174.735485069079));
#47426=CARTESIAN_POINT('',(-49.6631017902153,-61.1805873319336,174.485485069079));
#47427=CARTESIAN_POINT('Origin',(-53.6138862061095,-62.4509425968603,174.485485069079));
#47428=CARTESIAN_POINT('Origin',(-49.6631017902153,-61.1805873319336,174.735485069079));
#47429=CARTESIAN_POINT('Origin',(-53.6138862061095,-62.4509425968603,174.735485069079));
#47430=CARTESIAN_POINT('',(-54.2261056108935,-60.5469501072727,174.735485069079));
#47431=CARTESIAN_POINT('Origin',(-53.6138862061095,-62.4509425968603,174.735485069079));
#47432=CARTESIAN_POINT('',(-54.3026330364915,-60.3089510460743,174.485485069079));
#47433=CARTESIAN_POINT('Origin',(-54.3026330364915,-60.3089510460743,174.735485069079));
#47434=CARTESIAN_POINT('Origin',(-53.6138862061095,-62.4509425968603,174.485485069079));
#47435=CARTESIAN_POINT('Origin',(-53.6138862061095,-62.4509425968603,177.235485069079));
#47436=CARTESIAN_POINT('',(-57.5646706220038,-63.721297861787,177.485485069079));
#47437=CARTESIAN_POINT('',(-49.6631017902153,-61.1805873319336,177.485485069079));
#47438=CARTESIAN_POINT('Origin',(-53.6138862061095,-62.4509425968603,177.485485069079));
#47439=CARTESIAN_POINT('',(-57.8026696832023,-63.797825287385,177.235485069079));
#47440=CARTESIAN_POINT('Origin',(-57.5646706220038,-63.721297861787,177.235485069079));
#47441=CARTESIAN_POINT('',(-49.4251027290168,-61.1040599063356,177.235485069079));
#47442=CARTESIAN_POINT('Origin',(-53.6138862061095,-62.4509425968603,177.235485069079));
#47443=CARTESIAN_POINT('Origin',(-49.6631017902153,-61.1805873319336,177.235485069079));
#47444=CARTESIAN_POINT('Origin',(-70.1438101352762,-11.0431453779951,177.235485069079));
#47445=CARTESIAN_POINT('',(-70.8325569656582,-8.9011538272091,177.485485069079));
#47446=CARTESIAN_POINT('Origin',(-70.1438101352762,-11.0431453779951,177.485485069079));
#47447=CARTESIAN_POINT('',(-70.7560295400602,-9.13915288840755,177.235485069079));
#47448=CARTESIAN_POINT('Origin',(-70.8325569656582,-8.9011538272091,177.235485069079));
#47449=CARTESIAN_POINT('Origin',(-70.1438101352762,-11.0431453779951,177.235485069079));
#47450=CARTESIAN_POINT('Origin',(-53.6138862061095,-62.4509425968603,177.235485069079));
#47451=CARTESIAN_POINT('',(-54.3026330364915,-60.3089510460743,177.485485069079));
#47452=CARTESIAN_POINT('Origin',(-53.6138862061095,-62.4509425968603,177.485485069079));
#47453=CARTESIAN_POINT('',(-54.2261056108935,-60.5469501072727,177.235485069079));
#47454=CARTESIAN_POINT('Origin',(-54.3026330364915,-60.3089510460743,177.235485069079));
#47455=CARTESIAN_POINT('Origin',(-53.6138862061095,-62.4509425968603,177.235485069079));
#47456=CARTESIAN_POINT('Origin',(-53.6138862061095,-62.4509425968603,177.485485069079));
#47457=CARTESIAN_POINT('',(-54.2261056108935,-60.5469501072727,177.485485069079));
#47458=CARTESIAN_POINT('Origin',(-70.1438101352762,-11.0431453779951,177.485485069079));
#47459=CARTESIAN_POINT('',(-70.7560295400602,-9.13915288840755,177.485485069079));
#47460=CARTESIAN_POINT('Origin',(-53.6138862061095,-62.4509425968603,177.485485069079));
#47461=CARTESIAN_POINT('',(-57.8026696832023,-63.797825287385,177.485485069079));
#47462=CARTESIAN_POINT('',(-49.4251027290168,-61.1040599063356,177.485485069079));
#47463=CARTESIAN_POINT('Origin',(-53.6138862061095,-62.4509425968603,177.485485069079));
#47464=CARTESIAN_POINT('',(-73.7816789787941,-42.3755520783705,177.485485069079));
#47465=CARTESIAN_POINT('',(-68.8282104295052,-49.9715016156815,177.485485069079));
#47466=CARTESIAN_POINT('Origin',(-64.0748867591837,-41.4586634235648,177.485485069079));
#47467=CARTESIAN_POINT('Origin',(-80.6505795582534,-71.1444581447924,177.485485069079));
#47468=CARTESIAN_POINT('',(-54.8465294930114,-45.0602106510818,177.485485069079));
#47469=CARTESIAN_POINT('',(-49.6631017902153,-61.1805873319336,177.485485069079));
#47470=CARTESIAN_POINT('',(-61.0095980165858,-25.8931667939203,177.485485069079));
#47471=CARTESIAN_POINT('Origin',(-41.2010060476238,-30.0981857245761,177.485485069079));
#47472=CARTESIAN_POINT('',(-66.193025719382,-9.77279011306845,177.485485069079));
#47473=CARTESIAN_POINT('',(-49.6631017902153,-61.1805873319336,177.485485069079));
#47474=CARTESIAN_POINT('',(-74.082992404925,-12.3490332163964,177.485485069079));
#47475=CARTESIAN_POINT('Origin',(-70.1438101352762,-11.0431453779951,177.485485069079));
#47476=CARTESIAN_POINT('',(-73.5782138375345,-62.6512828356565,177.485485069079));
#47477=CARTESIAN_POINT('Origin',(-53.6138862061095,-62.4509425968603,174.485485069079));
#47478=CARTESIAN_POINT('',(-61.0095980165858,-25.8931667939203,174.485485069079));
#47479=CARTESIAN_POINT('',(-54.8465294930114,-45.0602106510818,174.485485069079));
#47480=CARTESIAN_POINT('Origin',(-41.2010060476238,-30.0981857245761,174.485485069079));
#47481=CARTESIAN_POINT('',(-49.6631017902153,-61.1805873319336,174.485485069079));
#47482=CARTESIAN_POINT('',(-68.8282104295052,-49.9715016156815,174.485485069079));
#47483=CARTESIAN_POINT('Origin',(-80.6505795582534,-71.1444581447924,174.485485069079));
#47484=CARTESIAN_POINT('',(-73.7816789787941,-42.3755520783705,174.485485069079));
#47485=CARTESIAN_POINT('Origin',(-64.0748867591837,-41.4586634235648,174.485485069079));
#47486=CARTESIAN_POINT('',(-74.082992404925,-12.3490332163964,174.485485069079));
#47487=CARTESIAN_POINT('',(-74.0826061988467,-12.3875194672263,174.485485069079));
#47488=CARTESIAN_POINT('',(-66.193025719382,-9.77279011306845,174.485485069079));
#47489=CARTESIAN_POINT('Origin',(-70.1438101352762,-11.0431453779951,174.485485069079));
#47490=CARTESIAN_POINT('',(-60.9891607787184,-25.956726274563,174.485485069079));
#47491=CARTESIAN_POINT('Origin',(-49.4251027290168,-61.1040599063356,177.485485069079));
#47492=CARTESIAN_POINT('',(-54.6289676696804,-44.920123744841,177.235485069079));
#47493=CARTESIAN_POINT('',(-54.6289676696804,-44.920123744841,174.735485069079));
#47494=CARTESIAN_POINT('',(-54.6289676696804,-44.920123744841,177.485485069079));
#47495=CARTESIAN_POINT('',(-49.4251027290168,-61.1040599063356,177.235485069079));
#47496=CARTESIAN_POINT('',(-54.6289676696804,-44.920123744841,174.735485069079));
#47497=CARTESIAN_POINT('Origin',(-41.2010060476238,-30.0981857245761,177.485485069079));
#47498=CARTESIAN_POINT('',(-60.7511617175199,-25.8801988489651,177.235485069079));
#47499=CARTESIAN_POINT('',(-60.7511617175199,-25.8801988489651,174.735485069079));
#47500=CARTESIAN_POINT('',(-60.7511617175199,-25.8801988489651,177.485485069079));
#47501=CARTESIAN_POINT('Origin',(-41.2010060476238,-30.0981857245761,177.235485069079));
#47502=CARTESIAN_POINT('Origin',(-41.2010060476238,-30.0981857245761,174.735485069079));
#47503=CARTESIAN_POINT('Origin',(-60.7511617175199,-25.8801988489651,177.485485069079));
#47504=CARTESIAN_POINT('',(-65.9550266581835,-9.69626268747045,177.235485069079));
#47505=CARTESIAN_POINT('',(-65.9550266581835,-9.69626268747045,174.735485069079));
#47506=CARTESIAN_POINT('',(-65.9550266581835,-9.69626268747045,177.485485069079));
#47507=CARTESIAN_POINT('',(-60.7511617175199,-25.8801988489651,177.235485069079));
#47508=CARTESIAN_POINT('',(-65.9550266581835,-9.69626268747045,174.735485069079));
#47509=CARTESIAN_POINT('Origin',(-70.1438101352762,-11.0431453779951,177.485485069079));
#47510=CARTESIAN_POINT('',(-74.3325936123689,-12.3900280685198,177.235485069079));
#47511=CARTESIAN_POINT('',(-74.3325936123689,-12.3900280685198,174.735485069079));
#47512=CARTESIAN_POINT('',(-74.3325936123689,-12.3900280685198,177.485485069079));
#47513=CARTESIAN_POINT('Origin',(-70.1438101352762,-11.0431453779951,177.235485069079));
#47514=CARTESIAN_POINT('Origin',(-70.1438101352762,-11.0431453779951,174.735485069079));
#47515=CARTESIAN_POINT('Origin',(-74.0315614571427,-42.3885176911912,177.485485069079));
#47516=CARTESIAN_POINT('',(-74.0315614571427,-42.3885176911912,177.235485069079));
#47517=CARTESIAN_POINT('',(-74.0315614571427,-42.3885176911912,174.735485069079));
#47518=CARTESIAN_POINT('',(-74.0315614571427,-42.3885176911912,177.485485069079));
#47519=CARTESIAN_POINT('',(-74.0315614571427,-42.3885176911912,177.235485069079));
#47520=CARTESIAN_POINT('',(-74.0315614571427,-42.3885176911912,174.735485069079));
#47521=CARTESIAN_POINT('Origin',(-64.0748867591837,-41.4586634235648,177.485485069079));
#47522=CARTESIAN_POINT('',(-68.950090523616,-50.1897795180435,177.235485069079));
#47523=CARTESIAN_POINT('',(-68.950090523616,-50.1897795180435,174.735485069079));
#47524=CARTESIAN_POINT('',(-68.950090523616,-50.1897795180435,177.485485069079));
#47525=CARTESIAN_POINT('Origin',(-64.0748867591837,-41.4586634235648,177.235485069079));
#47526=CARTESIAN_POINT('Origin',(-64.0748867591837,-41.4586634235648,174.735485069079));
#47527=CARTESIAN_POINT('Origin',(-80.6505795582534,-71.1444581447924,177.485485069079));
#47528=CARTESIAN_POINT('Origin',(-80.6505795582534,-71.1444581447924,177.235485069079));
#47529=CARTESIAN_POINT('Origin',(-80.6505795582534,-71.1444581447924,174.735485069079));
#47530=CARTESIAN_POINT('Origin',(-49.6631017902153,-61.1805873319336,177.235485069079));
#47531=CARTESIAN_POINT('Ctrl Pts',(-60.7511617175199,-25.8801988489651,
177.235485069079));
#47532=CARTESIAN_POINT('Ctrl Pts',(-60.7511617175199,-25.8801988489651,
177.236209624631));
#47533=CARTESIAN_POINT('Ctrl Pts',(-60.7511649745547,-25.8801990096816,
177.236934363604));
#47534=CARTESIAN_POINT('Ctrl Pts',(-60.751454897117,-25.8802133157759,177.26917313906));
#47535=CARTESIAN_POINT('Ctrl Pts',(-60.7578951724417,-25.8805307741899,
177.300270548243));
#47536=CARTESIAN_POINT('Ctrl Pts',(-60.782469053451,-25.8817463747679,177.358946342665));
#47537=CARTESIAN_POINT('Ctrl Pts',(-60.8005420012037,-25.8826417492884,
177.385802945446));
#47538=CARTESIAN_POINT('Ctrl Pts',(-60.8465753700736,-25.8849347071446,
177.432198391808));
#47539=CARTESIAN_POINT('Ctrl Pts',(-60.8744154272029,-25.88632691736,177.450986825543));
#47540=CARTESIAN_POINT('Ctrl Pts',(-60.937307891463,-25.8894927969754,177.477924595734));
#47541=CARTESIAN_POINT('Ctrl Pts',(-60.9721283554826,-25.8912560982159,
177.48517070955));
#47542=CARTESIAN_POINT('Ctrl Pts',(-61.0080570542599,-25.8930881990745,
177.48548173422));
#47543=CARTESIAN_POINT('Ctrl Pts',(-61.0088275341472,-25.8931274935949,
177.485485069079));
#47544=CARTESIAN_POINT('Ctrl Pts',(-61.0095980165858,-25.8931667939203,
177.485485069079));
#47545=CARTESIAN_POINT('Origin',(-66.193025719382,-9.77279011306845,177.235485069079));
#47546=CARTESIAN_POINT('Origin',(-70.1438101352762,-11.0431453779951,177.235485069079));
#47547=CARTESIAN_POINT('Ctrl Pts',(-74.0829924049255,-12.3490332163965,
177.485485069079));
#47548=CARTESIAN_POINT('Ctrl Pts',(-74.0837490876437,-12.3491592710996,
177.485485069079));
#47549=CARTESIAN_POINT('Ctrl Pts',(-74.0845057695073,-12.3492853090228,
177.485481622518));
#47550=CARTESIAN_POINT('Ctrl Pts',(-74.1187223288458,-12.3549838920991,
177.485169912202));
#47551=CARTESIAN_POINT('Ctrl Pts',(-74.1518167082703,-12.3604619039869,
177.478128415433));
#47552=CARTESIAN_POINT('Ctrl Pts',(-74.2122917073814,-12.3704217394355,
177.451777056831));
#47553=CARTESIAN_POINT('Ctrl Pts',(-74.2392789041521,-12.3748411885359,
177.433118690759));
#47554=CARTESIAN_POINT('Ctrl Pts',(-74.2843931866928,-12.3822052137679,
177.386633798983));
#47555=CARTESIAN_POINT('Ctrl Pts',(-74.3021911232899,-12.3850970696903,
177.359357331601));
#47556=CARTESIAN_POINT('Ctrl Pts',(-74.3263794660467,-12.3890225555062,
177.29957394136));
#47557=CARTESIAN_POINT('Ctrl Pts',(-74.332593612369,-12.3900280685198,177.267693581309));
#47558=CARTESIAN_POINT('Ctrl Pts',(-74.3325936123689,-12.3900280685198,
177.235485069079));
#47559=CARTESIAN_POINT('Origin',(-41.2010060476238,-30.0981857245761,177.235485069079));
#47560=CARTESIAN_POINT('Ctrl Pts',(-54.6289676696804,-44.920123744841,177.235485069079));
#47561=CARTESIAN_POINT('Ctrl Pts',(-54.6289676696804,-44.9201237448411,
177.266555445342));
#47562=CARTESIAN_POINT('Ctrl Pts',(-54.6340056002196,-44.9233739545679,
177.297288535147));
#47563=CARTESIAN_POINT('Ctrl Pts',(-54.6540860524352,-44.9363240585933,
177.356614103802));
#47564=CARTESIAN_POINT('Ctrl Pts',(-54.6694432684634,-44.9462265480297,
177.384289371841));
#47565=CARTESIAN_POINT('Ctrl Pts',(-54.7089373275903,-44.9716773681615,
177.432038662699));
#47566=CARTESIAN_POINT('Ctrl Pts',(-54.7329702784393,-44.9871579385665,
177.451300874194));
#47567=CARTESIAN_POINT('Ctrl Pts',(-54.7863463486712,-45.0215139393215,
177.478097428015));
#47568=CARTESIAN_POINT('Ctrl Pts',(-54.8153235492639,-45.0401531604041,
177.485174360859));
#47569=CARTESIAN_POINT('Ctrl Pts',(-54.845231509254,-45.0593763968009,177.48548173422));
#47570=CARTESIAN_POINT('Ctrl Pts',(-54.8458804984045,-45.0597935255564,
177.485485069079));
#47571=CARTESIAN_POINT('Ctrl Pts',(-54.8465294930115,-45.0602106510817,
177.485485069079));
#47572=CARTESIAN_POINT('Origin',(-73.5782138375345,-62.6512828356565,177.235485069079));
#47573=CARTESIAN_POINT('Ctrl Pts',(-73.7816789787941,-42.3755520783705,
177.485485069079));
#47574=CARTESIAN_POINT('Ctrl Pts',(-73.7981057833924,-42.3764086084212,
177.485485069079));
#47575=CARTESIAN_POINT('Ctrl Pts',(-73.8145162527323,-42.3772651018765,
177.483859254794));
#47576=CARTESIAN_POINT('Ctrl Pts',(-73.8305939553847,-42.3781032802876,
177.48064835975));
#47577=CARTESIAN_POINT('Ctrl Pts',(-73.8459401365431,-42.3789033223096,
177.47758355764));
#47578=CARTESIAN_POINT('Ctrl Pts',(-73.8609825651133,-42.379686630563,177.473075252585));
#47579=CARTESIAN_POINT('Ctrl Pts',(-73.8754594678907,-42.38043896216,177.467210817261));
#47580=CARTESIAN_POINT('Ctrl Pts',(-73.889953215135,-42.3811921691254,177.461339558427));
#47581=CARTESIAN_POINT('Ctrl Pts',(-73.9038795299571,-42.3819142779909,
177.45410931481));
#47582=CARTESIAN_POINT('Ctrl Pts',(-73.9169982217908,-42.3825934214874,
177.445654854873));
#47583=CARTESIAN_POINT('Ctrl Pts',(-73.9301452183313,-42.3832740302944,
177.43718215371));
#47584=CARTESIAN_POINT('Ctrl Pts',(-73.9424805770332,-42.3839114468893,
177.427480351751));
#47585=CARTESIAN_POINT('Ctrl Pts',(-73.9537935453965,-42.3844968441549,
177.416727042628));
#47586=CARTESIAN_POINT('Ctrl Pts',(-73.9553553902192,-42.3845776628807,
177.415242463193));
#47587=CARTESIAN_POINT('Ctrl Pts',(-73.9568978035099,-42.3846574955071,
177.4137379014));
#47588=CARTESIAN_POINT('Ctrl Pts',(-73.9584202852857,-42.3847363240965,
177.412213879973));
#47589=CARTESIAN_POINT('Ctrl Pts',(-73.9702299481194,-42.3853477856444,
177.400392274298));
#47590=CARTESIAN_POINT('Ctrl Pts',(-73.9808446692677,-42.3858989380282,
177.387389529667));
#47591=CARTESIAN_POINT('Ctrl Pts',(-73.9900643178673,-42.3863772577204,
177.373450709894));
#47592=CARTESIAN_POINT('Ctrl Pts',(-73.9992576720282,-42.3868542132448,
177.359551643636));
#47593=CARTESIAN_POINT('Ctrl Pts',(-74.0070636659419,-42.3872587376246,
177.344722141989));
#47594=CARTESIAN_POINT('Ctrl Pts',(-74.0133253949135,-42.3875821461516,
177.329235611602));
#47595=CARTESIAN_POINT('Ctrl Pts',(-74.0195252880819,-42.3879023609559,
177.313902013744));
#47596=CARTESIAN_POINT('Ctrl Pts',(-74.0242110678826,-42.3881430426806,
177.297924635572));
#47597=CARTESIAN_POINT('Ctrl Pts',(-74.0272743187926,-42.3882996010354,
177.281593926282));
#47598=CARTESIAN_POINT('Ctrl Pts',(-74.0301158269513,-42.3884448264367,
177.266445365145));
#47599=CARTESIAN_POINT('Ctrl Pts',(-74.0315614571427,-42.3885176911912,
177.250993231542));
#47600=CARTESIAN_POINT('Ctrl Pts',(-74.0315614571427,-42.3885176911912,
177.235485069079));
#47601=CARTESIAN_POINT('Origin',(-49.6631017902153,-61.1805873319336,177.235485069079));
#47602=CARTESIAN_POINT('Origin',(-64.0748867591837,-41.4586634235648,177.235485069079));
#47603=CARTESIAN_POINT('Origin',(-68.8282104295052,-49.9715016156815,177.235485069079));
#47604=CARTESIAN_POINT('Origin',(-80.6505795582534,-71.1444581447924,177.235485069079));
#47605=CARTESIAN_POINT('Origin',(-73.7815740436205,-42.3860090898976,174.735485069079));
#47606=CARTESIAN_POINT('Ctrl Pts',(-74.0829924049252,-12.3490332163965,
174.485485069079));
#47607=CARTESIAN_POINT('Ctrl Pts',(-74.0837490876434,-12.3491592710996,
174.485485069079));
#47608=CARTESIAN_POINT('Ctrl Pts',(-74.0845057695072,-12.3492853090228,
174.48548851564));
#47609=CARTESIAN_POINT('Ctrl Pts',(-74.1187223288457,-12.3549838920989,
174.485800225956));
#47610=CARTESIAN_POINT('Ctrl Pts',(-74.1518167082703,-12.3604619039867,
174.492841722725));
#47611=CARTESIAN_POINT('Ctrl Pts',(-74.2122917073815,-12.3704217394354,
174.519193081327));
#47612=CARTESIAN_POINT('Ctrl Pts',(-74.2392789041521,-12.374841188536,174.5378514474));
#47613=CARTESIAN_POINT('Ctrl Pts',(-74.2843931866929,-12.3822052137679,
174.584336339176));
#47614=CARTESIAN_POINT('Ctrl Pts',(-74.3021911232899,-12.3850970696904,
174.611612806557));
#47615=CARTESIAN_POINT('Ctrl Pts',(-74.3263794660467,-12.3890225555062,
174.671396196798));
#47616=CARTESIAN_POINT('Ctrl Pts',(-74.3325936123689,-12.3900280685199,
174.70327655685));
#47617=CARTESIAN_POINT('Ctrl Pts',(-74.3325936123689,-12.3900280685199,
174.735485069079));
#47618=CARTESIAN_POINT('Ctrl Pts',(-74.0315614571427,-42.3885176911912,
174.735485069079));
#47619=CARTESIAN_POINT('Ctrl Pts',(-74.0315614571427,-42.3885176911912,
174.718765393872));
#47620=CARTESIAN_POINT('Ctrl Pts',(-74.0298805568919,-42.3884329506508,
174.702110999624));
#47621=CARTESIAN_POINT('Ctrl Pts',(-74.026582879632,-42.3882642507143,174.685831471344));
#47622=CARTESIAN_POINT('Ctrl Pts',(-74.02326312362,-42.3880944212906,174.669442947658));
#47623=CARTESIAN_POINT('Ctrl Pts',(-74.0183051173532,-42.3878395216834,
174.653434683319));
#47624=CARTESIAN_POINT('Ctrl Pts',(-74.0118230397663,-42.3875045410618,
174.638101343067));
#47625=CARTESIAN_POINT('Ctrl Pts',(-74.0053026648678,-42.3871675813129,
174.62267741061));
#47626=CARTESIAN_POINT('Ctrl Pts',(-73.9972403916431,-42.3867496058168,
174.607936732203));
#47627=CARTESIAN_POINT('Ctrl Pts',(-73.9877979397281,-42.3862596813854,
174.594152694406));
#47628=CARTESIAN_POINT('Ctrl Pts',(-73.9791080850659,-42.3858088056868,
174.581467293813));
#47629=CARTESIAN_POINT('Ctrl Pts',(-73.9692499366581,-42.3852970451061,
174.569592003359));
#47630=CARTESIAN_POINT('Ctrl Pts',(-73.9583807640474,-42.3847342778285,
174.558716705829));
#47631=CARTESIAN_POINT('Ctrl Pts',(-73.9481748997668,-42.384205854308,174.548505090413));
#47632=CARTESIAN_POINT('Ctrl Pts',(-73.937051290793,-42.3836314002962,174.539151069091));
#47633=CARTESIAN_POINT('Ctrl Pts',(-73.9251817152964,-42.3830174841342,
174.530820820265));
#47634=CARTESIAN_POINT('Ctrl Pts',(-73.91332102571,-42.3824040275676,174.522496807706));
#47635=CARTESIAN_POINT('Ctrl Pts',(-73.9007161293092,-42.3817512215404,
174.515195584145));
#47636=CARTESIAN_POINT('Ctrl Pts',(-73.8875713433795,-42.3810688619176,
174.509042800644));
#47637=CARTESIAN_POINT('Ctrl Pts',(-73.8744327327308,-42.3803868228602,
174.502892907656));
#47638=CARTESIAN_POINT('Ctrl Pts',(-73.8607555029461,-42.3796753245276,
174.497890739208));
#47639=CARTESIAN_POINT('Ctrl Pts',(-73.8467659990825,-42.3789464847267,
174.494114765878));
#47640=CARTESIAN_POINT('Ctrl Pts',(-73.8327506058318,-42.3782162961134,
174.490331804621));
#47641=CARTESIAN_POINT('Ctrl Pts',(-73.8184226118037,-42.3774687767553,
174.487779751606));
#47642=CARTESIAN_POINT('Ctrl Pts',(-73.8040200140351,-42.3767173904492,
174.486486267331));
#47643=CARTESIAN_POINT('Ctrl Pts',(-73.796581894898,-42.3763293423378,174.485818256581));
#47644=CARTESIAN_POINT('Ctrl Pts',(-73.7891239696738,-42.375940276719,174.485485069079));
#47645=CARTESIAN_POINT('Ctrl Pts',(-73.7816789787941,-42.3755520783705,
174.485485069079));
#47646=CARTESIAN_POINT('Origin',(-64.0748867591837,-41.4586634235648,174.735485069079));
#47647=CARTESIAN_POINT('Origin',(-68.8282104295052,-49.9715016156815,174.735485069079));
#47648=CARTESIAN_POINT('Origin',(-70.1438101352762,-11.0431453779951,174.735485069079));
#47649=CARTESIAN_POINT('Origin',(-66.193025719382,-9.77279011306845,174.735485069079));
#47650=CARTESIAN_POINT('Origin',(-80.6505795582534,-71.1444581447924,174.735485069079));
#47651=CARTESIAN_POINT('Origin',(-60.9891607787184,-25.956726274563,174.735485069079));
#47652=CARTESIAN_POINT('Ctrl Pts',(-61.0095980165858,-25.8931667939203,
174.485485069079));
#47653=CARTESIAN_POINT('Ctrl Pts',(-61.0088275341472,-25.8931274935949,
174.485485069079));
#47654=CARTESIAN_POINT('Ctrl Pts',(-61.0080570542599,-25.8930881990744,
174.485488403939));
#47655=CARTESIAN_POINT('Ctrl Pts',(-60.9725501444756,-25.8912776063701,
174.4857957773));
#47656=CARTESIAN_POINT('Ctrl Pts',(-60.9381399458952,-25.8895349215335,
174.492872710144));
#47657=CARTESIAN_POINT('Ctrl Pts',(-60.8747431598305,-25.8863431856417,
174.519669263965));
#47658=CARTESIAN_POINT('Ctrl Pts',(-60.8461915856332,-25.8849154610819,
174.53893147546));
#47659=CARTESIAN_POINT('Ctrl Pts',(-60.7992654458767,-25.8825782920219,
174.586680766318));
#47660=CARTESIAN_POINT('Ctrl Pts',(-60.781014795274,-25.8816743375162,174.614356034357));
#47661=CARTESIAN_POINT('Ctrl Pts',(-60.7571498297398,-25.8804940089663,
174.673681603012));
#47662=CARTESIAN_POINT('Ctrl Pts',(-60.7511617175199,-25.8801988489651,
174.704414692817));
#47663=CARTESIAN_POINT('Ctrl Pts',(-60.7511617175199,-25.8801988489651,
174.735485069079));
#47664=CARTESIAN_POINT('Origin',(-41.2010060476238,-30.0981857245761,174.735485069079));
#47665=CARTESIAN_POINT('Ctrl Pts',(-54.8465294930115,-45.0602106510817,
174.485485069079));
#47666=CARTESIAN_POINT('Ctrl Pts',(-54.8458804984045,-45.0597935255564,
174.485485069079));
#47667=CARTESIAN_POINT('Ctrl Pts',(-54.845231509254,-45.0593763968009,174.485488403939));
#47668=CARTESIAN_POINT('Ctrl Pts',(-54.8153235492641,-45.0401531604042,
174.4857957773));
#47669=CARTESIAN_POINT('Ctrl Pts',(-54.7863463486712,-45.0215139393217,
174.492872710144));
#47670=CARTESIAN_POINT('Ctrl Pts',(-54.7329702784391,-44.9871579385665,
174.519669263965));
#47671=CARTESIAN_POINT('Ctrl Pts',(-54.7089373275902,-44.9716773681615,
174.538931475459));
#47672=CARTESIAN_POINT('Ctrl Pts',(-54.6694432684634,-44.9462265480297,
174.586680766317));
#47673=CARTESIAN_POINT('Ctrl Pts',(-54.6540860524352,-44.9363240585933,
174.614356034356));
#47674=CARTESIAN_POINT('Ctrl Pts',(-54.6340056002196,-44.9233739545679,
174.673681603011));
#47675=CARTESIAN_POINT('Ctrl Pts',(-54.6289676696804,-44.920123744841,174.704414692817));
#47676=CARTESIAN_POINT('Ctrl Pts',(-54.6289676696804,-44.920123744841,174.735485069079));
#47677=CARTESIAN_POINT('Origin',(-49.6631017902153,-61.1805873319336,174.735485069079));
#47678=CARTESIAN_POINT('',(0.,0.,0.));
#47679=CARTESIAN_POINT('',(0.,0.,0.));
#47680=CARTESIAN_POINT('',(0.,0.,0.));
#47681=CARTESIAN_POINT('',(0.,0.,0.));
#47682=CARTESIAN_POINT('',(0.,0.,0.));
#47683=CARTESIAN_POINT('',(0.,0.,0.));
#47684=CARTESIAN_POINT('',(0.,0.,0.));
#47685=CARTESIAN_POINT('',(0.,0.,0.));
#47686=CARTESIAN_POINT('',(0.,0.,0.));
#47687=CARTESIAN_POINT('',(0.,0.,0.));
#47688=CARTESIAN_POINT('',(0.,0.,0.));
#47689=CARTESIAN_POINT('',(0.,0.,0.));
#47690=UNCERTAINTY_MEASURE_WITH_UNIT(LENGTH_MEASURE(0.01),#47718,
'DISTANCE_ACCURACY_VALUE',
'Maximum model space distance between geometric entities at asserted c
onnectivities');
#47691=UNCERTAINTY_MEASURE_WITH_UNIT(LENGTH_MEASURE(0.01),#47718,
'DISTANCE_ACCURACY_VALUE',
'Maximum model space distance between geometric entities at asserted c
onnectivities');
#47692=UNCERTAINTY_MEASURE_WITH_UNIT(LENGTH_MEASURE(0.01),#47718,
'DISTANCE_ACCURACY_VALUE',
'Maximum model space distance between geometric entities at asserted c
onnectivities');
#47693=UNCERTAINTY_MEASURE_WITH_UNIT(LENGTH_MEASURE(0.01),#47718,
'DISTANCE_ACCURACY_VALUE',
'Maximum model space distance between geometric entities at asserted c
onnectivities');
#47694=UNCERTAINTY_MEASURE_WITH_UNIT(LENGTH_MEASURE(0.01),#47718,
'DISTANCE_ACCURACY_VALUE',
'Maximum model space distance between geometric entities at asserted c
onnectivities');
#47695=UNCERTAINTY_MEASURE_WITH_UNIT(LENGTH_MEASURE(0.01),#47718,
'DISTANCE_ACCURACY_VALUE',
'Maximum model space distance between geometric entities at asserted c
onnectivities');
#47696=UNCERTAINTY_MEASURE_WITH_UNIT(LENGTH_MEASURE(0.01),#47718,
'DISTANCE_ACCURACY_VALUE',
'Maximum model space distance between geometric entities at asserted c
onnectivities');
#47697=UNCERTAINTY_MEASURE_WITH_UNIT(LENGTH_MEASURE(0.01),#47718,
'DISTANCE_ACCURACY_VALUE',
'Maximum model space distance between geometric entities at asserted c
onnectivities');
#47698=UNCERTAINTY_MEASURE_WITH_UNIT(LENGTH_MEASURE(0.01),#47718,
'DISTANCE_ACCURACY_VALUE',
'Maximum model space distance between geometric entities at asserted c
onnectivities');
#47699=UNCERTAINTY_MEASURE_WITH_UNIT(LENGTH_MEASURE(0.01),#47718,
'DISTANCE_ACCURACY_VALUE',
'Maximum model space distance between geometric entities at asserted c
onnectivities');
#47700=UNCERTAINTY_MEASURE_WITH_UNIT(LENGTH_MEASURE(0.01),#47718,
'DISTANCE_ACCURACY_VALUE',
'Maximum model space distance between geometric entities at asserted c
onnectivities');
#47701=UNCERTAINTY_MEASURE_WITH_UNIT(LENGTH_MEASURE(0.01),#47718,
'DISTANCE_ACCURACY_VALUE',
'Maximum model space distance between geometric entities at asserted c
onnectivities');
#47702=UNCERTAINTY_MEASURE_WITH_UNIT(LENGTH_MEASURE(0.01),#47718,
'DISTANCE_ACCURACY_VALUE',
'Maximum model space distance between geometric entities at asserted c
onnectivities');
#47703=UNCERTAINTY_MEASURE_WITH_UNIT(LENGTH_MEASURE(0.01),#47718,
'DISTANCE_ACCURACY_VALUE',
'Maximum model space distance between geometric entities at asserted c
onnectivities');
#47704=(
GEOMETRIC_REPRESENTATION_CONTEXT(3)
GLOBAL_UNCERTAINTY_ASSIGNED_CONTEXT((#47690))
GLOBAL_UNIT_ASSIGNED_CONTEXT((#47718,#47720,#47721))
REPRESENTATION_CONTEXT('','3D')
);
#47705=(
GEOMETRIC_REPRESENTATION_CONTEXT(3)
GLOBAL_UNCERTAINTY_ASSIGNED_CONTEXT((#47691))
GLOBAL_UNIT_ASSIGNED_CONTEXT((#47718,#47720,#47721))
REPRESENTATION_CONTEXT('','3D')
);
#47706=(
GEOMETRIC_REPRESENTATION_CONTEXT(3)
GLOBAL_UNCERTAINTY_ASSIGNED_CONTEXT((#47692))
GLOBAL_UNIT_ASSIGNED_CONTEXT((#47718,#47720,#47721))
REPRESENTATION_CONTEXT('','3D')
);
#47707=(
GEOMETRIC_REPRESENTATION_CONTEXT(3)
GLOBAL_UNCERTAINTY_ASSIGNED_CONTEXT((#47693))
GLOBAL_UNIT_ASSIGNED_CONTEXT((#47718,#47720,#47721))
REPRESENTATION_CONTEXT('','3D')
);
#47708=(
GEOMETRIC_REPRESENTATION_CONTEXT(3)
GLOBAL_UNCERTAINTY_ASSIGNED_CONTEXT((#47694))
GLOBAL_UNIT_ASSIGNED_CONTEXT((#47718,#47720,#47721))
REPRESENTATION_CONTEXT('','3D')
);
#47709=(
GEOMETRIC_REPRESENTATION_CONTEXT(3)
GLOBAL_UNCERTAINTY_ASSIGNED_CONTEXT((#47695))
GLOBAL_UNIT_ASSIGNED_CONTEXT((#47718,#47720,#47721))
REPRESENTATION_CONTEXT('','3D')
);
#47710=(
GEOMETRIC_REPRESENTATION_CONTEXT(3)
GLOBAL_UNCERTAINTY_ASSIGNED_CONTEXT((#47696))
GLOBAL_UNIT_ASSIGNED_CONTEXT((#47718,#47720,#47721))
REPRESENTATION_CONTEXT('','3D')
);
#47711=(
GEOMETRIC_REPRESENTATION_CONTEXT(3)
GLOBAL_UNCERTAINTY_ASSIGNED_CONTEXT((#47697))
GLOBAL_UNIT_ASSIGNED_CONTEXT((#47718,#47720,#47721))
REPRESENTATION_CONTEXT('','3D')
);
#47712=(
GEOMETRIC_REPRESENTATION_CONTEXT(3)
GLOBAL_UNCERTAINTY_ASSIGNED_CONTEXT((#47698))
GLOBAL_UNIT_ASSIGNED_CONTEXT((#47718,#47720,#47721))
REPRESENTATION_CONTEXT('','3D')
);
#47713=(
GEOMETRIC_REPRESENTATION_CONTEXT(3)
GLOBAL_UNCERTAINTY_ASSIGNED_CONTEXT((#47699))
GLOBAL_UNIT_ASSIGNED_CONTEXT((#47718,#47720,#47721))
REPRESENTATION_CONTEXT('','3D')
);
#47714=(
GEOMETRIC_REPRESENTATION_CONTEXT(3)
GLOBAL_UNCERTAINTY_ASSIGNED_CONTEXT((#47700))
GLOBAL_UNIT_ASSIGNED_CONTEXT((#47718,#47720,#47721))
REPRESENTATION_CONTEXT('','3D')
);
#47715=(
GEOMETRIC_REPRESENTATION_CONTEXT(3)
GLOBAL_UNCERTAINTY_ASSIGNED_CONTEXT((#47701))
GLOBAL_UNIT_ASSIGNED_CONTEXT((#47718,#47720,#47721))
REPRESENTATION_CONTEXT('','3D')
);
#47716=(
GEOMETRIC_REPRESENTATION_CONTEXT(3)
GLOBAL_UNCERTAINTY_ASSIGNED_CONTEXT((#47702))
GLOBAL_UNIT_ASSIGNED_CONTEXT((#47718,#47720,#47721))
REPRESENTATION_CONTEXT('','3D')
);
#47717=(
GEOMETRIC_REPRESENTATION_CONTEXT(3)
GLOBAL_UNCERTAINTY_ASSIGNED_CONTEXT((#47703))
GLOBAL_UNIT_ASSIGNED_CONTEXT((#47718,#47720,#47721))
REPRESENTATION_CONTEXT('','3D')
);
#47718=(
LENGTH_UNIT()
NAMED_UNIT(*)
SI_UNIT(.MILLI.,.METRE.)
);
#47719=(
LENGTH_UNIT()
NAMED_UNIT(*)
SI_UNIT($,.METRE.)
);
#47720=(
NAMED_UNIT(*)
PLANE_ANGLE_UNIT()
SI_UNIT($,.RADIAN.)
);
#47721=(
NAMED_UNIT(*)
SI_UNIT($,.STERADIAN.)
SOLID_ANGLE_UNIT()
);
#47722=SHAPE_DEFINITION_REPRESENTATION(#47735,#47760);
#47723=SHAPE_DEFINITION_REPRESENTATION(#47736,#47761);
#47724=SHAPE_DEFINITION_REPRESENTATION(#47737,#47762);
#47725=SHAPE_DEFINITION_REPRESENTATION(#47738,#47763);
#47726=SHAPE_DEFINITION_REPRESENTATION(#47739,#47764);
#47727=SHAPE_DEFINITION_REPRESENTATION(#47740,#47765);
#47728=SHAPE_DEFINITION_REPRESENTATION(#47741,#47766);
#47729=SHAPE_DEFINITION_REPRESENTATION(#47742,#47767);
#47730=SHAPE_DEFINITION_REPRESENTATION(#47743,#47768);
#47731=SHAPE_DEFINITION_REPRESENTATION(#47744,#47769);
#47732=SHAPE_DEFINITION_REPRESENTATION(#47745,#47770);
#47733=SHAPE_DEFINITION_REPRESENTATION(#47746,#47771);
#47734=SHAPE_DEFINITION_REPRESENTATION(#47747,#47772);
#47735=PRODUCT_DEFINITION_SHAPE('',$,#47774);
#47736=PRODUCT_DEFINITION_SHAPE('',$,#47775);
#47737=PRODUCT_DEFINITION_SHAPE('',$,#47776);
#47738=PRODUCT_DEFINITION_SHAPE('',$,#47777);
#47739=PRODUCT_DEFINITION_SHAPE('',$,#47778);
#47740=PRODUCT_DEFINITION_SHAPE('',$,#47779);
#47741=PRODUCT_DEFINITION_SHAPE('',$,#47780);
#47742=PRODUCT_DEFINITION_SHAPE('',$,#47781);
#47743=PRODUCT_DEFINITION_SHAPE('',$,#47782);
#47744=PRODUCT_DEFINITION_SHAPE('',$,#47783);
#47745=PRODUCT_DEFINITION_SHAPE('',$,#47784);
#47746=PRODUCT_DEFINITION_SHAPE('',$,#47785);
#47747=PRODUCT_DEFINITION_SHAPE('',$,#47786);
#47748=PRODUCT_DEFINITION_SHAPE($,$,#47);
#47749=PRODUCT_DEFINITION_SHAPE($,$,#48);
#47750=PRODUCT_DEFINITION_SHAPE($,$,#49);
#47751=PRODUCT_DEFINITION_SHAPE($,$,#50);
#47752=PRODUCT_DEFINITION_SHAPE($,$,#51);
#47753=PRODUCT_DEFINITION_SHAPE($,$,#52);
#47754=PRODUCT_DEFINITION_SHAPE($,$,#53);
#47755=PRODUCT_DEFINITION_SHAPE($,$,#54);
#47756=PRODUCT_DEFINITION_SHAPE($,$,#55);
#47757=PRODUCT_DEFINITION_SHAPE($,$,#56);
#47758=PRODUCT_DEFINITION_SHAPE($,$,#57);
#47759=PRODUCT_DEFINITION_SHAPE($,$,#58);
#47760=SHAPE_REPRESENTATION('',(#9070,#9944,#9945,#9946,#9947,#9948,#9949,
#9950,#9951,#9952,#9953,#9954,#9955),#47704);
#47761=SHAPE_REPRESENTATION('',(#9071),#47705);
#47762=SHAPE_REPRESENTATION('',(#9081),#47706);
#47763=SHAPE_REPRESENTATION('',(#9112),#47707);
#47764=SHAPE_REPRESENTATION('',(#9122),#47708);
#47765=SHAPE_REPRESENTATION('',(#9345),#47709);
#47766=SHAPE_REPRESENTATION('',(#9511),#47710);
#47767=SHAPE_REPRESENTATION('',(#9515),#47711);
#47768=SHAPE_REPRESENTATION('',(#9703),#47712);
#47769=SHAPE_REPRESENTATION('',(#9812),#47713);
#47770=SHAPE_REPRESENTATION('',(#9824),#47714);
#47771=SHAPE_REPRESENTATION('',(#9834),#47715);
#47772=SHAPE_REPRESENTATION('',(#9871),#47716);
#47773=PRODUCT_DEFINITION_CONTEXT('part definition',#47814,'design');
#47774=PRODUCT_DEFINITION('locking pliers','MAS-610',#47787,
#47773);
#47775=PRODUCT_DEFINITION('Pivot Pins','Pivot Pins',#47788,#47773);
#47776=PRODUCT_DEFINITION('Tension Spring','Tension Spring',#47789,#47773);
#47777=PRODUCT_DEFINITION('Pivot Pins 3','Pivot Pins 3',#47790,#47773);
#47778=PRODUCT_DEFINITION('Upper Handle Fixed Jaw',
'Upper Handle Fixed Jaw',#47791,#47773);
#47779=PRODUCT_DEFINITION('Adjustment Screw','Adjustment Screw',#47792,
#47773);
#47780=PRODUCT_DEFINITION('Pivot Block','Pivot Block',#47793,#47773);
#47781=PRODUCT_DEFINITION('Movable Jaw','Movable Jaw',#47794,#47773);
#47782=PRODUCT_DEFINITION('Lower Handle','Lower Handle',#47795,#47773);
#47783=PRODUCT_DEFINITION('small pin','Small Pin',#47796,#47773);
#47784=PRODUCT_DEFINITION('Pivot Pins 2','Pivot Pins 2',#47797,#47773);
#47785=PRODUCT_DEFINITION('Release Lever','Release Lever',#47798,#47773);
#47786=PRODUCT_DEFINITION('Link Lever','Link Lever',#47799,#47773);
#47787=PRODUCT_DEFINITION_FORMATION('',$,#47816);
#47788=PRODUCT_DEFINITION_FORMATION('',$,#47817);
#47789=PRODUCT_DEFINITION_FORMATION('',$,#47818);
#47790=PRODUCT_DEFINITION_FORMATION('',$,#47819);
#47791=PRODUCT_DEFINITION_FORMATION('',$,#47820);
#47792=PRODUCT_DEFINITION_FORMATION('',$,#47821);
#47793=PRODUCT_DEFINITION_FORMATION('',$,#47822);
#47794=PRODUCT_DEFINITION_FORMATION('',$,#47823);
#47795=PRODUCT_DEFINITION_FORMATION('',$,#47824);
#47796=PRODUCT_DEFINITION_FORMATION('',$,#47825);
#47797=PRODUCT_DEFINITION_FORMATION('',$,#47826);
#47798=PRODUCT_DEFINITION_FORMATION('',$,#47827);
#47799=PRODUCT_DEFINITION_FORMATION('',$,#47828);
#47800=PRODUCT_RELATED_PRODUCT_CATEGORY('MAS-610',
'MAS-610',(#47816));
#47801=PRODUCT_RELATED_PRODUCT_CATEGORY('Pivot Pins','Pivot Pins',(#47817));
#47802=PRODUCT_RELATED_PRODUCT_CATEGORY('Tension Spring',
'Tension Spring',(#47818));
#47803=PRODUCT_RELATED_PRODUCT_CATEGORY('Pivot Pins 3','Pivot Pins 3',(#47819));
#47804=PRODUCT_RELATED_PRODUCT_CATEGORY('Upper Handle Fixed Jaw',
'Upper Handle Fixed Jaw',(#47820));
#47805=PRODUCT_RELATED_PRODUCT_CATEGORY('Adjustment Screw',
'Adjustment Screw',(#47821));
#47806=PRODUCT_RELATED_PRODUCT_CATEGORY('Pivot Block','Pivot Block',(#47822));
#47807=PRODUCT_RELATED_PRODUCT_CATEGORY('Movable Jaw','Movable Jaw',(#47823));
#47808=PRODUCT_RELATED_PRODUCT_CATEGORY('Lower Handle','Lower Handle',(#47824));
#47809=PRODUCT_RELATED_PRODUCT_CATEGORY('Small Pin','Small Pin',(#47825));
#47810=PRODUCT_RELATED_PRODUCT_CATEGORY('Pivot Pins 2','Pivot Pins 2',(#47826));
#47811=PRODUCT_RELATED_PRODUCT_CATEGORY('Release Lever','Release Lever',
(#47827));
#47812=PRODUCT_RELATED_PRODUCT_CATEGORY('Link Lever','Link Lever',(#47828));
#47813=APPLICATION_PROTOCOL_DEFINITION('international standard',
'automotive_design',2009,#47814);
#47814=APPLICATION_CONTEXT(
'Core Data for Automotive Mechanical Design Process');
#47815=PRODUCT_CONTEXT('part definition',#47814,'mechanical');
#47816=PRODUCT('locking pliers','MAS-610','STEP AP214',(#47815));
#47817=PRODUCT('Pivot Pins','Pivot Pins',$,(#47815));
#47818=PRODUCT('Tension Spring','Tension Spring',$,(#47815));
#47819=PRODUCT('Pivot Pins 3','Pivot Pins 3',$,(#47815));
#47820=PRODUCT('Upper Handle Fixed Jaw','Upper Handle Fixed Jaw',$,(#47815));
#47821=PRODUCT('Adjustment Screw','Adjustment Screw',$,(#47815));
#47822=PRODUCT('Pivot Block','Pivot Block',$,(#47815));
#47823=PRODUCT('Movable Jaw','Movable Jaw',$,(#47815));
#47824=PRODUCT('Lower Handle','Lower Handle',$,(#47815));
#47825=PRODUCT('small pin','Small Pin',$,(#47815));
#47826=PRODUCT('Pivot Pins 2','Pivot Pins 2',$,(#47815));
#47827=PRODUCT('Release Lever','Release Lever',$,(#47815));
#47828=PRODUCT('Link Lever','Link Lever',$,(#47815));
#47829=PRESENTATION_STYLE_ASSIGNMENT((#47831));
#47830=PRESENTATION_STYLE_ASSIGNMENT((#47832));
#47831=SURFACE_STYLE_USAGE(.BOTH.,#47833);
#47832=SURFACE_STYLE_USAGE(.BOTH.,#47834);
#47833=SURFACE_SIDE_STYLE('',(#47835));
#47834=SURFACE_SIDE_STYLE('',(#47836));
#47835=SURFACE_STYLE_FILL_AREA(#47837);
#47836=SURFACE_STYLE_FILL_AREA(#47838);
#47837=FILL_AREA_STYLE('Steel - Satin',(#47839));
#47838=FILL_AREA_STYLE('Opaque(202,209,238)',(#47840));
#47839=FILL_AREA_STYLE_COLOUR('Steel - Satin',#47841);
#47840=FILL_AREA_STYLE_COLOUR('Opaque(202,209,238)',#47842);
#47841=COLOUR_RGB('Steel - Satin', 0.66274510, 0.83137255, 0.94901961);
#47842=COLOUR_RGB('Opaque(202,209,238)', 0.66274510, 0.83137255, 0.94901961);
ENDSEC;
END-ISO-10303-21;
